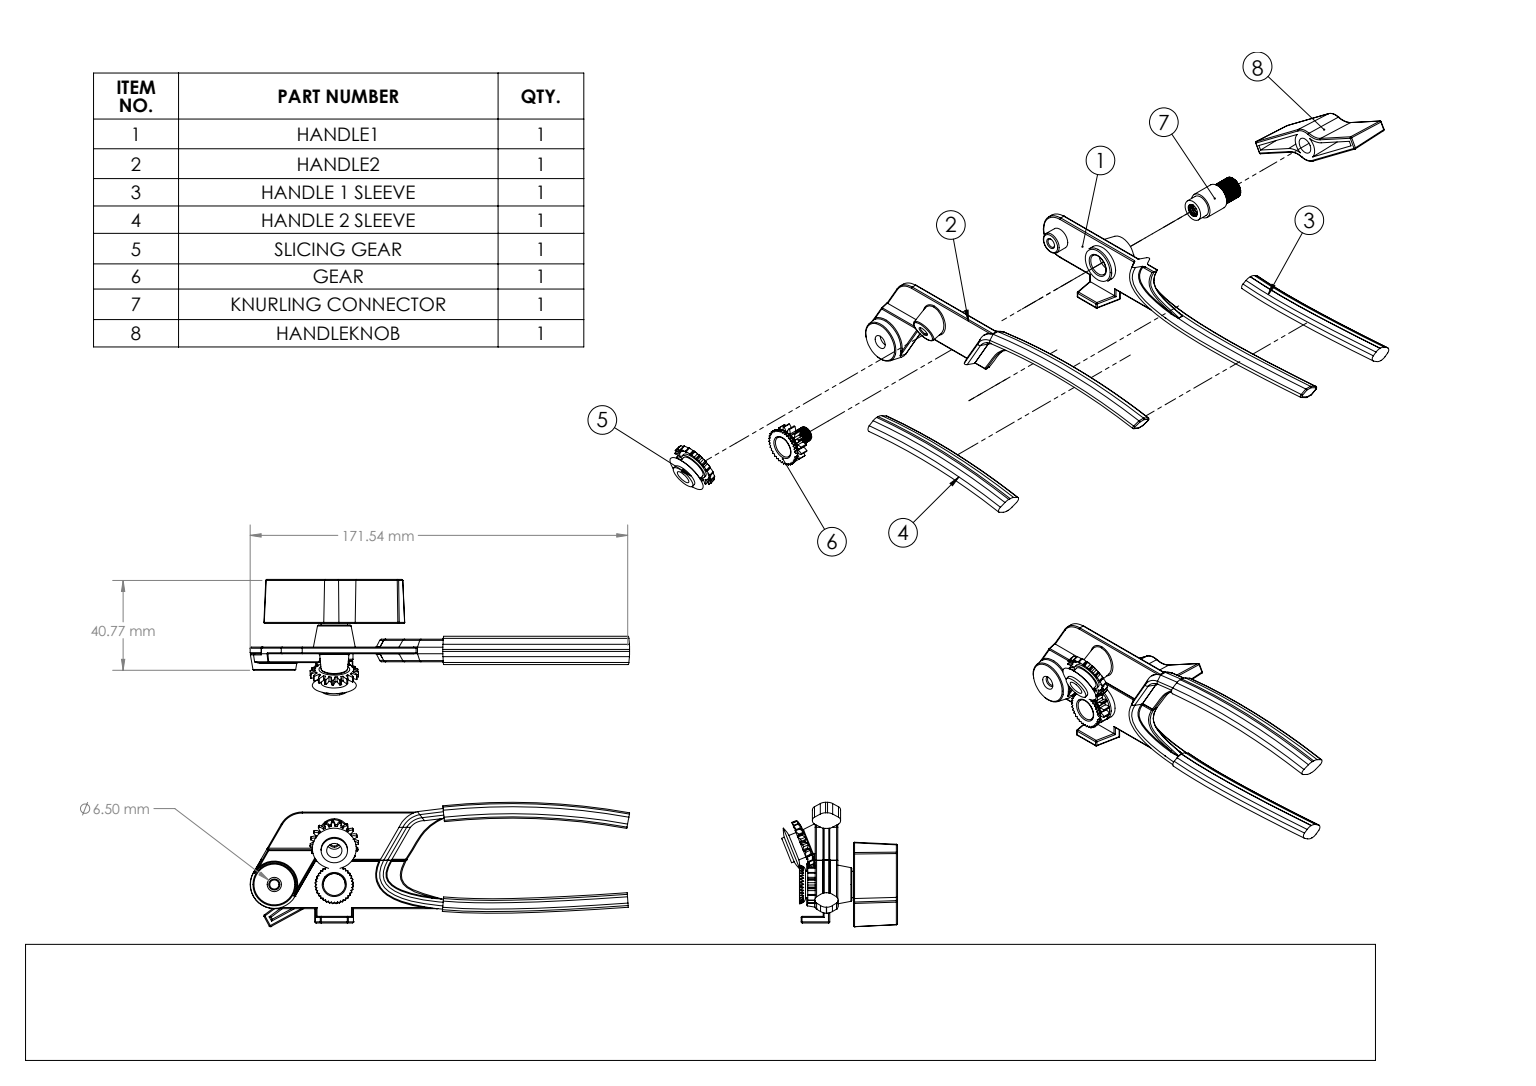
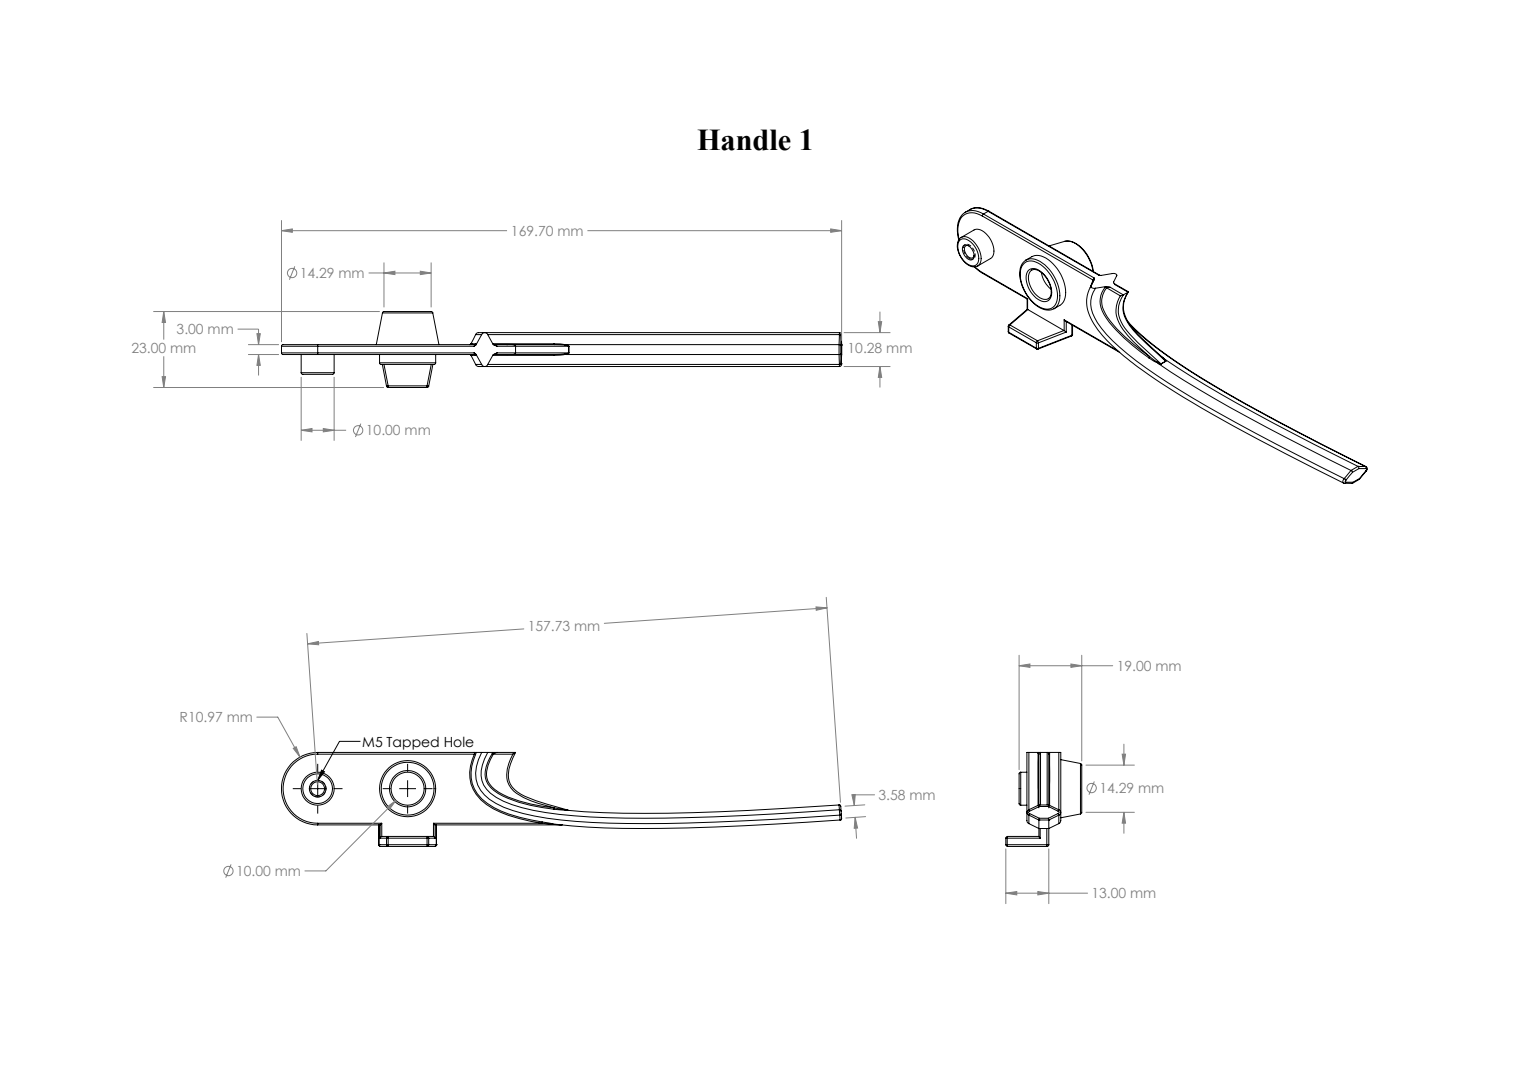
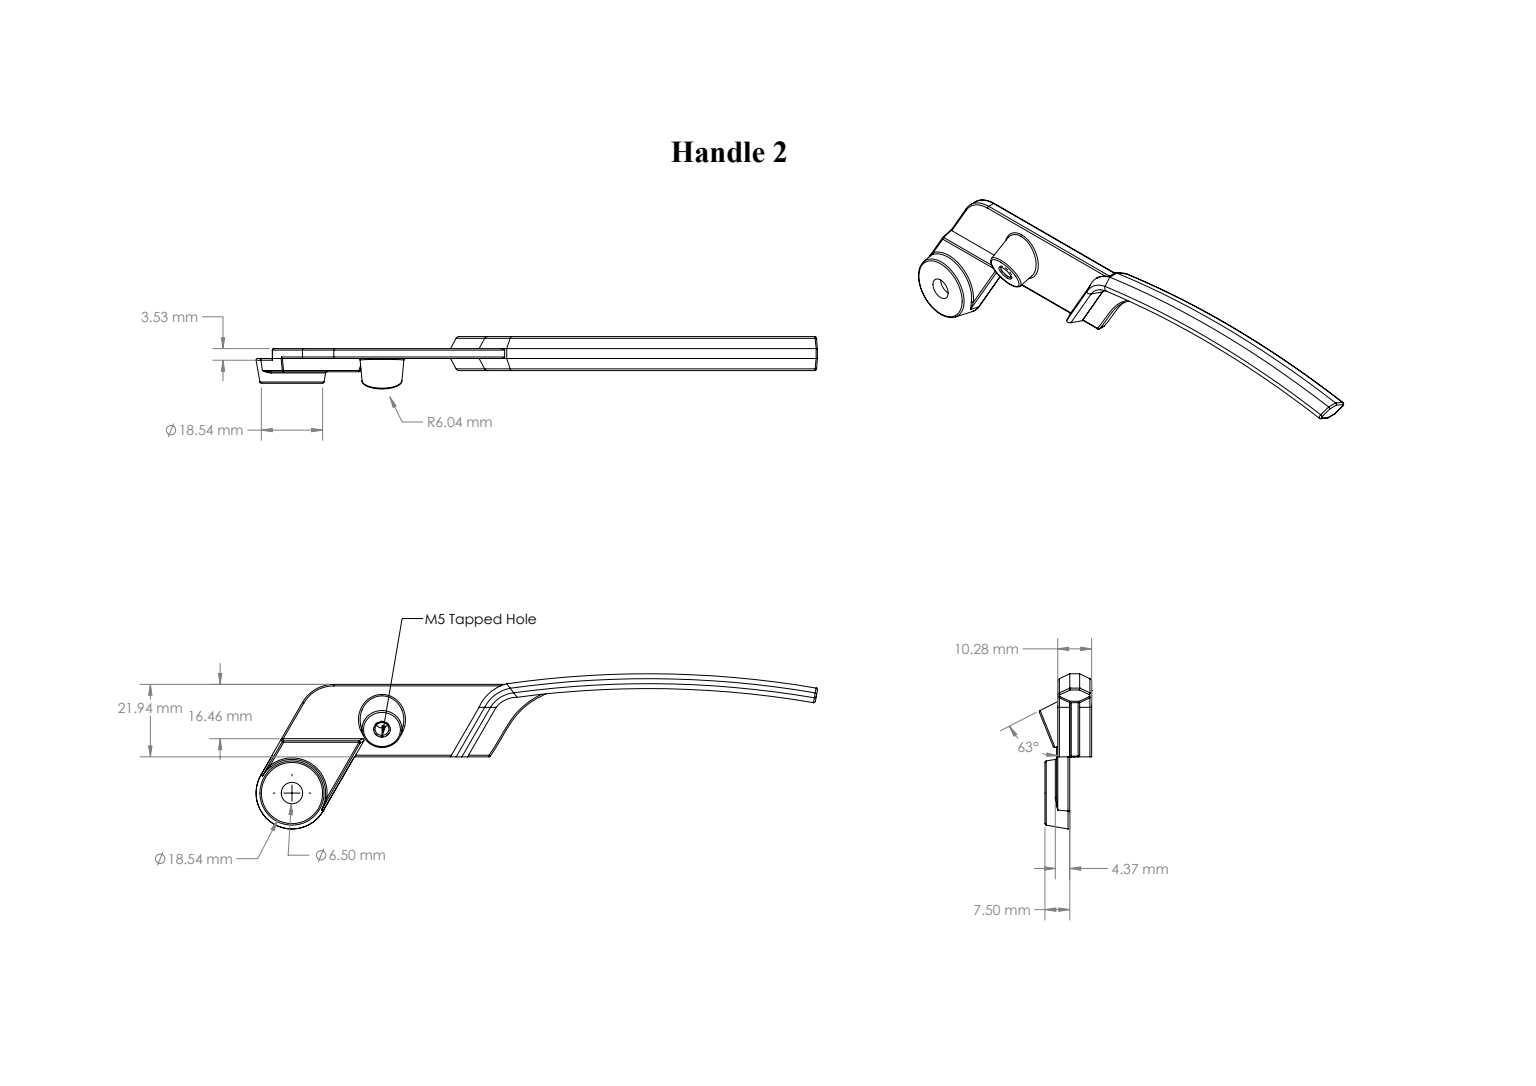
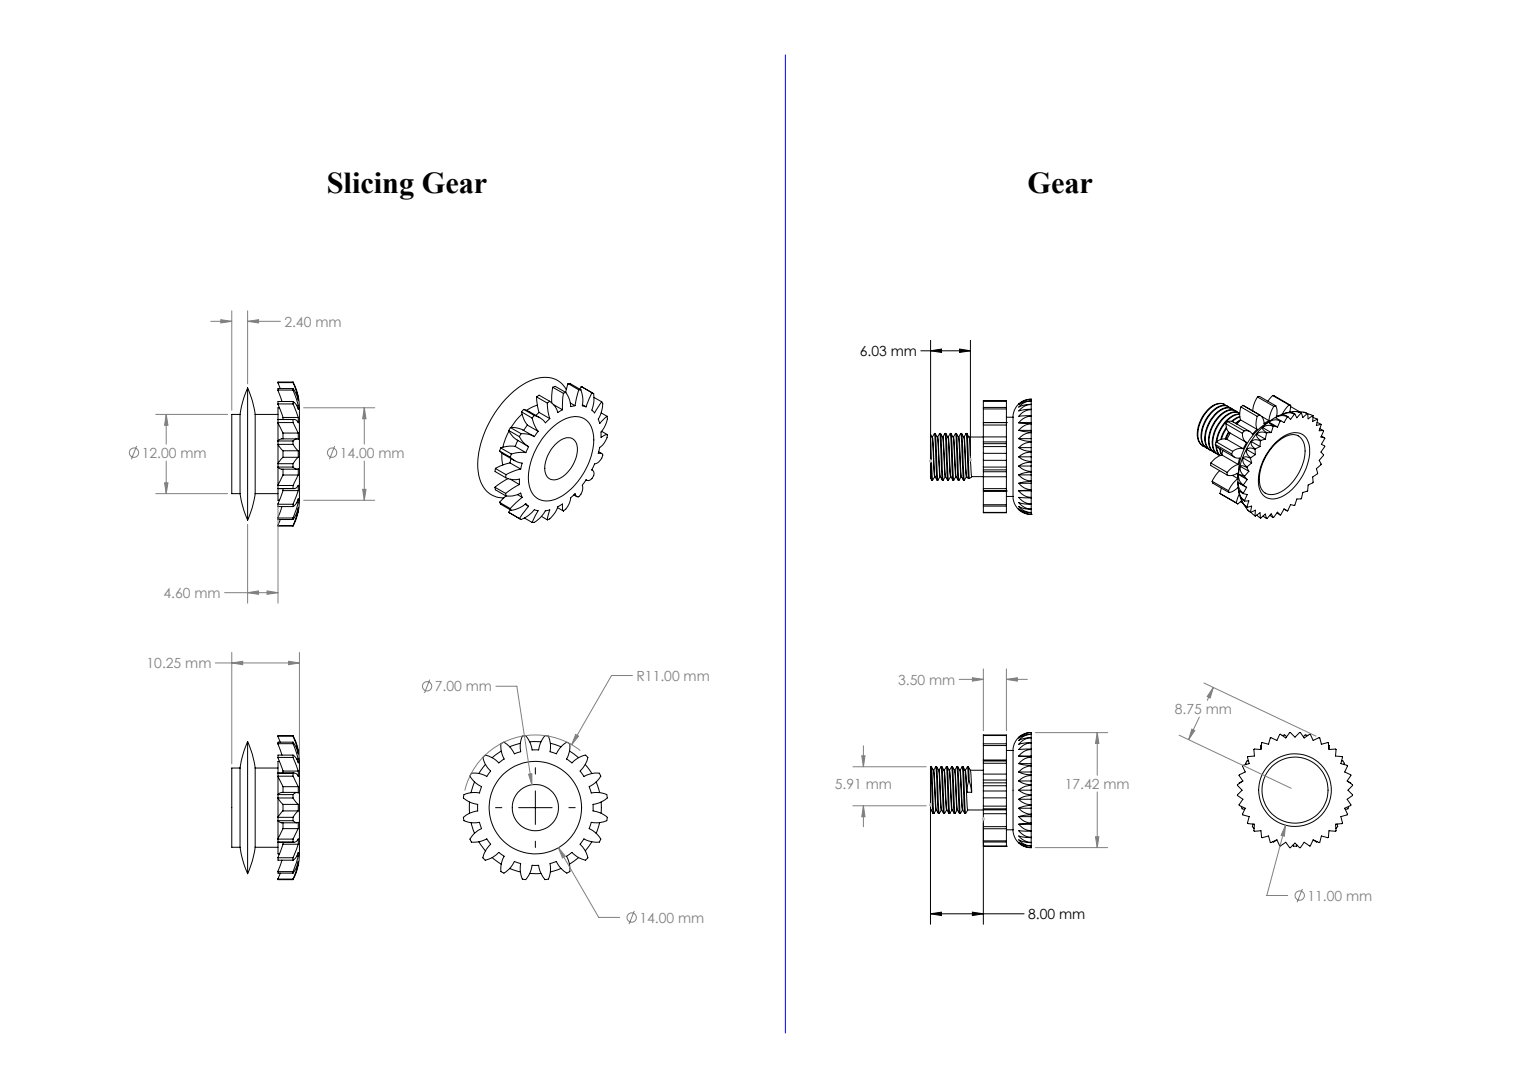
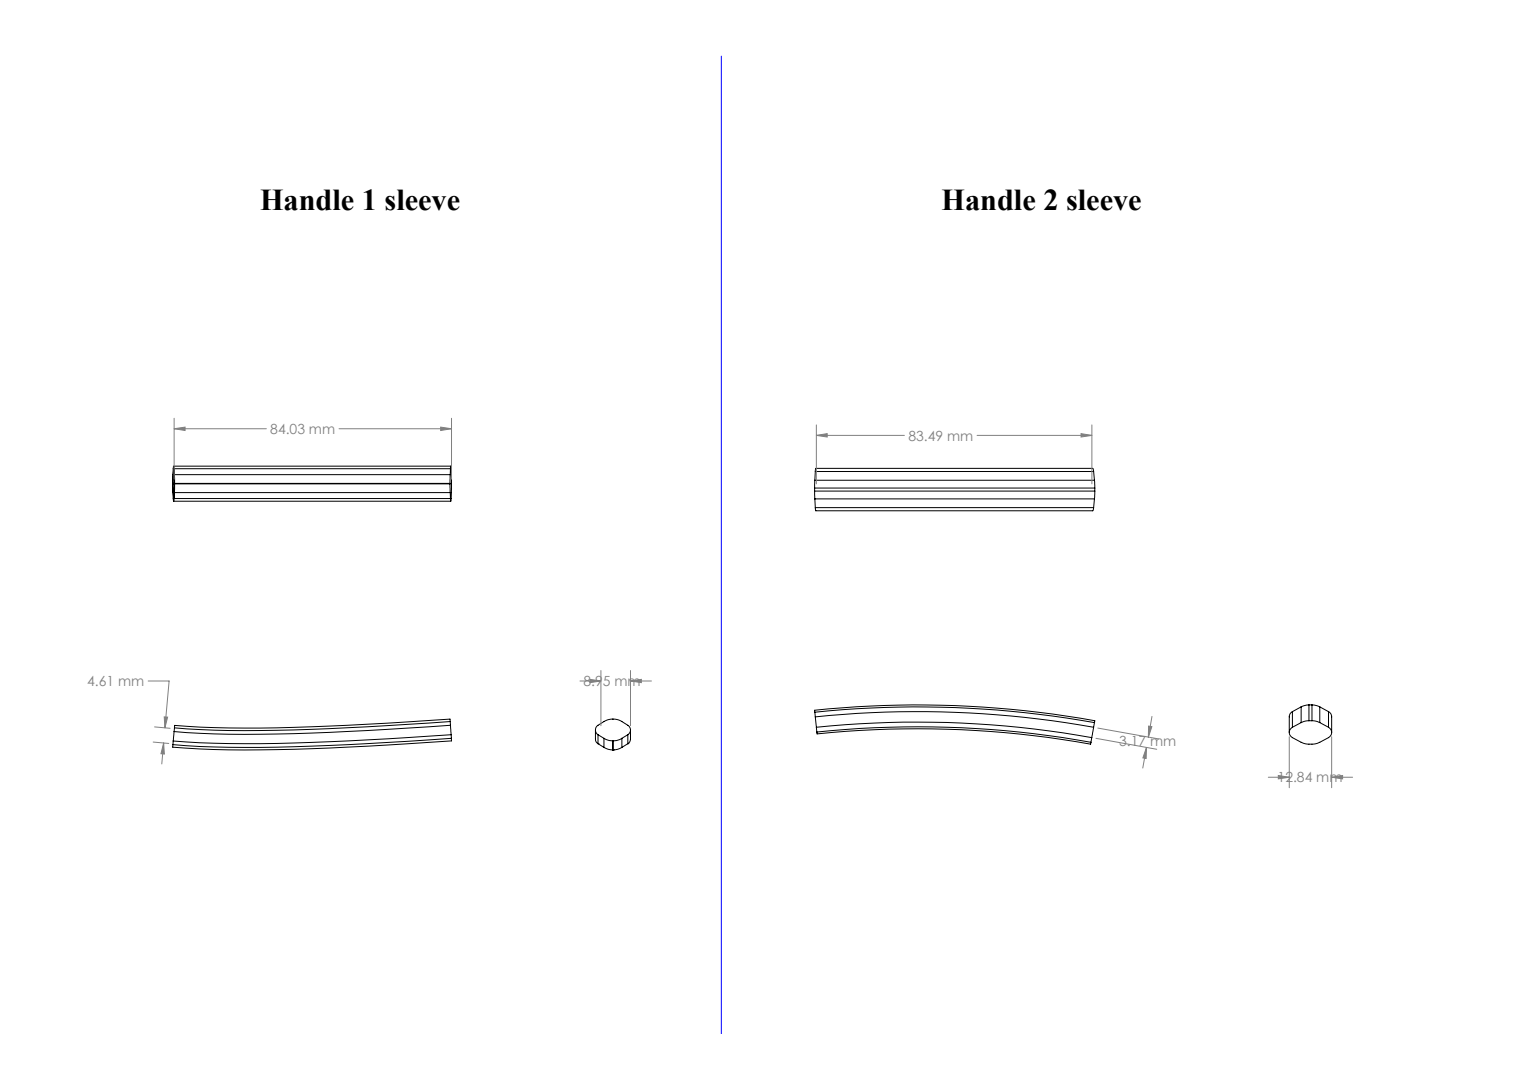
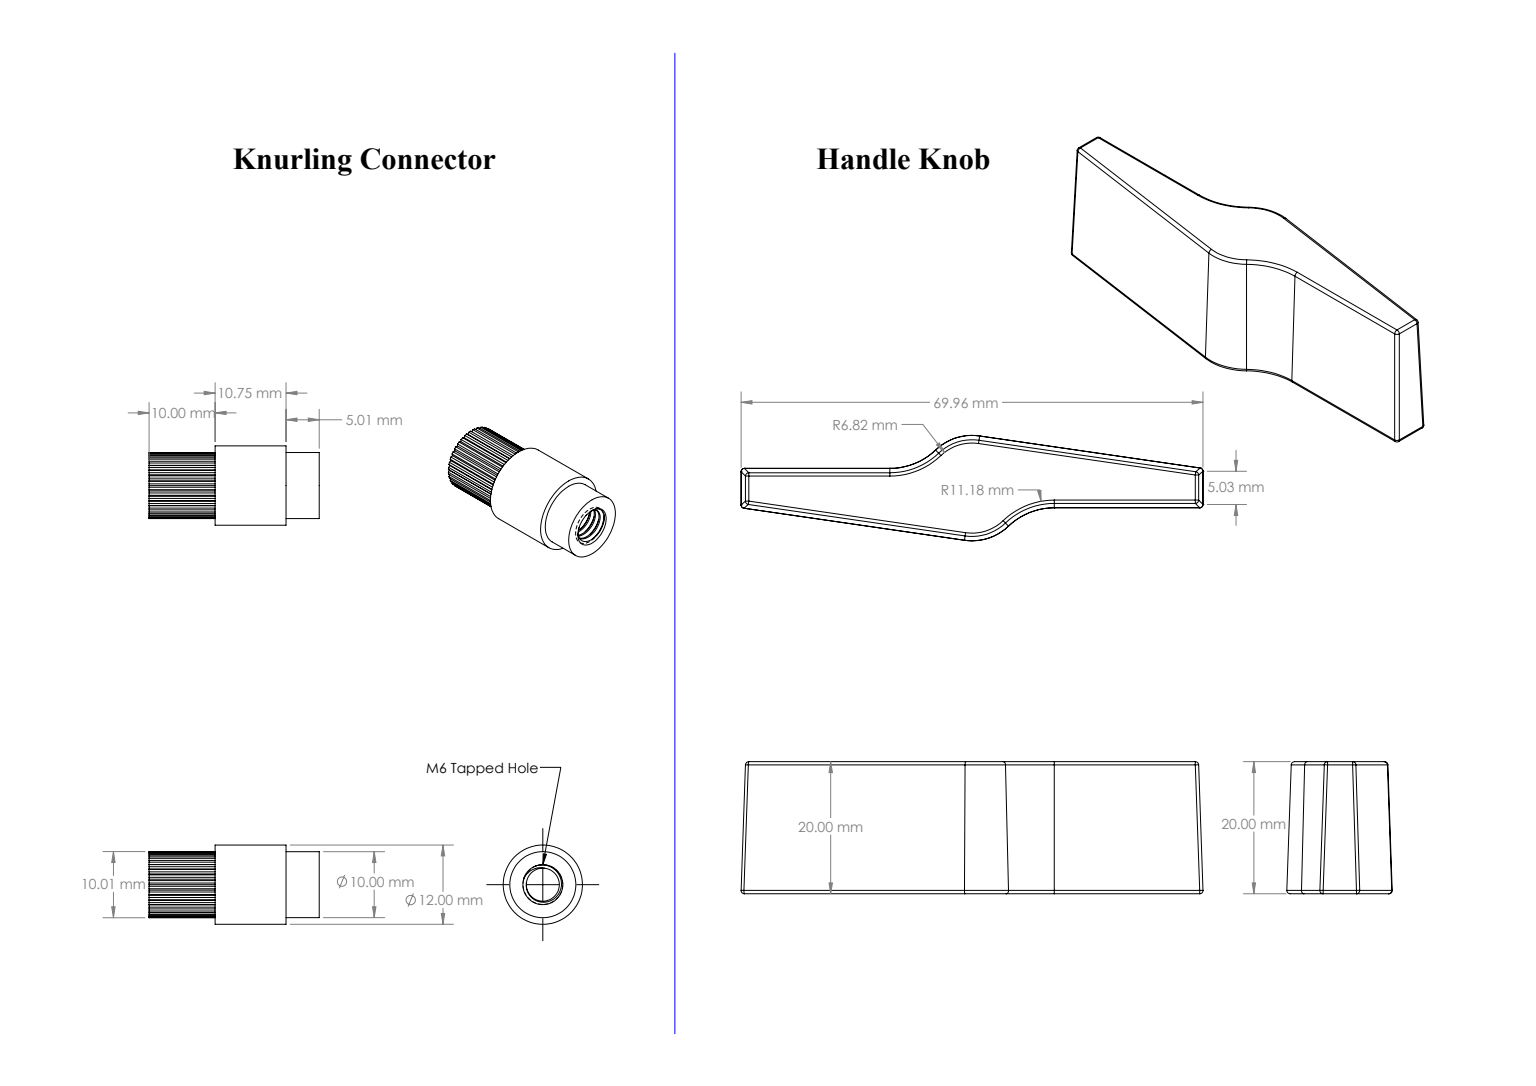
ISO-10303-21;
HEADER;
FILE_DESCRIPTION (('STEP AP203'),
    '1' );
FILE_NAME ('MAS-163',
    '2026-10-06T15:07:10',
    ( '' ),
    ( '' ),
    'SwSTEP 2.0',
    'SolidWorks 2024',
    '' );
FILE_SCHEMA (( 'AUTOMOTIVE_DESIGN' ));
ENDSEC;

DATA;
#1 = ADVANCED_FACE ( 'NONE', ( #10434 ), #18456, .F. ) ;
#2 = CARTESIAN_POINT ( 'NONE',  ( 54.89716490668163118, -3.628845007888942931, 0.07017451552782483226 ) ) ;
#3 = CARTESIAN_POINT ( 'NONE',  ( -8.000050800000000351, 3.673940397442060361E-16, 3.000000000000000444 ) ) ;
#4 = ORIENTED_EDGE ( 'NONE', *, *, #27611, .T. ) ;
#5 = DIRECTION ( 'NONE',  ( 1.000000000000000000, -0.000000000000000000, 0.000000000000000000 ) ) ;
#6 = EDGE_CURVE ( 'NONE', #31023, #30399, #20030, .T. ) ;
#7 = AXIS2_PLACEMENT_3D ( 'NONE', #248, #30174, #22638 ) ;
#8 = AXIS2_PLACEMENT_3D ( 'NONE', #3231, #13394, #23612 ) ;
#9 = APPLICATION_PROTOCOL_DEFINITION ( 'international standard', 'config_control_design', 1994, #20608 ) ;
#10 = CARTESIAN_POINT ( 'NONE',  ( 18.75828436641558028, -5.879118399717574661, -3.993434336035625254 ) ) ;
#11 = VERTEX_POINT ( 'NONE', #9811 ) ;
#12 = AXIS2_PLACEMENT_3D ( 'NONE', #13774, #23975, #1092 ) ;
#13 = SHAPE_REPRESENTATION ( 'Part5_knurlingConnector', ( #2865 ), #13509 ) ;
#14 = DIRECTION ( 'NONE',  ( 0.000000000000000000, 1.000000000000000000, 0.000000000000000000 ) ) ;
#15 = ORIENTED_EDGE ( 'NONE', *, *, #21559, .T. ) ;
#16 = CARTESIAN_POINT ( 'NONE',  ( -21.76338877130672245, 18.20021209127403239, 1.779283699008895159 ) ) ;
#18 = ORIENTED_EDGE ( 'NONE', *, *, #3562, .F. ) ;
#17 = CARTESIAN_POINT ( 'NONE',  ( 69.01456695820279208, -4.997110861600952525, -4.033870539711066350 ) ) ;
#19 = ORIENTED_EDGE ( 'NONE', *, *, #12026, .T. ) ;
#20 = CARTESIAN_POINT ( 'NONE',  ( -2.511343449419941365, -0.3178988483021044087, 3.024605502323848949 ) ) ;
#21 = CARTESIAN_POINT ( 'NONE',  ( 10.57125986779756843, 4.681538312723516171, 0.8254815157535410064 ) ) ;
#22 = DIRECTION ( 'NONE',  ( 0.000000000000000000, 1.000000000000000000, 0.000000000000000000 ) ) ;
#23 = EDGE_CURVE ( 'NONE', #10880, #2577, #7296, .T. ) ;
#24 = FACE_OUTER_BOUND ( 'NONE', #30613, .T. ) ;
#25 = CC_DESIGN_DATE_AND_TIME_ASSIGNMENT ( #14013, #6672, ( #1036 ) ) ;
#27 = ORIENTED_EDGE ( 'NONE', *, *, #10830, .T. ) ;
#26 = FACE_OUTER_BOUND ( 'NONE', #27997, .T. ) ;
#28 = DIRECTION ( 'NONE',  ( -1.000000000000000000, -0.000000000000000000, 0.000000000000000000 ) ) ;
#29 = CARTESIAN_POINT ( 'NONE',  ( 26.04699060503310193, 19.53185396608588320, 1.500000000000000000 ) ) ;
#30 = CARTESIAN_POINT ( 'NONE',  ( -3.423602242323041001, -10.69107769603132674, 1.500000000000237144 ) ) ;
#31 = CARTESIAN_POINT ( 'NONE',  ( 2.717504505341735932, -0.4236608596156870021, 1.500000000000000000 ) ) ;
#33 = ORIENTED_EDGE ( 'NONE', *, *, #17651, .T. ) ;
#32 = CARTESIAN_POINT ( 'NONE',  ( 107.5624060836778426, -18.99272400518356463, -4.497198431447757550 ) ) ;
#34 = DIRECTION ( 'NONE',  ( -0.000000000000000000, -0.000000000000000000, 1.000000000000000000 ) ) ;
#35 = AXIS2_PLACEMENT_3D ( 'NONE', #30229, #18289, #20649 ) ;
#36 = AXIS2_PLACEMENT_3D ( 'NONE', #29138, #6225, #23788 ) ;
#37 = B_SPLINE_CURVE_WITH_KNOTS ( 'NONE', 3,
 ( #24439, #32167, #19463, #16927, #1731, #20453, #20272, #30474 ),
 .UNSPECIFIED., .F., .F.,
 ( 4, 2, 2, 4 ),
 ( 2.304311362529957687E-07, 0.001227991214883143506, 0.001841871606756588465, 0.002455751998630033642 ),
 .UNSPECIFIED. ) ;
#38 = DIRECTION ( 'NONE',  ( 1.000000000000000000, -8.574039729943018344E-17, -0.000000000000000000 ) ) ;
#39 = CARTESIAN_POINT ( 'NONE',  ( 23.86000000273118715, -1.942864903642428587, -1.573300977624592756 ) ) ;
#40 = AXIS2_PLACEMENT_3D ( 'NONE', #21836, #32050, #26400 ) ;
#41 = EDGE_CURVE ( 'NONE', #3413, #15831, #25636, .T. ) ;
#42 = DIRECTION ( 'NONE',  ( 0.000000000000000000, 1.000000000000000000, 0.000000000000000000 ) ) ;
#43 = CARTESIAN_POINT ( 'NONE',  ( -8.000050800000000351, 0.000000000000000000, 0.000000000000000000 ) ) ;
#44 = CARTESIAN_POINT ( 'NONE',  ( -2.880987360464337677, -0.6119841066606566127, -1.499999999999999334 ) ) ;
#45 = VECTOR ( 'NONE', #11499, 1000.000000000000000 ) ;
#46 = EDGE_LOOP ( 'NONE', ( #17358, #23961, #2698, #31842 ) ) ;
#47 = DIRECTION ( 'NONE',  ( 0.000000000000000000, -0.4226182617406998299, -0.9063077870366498257 ) ) ;
#48 = LINE ( 'NONE', #23124, #20445 ) ;
#49 = CARTESIAN_POINT ( 'NONE',  ( -6.387550801365593500, 3.521866450007987037, 0.3701630799359328372 ) ) ;
#50 = ORIENTED_EDGE ( 'NONE', *, *, #20292, .T. ) ;
#51 = DIRECTION ( 'NONE',  ( 6.062761635205658338E-17, 0.7071067811865558994, -0.7071067811865391350 ) ) ;
#52 = AXIS2_PLACEMENT_3D ( 'NONE', #22887, #28230, #10168 ) ;
#53 = DIRECTION ( 'NONE',  ( 0.000000000000000000, -0.7071067811865380248, -0.7071067811865570096 ) ) ;
#54 = VECTOR ( 'NONE', #11765, 999.9999999999998863 ) ;
#55 = CARTESIAN_POINT ( 'NONE',  ( 2.117172266158220406, -1.242920418748501676, -0.9788672205888330202 ) ) ;
#56 = CARTESIAN_POINT ( 'NONE',  ( 19.46884934643044929, -15.80146560116522991, 1.000000000000000000 ) ) ;
#57 = EDGE_LOOP ( 'NONE', ( #2228, #29495, #10201, #20358 ) ) ;
#58 = CIRCLE ( 'NONE', #27352, 8.500000000000000000 ) ;
#59 = CIRCLE ( 'NONE', #14435, 12.62979293944910353 ) ;
#60 = CARTESIAN_POINT ( 'NONE',  ( -40.65244704454411107, -12.44919619934167088, 5.499999999999999112 ) ) ;
#61 = VERTEX_POINT ( 'NONE', #14078 ) ;
#62 = CARTESIAN_POINT ( 'NONE',  ( -2.655659815844460869, 0.1700350810717016214, 1.254089647469669000 ) ) ;
#64 = ORIENTED_EDGE ( 'NONE', *, *, #2032, .F. ) ;
#63 = DIRECTION ( 'NONE',  ( 0.000000000000000000, -0.000000000000000000, -1.000000000000000000 ) ) ;
#65 = ORIENTED_EDGE ( 'NONE', *, *, #16539, .T. ) ;
#66 = DIRECTION ( 'NONE',  ( 0.000000000000000000, -0.7071067811865455743, -0.7071067811865495711 ) ) ;
#67 = ADVANCED_FACE ( 'NONE', ( #1394 ), #31658, .F. ) ;
#68 = EDGE_LOOP ( 'NONE', ( #22629, #18065, #11744, #10106 ) ) ;
#70 = VECTOR ( 'NONE', #32626, 1000.000000000000000 ) ;
#69 = CARTESIAN_POINT ( 'NONE',  ( 5.612718761614564400, -7.013540705848206436, 4.279483796479000013 ) ) ;
#72 = VERTEX_POINT ( 'NONE', #1047 ) ;
#71 = DIRECTION ( 'NONE',  ( 0.000000000000000000, 0.9961946980917452121, 0.08715574274766296758 ) ) ;
#73 = CARTESIAN_POINT ( 'NONE',  ( 0.8174907777731121872, -3.242754804592638429, -1.762319835267122992 ) ) ;
#74 = CARTESIAN_POINT ( 'NONE',  ( 0.9232102171129921153, 0.000000000000000000, 4.522129901861157819 ) ) ;
#75 = CARTESIAN_POINT ( 'NONE',  ( 10.57125986779756843, -1.115095498423343878, 4.884328206559833241 ) ) ;
#76 = DIRECTION ( 'NONE',  ( -1.000000000000000000, -0.000000000000000000, -0.000000000000000000 ) ) ;
#77 = AXIS2_PLACEMENT_3D ( 'NONE', #24647, #7270, #1946 ) ;
#78 = DIRECTION ( 'NONE',  ( -0.000000000000000000, -0.000000000000000000, -1.000000000000000000 ) ) ;
#79 = CARTESIAN_POINT ( 'NONE',  ( 0.6738579927983930906, -5.220872085256825557, 1.499999999999999556 ) ) ;
#80 = FACE_OUTER_BOUND ( 'NONE', #3087, .T. ) ;
#81 = ADVANCED_FACE ( 'NONE', ( #26310 ), #21929, .F. ) ;
#82 = EDGE_CURVE ( 'NONE', #20879, #12815, #17217, .T. ) ;
#83 = AXIS2_PLACEMENT_3D ( 'NONE', #30124, #5184, #17706 ) ;
#84 = VECTOR ( 'NONE', #19365, 1000.000000000000227 ) ;
#85 = PLANE ( 'NONE',  #10726 ) ;
#86 = CARTESIAN_POINT ( 'NONE',  ( 101.9216173105994159, -5.769792427975438898, -0.07017451552783579571 ) ) ;
#87 = DIRECTION ( 'NONE',  ( 4.458171167563049465E-29, -1.000000000000000000, -5.782411586589359611E-15 ) ) ;
#88 = CARTESIAN_POINT ( 'NONE',  ( 54.64624227588102201, -3.635739347938791610, 0.02339150516273077324 ) ) ;
#89 = CIRCLE ( 'NONE', #23575, 2.099999999999997868 ) ;
#90 = EDGE_CURVE ( 'NONE', #31165, #31196, #18949, .T. ) ;
#91 = CIRCLE ( 'NONE', #29457, 2.999999999999999112 ) ;
#92 = CARTESIAN_POINT ( 'NONE',  ( 7.249760686538667009, -2.789499415801756586E-14, 8.014274990069656823 ) ) ;
#93 = CARTESIAN_POINT ( 'NONE',  ( 9.999999999999998224, -4.753758587302148619, -3.462581523170091167E-33 ) ) ;
#94 = ORIENTED_EDGE ( 'NONE', *, *, #25211, .F. ) ;
#95 = CARTESIAN_POINT ( 'NONE',  ( -5.787550801365593856, 0.3701630799359330593, -3.521866450007987037 ) ) ;
#96 = AXIS2_PLACEMENT_3D ( 'NONE', #16937, #1925, #32505 ) ;
#97 = VECTOR ( 'NONE', #5631, 999.9999999999998863 ) ;
#98 = FACE_OUTER_BOUND ( 'NONE', #358, .T. ) ;
#99 = CARTESIAN_POINT ( 'NONE',  ( 2.274274201627632941, 1.975651141464536797, -10.82112760146234720 ) ) ;
#100 = ORIENTED_EDGE ( 'NONE', *, *, #5872, .F. ) ;
#101 = CARTESIAN_POINT ( 'NONE',  ( 18.76371685221734964, -5.818394111045739336, -4.091315477141358237 ) ) ;
#102 = CARTESIAN_POINT ( 'NONE',  ( 5.377543748152548986, -5.151476664237435443, -6.139290821770307716 ) ) ;
#103 = ORIENTED_EDGE ( 'NONE', *, *, #2188, .F. ) ;
#104 = DIRECTION ( 'NONE',  ( 0.000000000000000000, 0.000000000000000000, 1.000000000000000000 ) ) ;
#105 = APPROVAL_ROLE ( '' ) ;
#106 = AXIS2_PLACEMENT_3D ( 'NONE', #14206, #26936, #32117 ) ;
#108 = ORIENTED_EDGE ( 'NONE', *, *, #26018, .T. ) ;
#107 = CARTESIAN_POINT ( 'NONE',  ( 13.65718777918027271, -19.09288791508984318, -4.522129901861166701 ) ) ;
#109 = ORIENTED_EDGE ( 'NONE', *, *, #15136, .T. ) ;
#110 = DIRECTION ( 'NONE',  ( -0.000000000000000000, -1.000000000000000000, -0.000000000000000000 ) ) ;
#111 = AXIS2_PLACEMENT_3D ( 'NONE', #29332, #11295, #4258 ) ;
#112 = VERTEX_POINT ( 'NONE', #19260 ) ;
#113 = CARTESIAN_POINT ( 'NONE',  ( 107.9870634758426746, -17.88307938695580646, -4.509668461024523012 ) ) ;
#115 = VERTEX_POINT ( 'NONE', #32150 ) ;
#114 = LINE ( 'NONE', #298, #18162 ) ;
#116 = CIRCLE ( 'NONE', #24119, 8.500000000000000000 ) ;
#117 = LINE ( 'NONE', #10625, #6451 ) ;
#118 = CARTESIAN_POINT ( 'NONE',  ( 0.000000000000000000, 0.000000000000000000, 0.000000000000000000 ) ) ;
#119 = VECTOR ( 'NONE', #15199, 1000.000000000000114 ) ;
#120 = CARTESIAN_POINT ( 'NONE',  ( 21.54063306425963020, -21.75686058823632862, -1.475739251284730269 ) ) ;
#121 = CARTESIAN_POINT ( 'NONE',  ( 108.6457025336241031, 16.11621187055573046, -2.334455007174250696 ) ) ;
#122 = VECTOR ( 'NONE', #10002, 1000.000000000000000 ) ;
#123 = ADVANCED_FACE ( 'NONE', ( #13736 ), #14864, .T. ) ;
#124 = ORIENTED_EDGE ( 'NONE', *, *, #31376, .T. ) ;
#125 = CARTESIAN_POINT ( 'NONE',  ( -4.599999999999996980, 0.000000000000000000, -10.00000000000000178 ) ) ;
#126 = CARTESIAN_POINT ( 'NONE',  ( 107.7308922075239082, 16.67966155151041363, -1.408250966677084381 ) ) ;
#127 = CARTESIAN_POINT ( 'NONE',  ( -7.000050800000000351, 7.347880794884120722E-16, 6.000000000000000888 ) ) ;
#128 = DIRECTION ( 'NONE',  ( 0.000000000000000000, 0.000000000000000000, 1.000000000000000000 ) ) ;
#129 = EDGE_CURVE ( 'NONE', #32786, #20668, #15618, .T. ) ;
#130 = EDGE_CURVE ( 'NONE', #2062, #25766, #16915, .T. ) ;
#131 = CARTESIAN_POINT ( 'NONE',  ( -35.00045521830035966, -0.01303574654798572707, 2.568038078148746184 ) ) ;
#132 = CIRCLE ( 'NONE', #12926, 5.009999999999999787 ) ;
#133 = CARTESIAN_POINT ( 'NONE',  ( -6.962942409646511344, 7.727249047114547632E-16, -2.999999999999999556 ) ) ;
#134 = CARTESIAN_POINT ( 'NONE',  ( 3.063284526839887167, 0.000000000000000000, 0.000000000000000000 ) ) ;
#135 = PLANE ( 'NONE',  #7597 ) ;
#136 = VERTEX_POINT ( 'NONE', #4209 ) ;
#137 = VECTOR ( 'NONE', #28016, 1000.000000000000000 ) ;
#138 = VECTOR ( 'NONE', #31382, 1000.000000000000114 ) ;
#139 = CARTESIAN_POINT ( 'NONE',  ( -5.712550801365594566, -1.088641768524163389, -3.675193018007246071 ) ) ;
#140 = VERTEX_POINT ( 'NONE', #15060 ) ;
#141 = VECTOR ( 'NONE', #13151, 1000.000000000000000 ) ;
#142 = CARTESIAN_POINT ( 'NONE',  ( -4.654531657079157725, -2.846291840500172921, -1.545410377633947618 ) ) ;
#143 = AXIS2_PLACEMENT_3D ( 'NONE', #19996, #12938, #271 ) ;
#144 = AXIS2_PLACEMENT_3D ( 'NONE', #9896, #22118, #20259 ) ;
#145 = CARTESIAN_POINT ( 'NONE',  ( 108.0191169540316167, 18.28461066811921754, 4.532506712702909724 ) ) ;
#146 = CARTESIAN_POINT ( 'NONE',  ( 0.4088345642745362385, -8.504920321588055998, 1.772058741665319292 ) ) ;
#147 = CARTESIAN_POINT ( 'NONE',  ( 13.44509804309065615, -13.81913516398266495, 1.499999999999168887 ) ) ;
#148 = AXIS2_PLACEMENT_3D ( 'NONE', #28905, #8200, #6010 ) ;
#149 = ORIENTED_EDGE ( 'NONE', *, *, #3090, .F. ) ;
#150 = CARTESIAN_POINT ( 'NONE',  ( -4.187842409712542721E-16, -4.884328206559843011, 1.115095498423292142 ) ) ;
#151 = AXIS2_PLACEMENT_3D ( 'NONE', #26577, #18412, #21086 ) ;
#152 = ORIENTED_EDGE ( 'NONE', *, *, #16988, .F. ) ;
#153 = CARTESIAN_POINT ( 'NONE',  ( 2.592584512317751333, -0.9926283730658966853, -10.27797909967270584 ) ) ;
#154 = PERSON_AND_ORGANIZATION ( #6766, #25292 ) ;
#155 = CARTESIAN_POINT ( 'NONE',  ( 85.03119751210560651, -5.129410398413424055, 4.093303008813728994 ) ) ;
#156 = AXIS2_PLACEMENT_3D ( 'NONE', #22378, #9498, #26916 ) ;
#157 = CARTESIAN_POINT ( 'NONE',  ( 3.499999999999999556, 0.000000000000000000, 0.000000000000000000 ) ) ;
#158 = AXIS2_PLACEMENT_3D ( 'NONE', #14423, #2390, #20600 ) ;
#160 = CARTESIAN_POINT ( 'NONE',  ( 56.97280603064898941, -277.2763395528616002, 4.999054092451761022 ) ) ;
#159 = CARTESIAN_POINT ( 'NONE',  ( 10.00000000000000000, 2.718385644597173023, 4.208382051008202396 ) ) ;
#161 = EDGE_CURVE ( 'NONE', #26388, #31289, #10295, .T. ) ;
#162 = AXIS2_PLACEMENT_3D ( 'NONE', #23286, #22786, #32990 ) ;
#163 = ORIENTED_EDGE ( 'NONE', *, *, #25130, .F. ) ;
#164 = VECTOR ( 'NONE', #17000, 1000.000000000000114 ) ;
#165 = CARTESIAN_POINT ( 'NONE',  ( 0.7632845268449858223, 8.461683424485162419, -2.223716399040675196 ) ) ;
#166 = CARTESIAN_POINT ( 'NONE',  ( 2.857987933988741958, 0.6743480930095439030, 9.536462466408304195 ) ) ;
#167 = VECTOR ( 'NONE', #10719, 1000.000000000000114 ) ;
#168 = CARTESIAN_POINT ( 'NONE',  ( 24.73500000136559507, 3.156283516753366047, 0.9349337715887203748 ) ) ;
#169 = CIRCLE ( 'NONE', #6539, 2.099999999999997868 ) ;
#170 = CARTESIAN_POINT ( 'NONE',  ( 10.98818895950636509, -14.84697401622043600, -1.499999999999999556 ) ) ;
#171 = EDGE_CURVE ( 'NONE', #23760, #9712, #9390, .T. ) ;
#173 = ORIENTED_EDGE ( 'NONE', *, *, #21181, .F. ) ;
#172 = CARTESIAN_POINT ( 'NONE',  ( 0.8174570305809125692, -9.170357625429589987, 1.500000000000000444 ) ) ;
#174 = CARTESIAN_POINT ( 'NONE',  ( -5.212550801365593678, -1.828967928396026510, 3.368539882008728004 ) ) ;
#175 = LINE ( 'NONE', #20570, #28869 ) ;
#176 = B_SPLINE_CURVE_WITH_KNOTS ( 'NONE', 3,
 ( #7908, #5090, #2742, #23440, #17780, #10075, #13097, #30687, #7762, #30496, #23136, #15414 ),
 .UNSPECIFIED., .F., .F.,
 ( 4, 2, 2, 2, 2, 4 ),
 ( -5.999999993276212224E-08, 0.0005421711927698825593, 0.0008132867891547902132, 0.001084402385539697759, 0.001626633578309510247, 0.002168864771079322736 ),
 .UNSPECIFIED. ) ;
#177 = CARTESIAN_POINT ( 'NONE',  ( 5.377543748152548986, -6.139290821770289064, 5.151476664237455871 ) ) ;
#178 = EDGE_CURVE ( 'NONE', #11731, #23666, #11346, .T. ) ;
#179 =( GEOMETRIC_REPRESENTATION_CONTEXT ( 3 ) GLOBAL_UNCERTAINTY_ASSIGNED_CONTEXT ( ( #3915 ) ) GLOBAL_UNIT_ASSIGNED_CONTEXT ( ( #27348, #27672, #7131 ) ) REPRESENTATION_CONTEXT ( 'NONE', 'WORKASPACE' ) );
#180 = ORIENTED_EDGE ( 'NONE', *, *, #13228, .F. ) ;
#182 = EDGE_LOOP ( 'NONE', ( #4676, #19441, #6640, #3021 ) ) ;
#181 = CARTESIAN_POINT ( 'NONE',  ( -2.598264985223428969, 0.000000000000000000, 5.684322216989629695 ) ) ;
#183 = EDGE_CURVE ( 'NONE', #26433, #28176, #18018, .T. ) ;
#184 = AXIS2_PLACEMENT_3D ( 'NONE', #31855, #21799, #29506 ) ;
#185 = LINE ( 'NONE', #10366, #12356 ) ;
#186 = CARTESIAN_POINT ( 'NONE',  ( 107.7222261516258612, 19.48138685844068974, -4.344084370466780420 ) ) ;
#187 = EDGE_CURVE ( 'NONE', #21614, #30476, #10440, .T. ) ;
#188 = CARTESIAN_POINT ( 'NONE',  ( 23.67250000136559507, 3.024605502323846729, -0.3178988483021056854 ) ) ;
#189 = CARTESIAN_POINT ( 'NONE',  ( 102.9885081044300534, -6.698322160490901567, -0.07017451552781736601 ) ) ;
#190 = LINE ( 'NONE', #18394, #23629 ) ;
#191 = VECTOR ( 'NONE', #32403, 1000.000000000000000 ) ;
#192 = CARTESIAN_POINT ( 'NONE',  ( 2.326025872504024150, -9.559203939530167560, 5.234065033669340394 ) ) ;
#193 = PRODUCT_DEFINITION_SHAPE ( 'NONE', 'NONE',  #33098 ) ;
#194 = CIRCLE ( 'NONE', #7673, 0.5000000000000004441 ) ;
#195 = CARTESIAN_POINT ( 'NONE',  ( 3.499999999999999556, 0.000000000000000000, 0.000000000000000000 ) ) ;
#196 = DIRECTION ( 'NONE',  ( -0.000000000000000000, -0.000000000000000000, 1.000000000000000000 ) ) ;
#197 = ORIENTED_EDGE ( 'NONE', *, *, #20307, .T. ) ;
#198 = CARTESIAN_POINT ( 'NONE',  ( 28.66386174151161370, -4.482150724175043344, 2.184956778824117762 ) ) ;
#199 = AXIS2_PLACEMENT_3D ( 'NONE', #1341, #6668, #6487 ) ;
#201 = EDGE_CURVE ( 'NONE', #32996, #24872, #8151, .T. ) ;
#200 = AXIS2_PLACEMENT_3D ( 'NONE', #7022, #17038, #24913 ) ;
#202 = B_SPLINE_CURVE_WITH_KNOTS ( 'NONE', 3,
 ( #27500, #19992, #25480, #30192, #2590, #12755, #27322, #4443 ),
 .UNSPECIFIED., .F., .F.,
 ( 4, 2, 2, 4 ),
 ( 0.000000000000000000, 0.5000000000000000000, 0.7500000000000000000, 1.000000000000000000 ),
 .UNSPECIFIED. ) ;
#203 = CIRCLE ( 'NONE', #12966, 11.00000000000000000 ) ;
#204 = COORDINATED_UNIVERSAL_TIME_OFFSET ( 0, 0, .AHEAD. ) ;
#205 = CARTESIAN_POINT ( 'NONE',  ( 101.9216173105994443, -5.769792427975428240, -0.07017451552783622593 ) ) ;
#206 = EDGE_LOOP ( 'NONE', ( #7867, #23805, #1516, #15326 ) ) ;
#207 = DIRECTION ( 'NONE',  ( -1.000000000000000000, 8.574039729943018344E-17, -0.000000000000000000 ) ) ;
#208 = ORIENTED_EDGE ( 'NONE', *, *, #25908, .T. ) ;
#209 = DIRECTION ( 'NONE',  ( -0.9975973382524639943, -0.06927878976713693071, 0.000000000000000000 ) ) ;
#211 = ORIENTED_EDGE ( 'NONE', *, *, #28572, .F. ) ;
#210 = CARTESIAN_POINT ( 'NONE',  ( 40.87780399789884456, -5.761808403395388467, -4.013697493846343889 ) ) ;
#212 = ORIENTED_EDGE ( 'NONE', *, *, #20307, .F. ) ;
#213 = CARTESIAN_POINT ( 'NONE',  ( 0.000000000000000000, 9.620177616658057929, -5.227991826303984624 ) ) ;
#214 = CARTESIAN_POINT ( 'NONE',  ( 0.7212198416586443894, 5.676697589981204217, -6.922088825865619022 ) ) ;
#215 = DIRECTION ( 'NONE',  ( 7.023442172597920956E-17, 0.8191520442889983489, -0.5735764363510366115 ) ) ;
#216 = CYLINDRICAL_SURFACE ( 'NONE', #29485, 8.749000000000002331 ) ;
#218 = ORIENTED_EDGE ( 'NONE', *, *, #6090, .F. ) ;
#217 = CARTESIAN_POINT ( 'NONE',  ( 22.29750000273118715, 2.594547506269380133, 0.7685399846772031918 ) ) ;
#219 = VECTOR ( 'NONE', #6570, 1000.000000000000000 ) ;
#220 = CARTESIAN_POINT ( 'NONE',  ( 107.5617944031221640, -18.98359742639815551, 4.522129901861158707 ) ) ;
#221 = DIRECTION ( 'NONE',  ( 3.623545766764223251E-17, 0.4226182617407006070, -0.9063077870366493816 ) ) ;
#222 = CARTESIAN_POINT ( 'NONE',  ( 3.557967483062660641, -17.13335440830369194, 1.747754005074379169 ) ) ;
#224 = ADVANCED_FACE ( 'NONE', ( #25945 ), #18072, .T. ) ;
#223 = CARTESIAN_POINT ( 'NONE',  ( 24.11000000136559862, -3.156283516753370044, -0.9349337715887220401 ) ) ;
#225 = AXIS2_PLACEMENT_3D ( 'NONE', #7662, #15180, #20362 ) ;
#226 = CARTESIAN_POINT ( 'NONE',  ( 9.101556641444268791, 0.000000000000000000, 0.000000000000000000 ) ) ;
#228 = VERTEX_POINT ( 'NONE', #15742 ) ;
#227 = FACE_OUTER_BOUND ( 'NONE', #31998, .T. ) ;
#229 = EDGE_CURVE ( 'NONE', #7402, #25225, #10396, .T. ) ;
#230 = LINE ( 'NONE', #2912, #2926 ) ;
#231 = AXIS2_PLACEMENT_3D ( 'NONE', #18970, #26981, #26340 ) ;
#232 = CARTESIAN_POINT ( 'NONE',  ( 2.274274201627632053, 10.82112760146237029, 1.975651141464422000 ) ) ;
#233 = CARTESIAN_POINT ( 'NONE',  ( 22.67250000136559507, 2.363507492473148286, 1.913930629741525058 ) ) ;
#234 = LOCAL_TIME ( 16, 7, 10.00000000000000000, #9845 ) ;
#235 = EDGE_CURVE ( 'NONE', #10254, #1604, #2904, .T. ) ;
#236 = DIRECTION ( 'NONE',  ( -1.000000000000000000, 0.000000000000000000, 0.000000000000000000 ) ) ;
#237 = CARTESIAN_POINT ( 'NONE',  ( 6.356381451270080696, 8.587653982362812854, -0.5733789922931548100 ) ) ;
#238 = CARTESIAN_POINT ( 'NONE',  ( 18.75828436641558028, -5.879118399717575549, 3.993434336035622589 ) ) ;
#239 = ORIENTED_EDGE ( 'NONE', *, *, #30794, .T. ) ;
#240 = PLANE ( 'NONE',  #32748 ) ;
#241 = DIRECTION ( 'NONE',  ( 0.4999999999999970579, -0.09052430460833674197, 0.8612812260087757688 ) ) ;
#242 = CARTESIAN_POINT ( 'NONE',  ( -2.537550801365593411, 1.828967928396027398, -3.368539882008727115 ) ) ;
#243 = ORIENTED_EDGE ( 'NONE', *, *, #2990, .F. ) ;
#244 = EDGE_CURVE ( 'NONE', #31304, #5929, #3201, .T. ) ;
#245 =( BOUNDED_CURVE ( )  B_SPLINE_CURVE ( 3, ( #13031, #23237, #341, #27192 ),
 .UNSPECIFIED., .F., .F. ) 
 B_SPLINE_CURVE_WITH_KNOTS ( ( 4, 4 ),
 ( 0.000000000000000000, 1.570796326794914100 ),
 .UNSPECIFIED. ) 
 CURVE ( )  GEOMETRIC_REPRESENTATION_ITEM ( )  RATIONAL_B_SPLINE_CURVE ( ( 1.000000000000000000, 0.8047378541243608296, 0.8047378541243608296, 1.000000000000000000 ) ) 
 REPRESENTATION_ITEM ( '' )  );
#246 = AXIS2_PLACEMENT_3D ( 'NONE', #21103, #12004, #13369 ) ;
#247 = CARTESIAN_POINT ( 'NONE',  ( 10.57125986779756843, 0.8254815157535864145, -4.681538312723508177 ) ) ;
#248 = CARTESIAN_POINT ( 'NONE',  ( 3.249999999999999556, 9.241976615262160522, -1.699438267350404930 ) ) ;
#249 = CARTESIAN_POINT ( 'NONE',  ( 72.52374898135332160, -19.78015497550546442, -4.522129901861164925 ) ) ;
#250 = DIRECTION ( 'NONE',  ( 0.000000000000000000, 0.000000000000000000, 1.000000000000000000 ) ) ;
#251 = ORIENTED_EDGE ( 'NONE', *, *, #16628, .F. ) ;
#252 = LINE ( 'NONE', #7401, #30475 ) ;
#253 = ORIENTED_EDGE ( 'NONE', *, *, #2293, .F. ) ;
#254 = CARTESIAN_POINT ( 'NONE',  ( -2.745055912661534592, -0.1926413909284909742, 1.404235515125175970 ) ) ;
#256 = VERTEX_POINT ( 'NONE', #8036 ) ;
#255 = DIRECTION ( 'NONE',  ( 0.000000000000000000, -1.000000000000000000, 0.000000000000000000 ) ) ;
#257 = EDGE_LOOP ( 'NONE', ( #26300, #26585, #23410, #1568 ) ) ;
#258 = DIRECTION ( 'NONE',  ( 0.000000000000000000, 0.000000000000000000, -1.000000000000000000 ) ) ;
#259 = CC_DESIGN_APPROVAL ( #32320, ( #27464 ) ) ;
#260 = ORIENTED_EDGE ( 'NONE', *, *, #26605, .T. ) ;
#261 = CARTESIAN_POINT ( 'NONE',  ( -8.000050800000000351, 3.673940397442060361E-16, 3.000000000000000444 ) ) ;
#263 = ORIENTED_EDGE ( 'NONE', *, *, #4868, .T. ) ;
#262 = CARTESIAN_POINT ( 'NONE',  ( 102.9885081044300534, -6.698322160490901567, 0.07017451552781736601 ) ) ;
#264 = VERTEX_POINT ( 'NONE', #28449 ) ;
#265 = CARTESIAN_POINT ( 'NONE',  ( -5.500050800000000351, -2.983565686104819648, -0.3135853898029605791 ) ) ;
#266 = DIRECTION ( 'NONE',  ( 0.000000000000000000, 0.000000000000000000, -1.000000000000000000 ) ) ;
#267 = EDGE_CURVE ( 'NONE', #17721, #28345, #13209, .T. ) ;
#268 = CARTESIAN_POINT ( 'NONE',  ( 7.249760686538667009, 8.385837730238846314E-14, -8.014274990069656823 ) ) ;
#269 = FACE_OUTER_BOUND ( 'NONE', #21675, .T. ) ;
#270 = VECTOR ( 'NONE', #15790, 999.9999999999998863 ) ;
#271 = DIRECTION ( 'NONE',  ( 1.000000000000000000, 0.000000000000000000, 0.000000000000000000 ) ) ;
#272 = PLANE ( 'NONE',  #12904 ) ;
#273 = LINE ( 'NONE', #20493, #10381 ) ;
#274 = CARTESIAN_POINT ( 'NONE',  ( 3.566513200368869096, -17.47573827932033197, 1.500000000000000000 ) ) ;
#275 = CARTESIAN_POINT ( 'NONE',  ( 18.80941384712784981, -5.307593421039076276, 3.636029349014984202 ) ) ;
#276 = DIRECTION ( 'NONE',  ( 0.000000000000000000, -1.000000000000000000, 0.000000000000000000 ) ) ;
#277 = CARTESIAN_POINT ( 'NONE',  ( 5.885541736258995904, -3.216848386728015097, -7.752826540560539215 ) ) ;
#278 = CARTESIAN_POINT ( 'NONE',  ( 69.22368686548678340, -4.843077221807417843, 5.695980980372492120 ) ) ;
#279 = FACE_OUTER_BOUND ( 'NONE', #24858, .T. ) ;
#280 = VERTEX_POINT ( 'NONE', #698 ) ;
#281 = CARTESIAN_POINT ( 'NONE',  ( -7.237550801365592257, 3.675193018007247403, -1.088641768524161391 ) ) ;
#282 = ADVANCED_FACE ( 'NONE', ( #5372, #20917 ), #12718, .T. ) ;
#283 = CARTESIAN_POINT ( 'NONE',  ( 0.3045634402742546376, 4.096074720329792918, 9.425384029459841884 ) ) ;
#284 = CARTESIAN_POINT ( 'NONE',  ( 108.7297614063222113, 16.58428484178596207, 3.222654696952877096 ) ) ;
#285 = VERTEX_POINT ( 'NONE', #15558 ) ;
#286 = CARTESIAN_POINT ( 'NONE',  ( -5.750050799999999462, 7.347880794884122694E-16, 6.000000000000002665 ) ) ;
#287 = AXIS2_PLACEMENT_3D ( 'NONE', #26971, #13593, #8899 ) ;
#288 = ORIENTED_EDGE ( 'NONE', *, *, #372, .T. ) ;
#289 = CARTESIAN_POINT ( 'NONE',  ( 19.10390797508229710, -2.015740111943975066, -0.07017451552781585333 ) ) ;
#290 = DATE_AND_TIME ( #23181, #10926 ) ;
#292 = VERTEX_POINT ( 'NONE', #23411 ) ;
#291 = CARTESIAN_POINT ( 'NONE',  ( 0.3285611067768016147, -13.34342412963018276, -4.522129901861166701 ) ) ;
#293 = VERTEX_POINT ( 'NONE', #28613 ) ;
#294 = CARTESIAN_POINT ( 'NONE',  ( -3.765880891406458986, -9.390842214537469701, 1.743616753168593769 ) ) ;
#295 = ADVANCED_FACE ( 'NONE', ( #25777 ), #18309, .T. ) ;
#296 = ORIENTED_EDGE ( 'NONE', *, *, #10528, .F. ) ;
#297 = CARTESIAN_POINT ( 'NONE',  ( 7.249760686538667009, 0.000000000000000000, 0.000000000000000000 ) ) ;
#299 = VERTEX_POINT ( 'NONE', #30459 ) ;
#298 = CARTESIAN_POINT ( 'NONE',  ( 1.394036994807660394E-16, 1.625881193364758337, -4.467071865485455540 ) ) ;
#300 = CARTESIAN_POINT ( 'NONE',  ( 48.09670199522224721, -9.430894477034977186, 0.07017451552781803215 ) ) ;
#301 = DIRECTION ( 'NONE',  ( 0.4999999999999981681, 0.8660254037844397068, 0.000000000000000000 ) ) ;
#302 = EDGE_CURVE ( 'NONE', #6546, #31289, #13105, .T. ) ;
#303 = DIRECTION ( 'NONE',  ( -0.000000000000000000, -0.000000000000000000, -1.000000000000000000 ) ) ;
#304 = DIRECTION ( 'NONE',  ( 0.000000000000000000, 0.4226182617407134856, -0.9063077870366433864 ) ) ;
#305 = ORIENTED_EDGE ( 'NONE', *, *, #17119, .F. ) ;
#306 = CARTESIAN_POINT ( 'NONE',  ( 5.377543748152548986, -6.139290821770289064, 5.151476664237455871 ) ) ;
#307 = CARTESIAN_POINT ( 'NONE',  ( 25.86240141410256044, 23.76612641949138549, -0.4463807625373443777 ) ) ;
#308 = CARTESIAN_POINT ( 'NONE',  ( 7.249760686538667009, -8.466096581343467875, -2.210816291636301223 ) ) ;
#309 = DIRECTION ( 'NONE',  ( -1.000000000000000000, -0.000000000000000000, -0.000000000000000000 ) ) ;
#310 = CARTESIAN_POINT ( 'NONE',  ( 23.22564588060107482, -21.93932300456764040, 1.000000000000000000 ) ) ;
#311 = CARTESIAN_POINT ( 'NONE',  ( 2.330754651808292648E-16, 2.718385644597173467, 4.208382051008202396 ) ) ;
#312 = CARTESIAN_POINT ( 'NONE',  ( 2.376564509656898139, 9.436969261173645762, 5.239665997526921082 ) ) ;
#313 = CARTESIAN_POINT ( 'NONE',  ( 6.037141879243260512, -6.770886333893388453, -5.096219216992919243 ) ) ;
#314 = ORIENTED_EDGE ( 'NONE', *, *, #986, .T. ) ;
#315 = CARTESIAN_POINT ( 'NONE',  ( -6.812550801365595099, -1.828967928396026510, 3.368539882008728004 ) ) ;
#316 = EDGE_LOOP ( 'NONE', ( #2684, #263, #10060, #23233 ) ) ;
#317 = CARTESIAN_POINT ( 'NONE',  ( -3.504531657079157370, 2.975847129947406522, 0.3127741368606808403 ) ) ;
#318 = CARTESIAN_POINT ( 'NONE',  ( 108.0671932761865861, 18.55231859988835552, 4.648224005204301790 ) ) ;
#319 = CARTESIAN_POINT ( 'NONE',  ( 0.1303119166710321464, -6.187468044926815125, 1.772538222416039089 ) ) ;
#320 = CARTESIAN_POINT ( 'NONE',  ( 8.690654616498143525, -10.89241706857682956, 1.499999999999998668 ) ) ;
#321 = ORIENTED_EDGE ( 'NONE', *, *, #29783, .T. ) ;
#322 = CARTESIAN_POINT ( 'NONE',  ( 102.2656009641821271, -1.731193774301692523, -2.184956770134436344 ) ) ;
#323 = ORIENTED_EDGE ( 'NONE', *, *, #3103, .F. ) ;
#324 = FACE_OUTER_BOUND ( 'NONE', #26610, .T. ) ;
#325 = CALENDAR_DATE ( 2026, 6, 10 ) ;
#326 = CARTESIAN_POINT ( 'NONE',  ( 28.66745692012980840, -6.633544308268587208, 4.150065909475219250 ) ) ;
#327 = EDGE_CURVE ( 'NONE', #7729, #6546, #8223, .T. ) ;
#328 = EDGE_CURVE ( 'NONE', #24580, #21614, #8416, .T. ) ;
#329 = CARTESIAN_POINT ( 'NONE',  ( 2.619932554246601438E-16, 3.055657119358849982, -3.641590349731898879 ) ) ;
#331 = SPHERICAL_SURFACE ( 'NONE', #5973, 0.5000000000000000000 ) ;
#330 = CARTESIAN_POINT ( 'NONE',  ( 7.249760686538667009, 0.000000000000000000, 0.000000000000000000 ) ) ;
#332 = ORIENTED_EDGE ( 'NONE', *, *, #10400, .T. ) ;
#333 = CARTESIAN_POINT ( 'NONE',  ( -8.000050800000002127, -3.003076289684047495, 0.02717128497728628356 ) ) ;
#334 = CARTESIAN_POINT ( 'NONE',  ( 7.249760686538667009, 8.721381771256204729, -0.7071067811865423547 ) ) ;
#335 = DIRECTION ( 'NONE',  ( -0.000000000000000000, -0.000000000000000000, -1.000000000000000000 ) ) ;
#336 = DIRECTION ( 'NONE',  ( 8.574039729943018344E-17, 1.000000000000000000, 0.000000000000000000 ) ) ;
#338 = ORIENTED_EDGE ( 'NONE', *, *, #20871, .F. ) ;
#337 = CARTESIAN_POINT ( 'NONE',  ( 108.3527736681033531, 20.14254290672267800, -1.579327705512915569 ) ) ;
#339 = CARTESIAN_POINT ( 'NONE',  ( -7.712550801365593678, 1.088641768524161613, 3.675193018007247403 ) ) ;
#340 = CARTESIAN_POINT ( 'NONE',  ( 0.000000000000000000, 0.000000000000000000, 0.000000000000000000 ) ) ;
#341 = CARTESIAN_POINT ( 'NONE',  ( -31.68982948510041808, 0.2071067811865522357, 1.500000000000005329 ) ) ;
#342 = ORIENTED_EDGE ( 'NONE', *, *, #15050, .F. ) ;
#343 = ORIENTED_EDGE ( 'NONE', *, *, #19267, .T. ) ;
#344 = CARTESIAN_POINT ( 'NONE',  ( 25.75999999999999801, 2.805042440084548172, 1.132414195126726364 ) ) ;
#345 = CARTESIAN_POINT ( 'NONE',  ( 4.749760686538667009, -7.530955069117533540, 2.741043480754901118 ) ) ;
#346 = EDGE_CURVE ( 'NONE', #14768, #27103, #14556, .T. ) ;
#347 = CARTESIAN_POINT ( 'NONE',  ( 22.48500000136559507, 0.9349337715887185984, -3.156283516753368268 ) ) ;
#348 = CARTESIAN_POINT ( 'NONE',  ( 0.000000000000000000, 1.999317321091499400, 10.76487093102065451 ) ) ;
#349 = CARTESIAN_POINT ( 'NONE',  ( 29.27523314209411609, -3.695744416148339706, -0.07017451552781629742 ) ) ;
#350 = CARTESIAN_POINT ( 'NONE',  ( 3.122314033877900197E-16, 3.641590349731971710, -3.055657119358763829 ) ) ;
#351 = ORIENTED_EDGE ( 'NONE', *, *, #13040, .F. ) ;
#352 = CARTESIAN_POINT ( 'NONE',  ( 2.795120667414443094, 7.433119754671809964, -6.320583870825271511 ) ) ;
#353 = EDGE_CURVE ( 'NONE', #9758, #29455, #29513, .T. ) ;
#354 = PERSON_AND_ORGANIZATION ( #6766, #25292 ) ;
#355 = CARTESIAN_POINT ( 'NONE',  ( 0.000000000000000000, 0.000000000000000000, 0.000000000000000000 ) ) ;
#356 = ORIENTED_EDGE ( 'NONE', *, *, #4582, .F. ) ;
#357 = DIRECTION ( 'NONE',  ( 0.000000000000000000, 0.000000000000000000, 1.000000000000000000 ) ) ;
#358 = EDGE_LOOP ( 'NONE', ( #22416, #3974, #15722, #2891 ) ) ;
#359 = CARTESIAN_POINT ( 'NONE',  ( -18.90990005423338971, 16.40670164838886791, 1.822708526801201767 ) ) ;
#361 = ORIENTED_EDGE ( 'NONE', *, *, #14296, .F. ) ;
#360 = CARTESIAN_POINT ( 'NONE',  ( 28.68200330690814681, -6.065191176915236682, -4.312042181581901445 ) ) ;
#362 = ADVANCED_FACE ( 'NONE', ( #28114 ), #31976, .F. ) ;
#363 = ORIENTED_EDGE ( 'NONE', *, *, #25190, .F. ) ;
#364 = CYLINDRICAL_SURFACE ( 'NONE', #25143, 3.000000000000000444 ) ;
#365 = CARTESIAN_POINT ( 'NONE',  ( -6.512550801365594388, -1.088641768524163611, -3.675193018007245627 ) ) ;
#366 = CARTESIAN_POINT ( 'NONE',  ( 26.11000000000000298, 1.942864903642424146, 1.573300977624592534 ) ) ;
#367 = CARTESIAN_POINT ( 'NONE',  ( 1.624999999999999778, 1.464956435139542767, 10.90201369670499254 ) ) ;
#369 = ORIENTED_EDGE ( 'NONE', *, *, #18274, .T. ) ;
#368 = DIRECTION ( 'NONE',  ( -0.9816271834476639757, 0.000000000000000000, -0.1908089953765449709 ) ) ;
#370 = DIRECTION ( 'NONE',  ( 1.000000000000000000, -2.473959037481237219E-13, 0.000000000000000000 ) ) ;
#371 = CARTESIAN_POINT ( 'NONE',  ( 23.81497248397844402, 17.93793532042042571, 1.500000000000414557 ) ) ;
#372 = EDGE_CURVE ( 'NONE', #17843, #32661, #6158, .T. ) ;
#373 = CARTESIAN_POINT ( 'NONE',  ( -4.433196769082780264, -8.338993190668213984, 1.500000000000000000 ) ) ;
#374 = CARTESIAN_POINT ( 'NONE',  ( 25.67250000136559507, 2.363507492473148286, 1.913930629741525058 ) ) ;
#375 = CARTESIAN_POINT ( 'NONE',  ( 72.90878003214187686, -18.24052684336794883, 1.499999999999999556 ) ) ;
#377 = ORIENTED_EDGE ( 'NONE', *, *, #23581, .T. ) ;
#376 = CARTESIAN_POINT ( 'NONE',  ( 18.60402535541760827, -7.603424548860325594, -0.4426577273443823568 ) ) ;
#378 = CARTESIAN_POINT ( 'NONE',  ( 107.6235316907398811, 18.91057310341854603, 4.414476567109417715 ) ) ;
#379 = CARTESIAN_POINT ( 'NONE',  ( 3.499999999999999556, 5.471841788314750765, -3.018103451449674068 ) ) ;
#380 = CARTESIAN_POINT ( 'NONE',  ( 22.04750000136559507, -3.024605502323851169, 0.3178988483021052969 ) ) ;
#381 = EDGE_CURVE ( 'NONE', #25477, #26129, #24703, .T. ) ;
#382 = CARTESIAN_POINT ( 'NONE',  ( -8.000050800000000351, 0.2618957199879418662, -2.989246278116708400 ) ) ;
#383 = DIRECTION ( 'NONE',  ( -0.000000000000000000, -0.000000000000000000, -1.000000000000000000 ) ) ;
#384 = DIRECTION ( 'NONE',  ( -1.000000000000000000, -0.000000000000000000, -0.000000000000000000 ) ) ;
#385 = EDGE_LOOP ( 'NONE', ( #24811, #18638, #9529, #556 ) ) ;
#386 = CARTESIAN_POINT ( 'NONE',  ( 1.624999999999999778, 4.762163868918273479, 9.915734732513236338 ) ) ;
#387 = EDGE_CURVE ( 'NONE', #22172, #21390, #18321, .T. ) ;
#388 = DIRECTION ( 'NONE',  ( 0.000000000000000000, -1.000000000000000000, 0.000000000000000000 ) ) ;
#389 = VERTEX_POINT ( 'NONE', #29371 ) ;
#390 = DIRECTION ( 'NONE',  ( 0.5000000000000002220, 0.09052430460833657544, 0.8612812260087741034 ) ) ;
#391 = CARTESIAN_POINT ( 'NONE',  ( 0.7632845268398871230, 0.000000000000000000, 0.000000000000000000 ) ) ;
#392 = EDGE_CURVE ( 'NONE', #27444, #8159, #6302, .T. ) ;
#393 = CARTESIAN_POINT ( 'NONE',  ( -1.047937531484008478, -4.989690239015235562, -4.522129901861164925 ) ) ;
#395 = CARTESIAN_POINT ( 'NONE',  ( 107.5537258199849617, -18.86684600943444678, 4.756303069492835434 ) ) ;
#394 = CARTESIAN_POINT ( 'NONE',  ( 18.65837979360809840, -6.995851018290569989, 0.07017451552783667001 ) ) ;
#396 = ADVANCED_FACE ( 'NONE', ( #26695 ), #12150, .T. ) ;
#397 = ORIENTED_EDGE ( 'NONE', *, *, #19596, .F. ) ;
#398 = CARTESIAN_POINT ( 'NONE',  ( -40.27879340802675756, -12.50360960397076582, 5.500000000000000000 ) ) ;
#399 = EDGE_LOOP ( 'NONE', ( #18098, #32679, #22647, #21722 ) ) ;
#400 = CARTESIAN_POINT ( 'NONE',  ( 2.437082316315989150, 1.217322776604855550, -10.59788678609682755 ) ) ;
#402 = ORIENTED_EDGE ( 'NONE', *, *, #26636, .T. ) ;
#401 = CARTESIAN_POINT ( 'NONE',  ( 109.3993806922052840, 20.31298924473512457, -2.334455007174283558 ) ) ;
#403 = ORIENTED_EDGE ( 'NONE', *, *, #25920, .T. ) ;
#404 = CARTESIAN_POINT ( 'NONE',  ( 110.6444052656891301, 21.58830278953161752, -0.4463807625373402699 ) ) ;
#405 = DIRECTION ( 'NONE',  ( -1.000000000000000000, 0.000000000000000000, -0.000000000000000000 ) ) ;
#407 = ORIENTED_EDGE ( 'NONE', *, *, #15411, .F. ) ;
#406 = CARTESIAN_POINT ( 'NONE',  ( 108.6155529559672885, -15.79924867777639186, -1.500000000000000000 ) ) ;
#408 = ORIENTED_EDGE ( 'NONE', *, *, #11645, .F. ) ;
#409 = CARTESIAN_POINT ( 'NONE',  ( 7.249760686538667009, -6.940565734314570356, -4.007137495034885255 ) ) ;
#410 = CARTESIAN_POINT ( 'NONE',  ( -23.54713438637982748, 14.02568012664692532, 10.48023388603047579 ) ) ;
#411 = CARTESIAN_POINT ( 'NONE',  ( 107.6641948605228123, -20.45809826282219746, -1.499999999999999556 ) ) ;
#412 = CARTESIAN_POINT ( 'NONE',  ( 34.48223484310469189, 0.5174497483512505713, 2.981930256614498287 ) ) ;
#413 = CARTESIAN_POINT ( 'NONE',  ( 101.6441386174529953, -1.774168274679931212, 2.184956718805492581 ) ) ;
#414 = ADVANCED_FACE ( 'NONE', ( #24506 ), #19854, .T. ) ;
#415 = CARTESIAN_POINT ( 'NONE',  ( 3.249999999999999556, -4.472189673936727949, -8.264486777890155622 ) ) ;
#416 = CARTESIAN_POINT ( 'NONE',  ( 19.80237848050798988, -16.61788897934828668, 1.500000000000000666 ) ) ;
#417 = DIRECTION ( 'NONE',  ( -1.000000000000000000, 8.574039729943018344E-17, -0.000000000000000000 ) ) ;
#418 = LINE ( 'NONE', #30860, #2758 ) ;
#419 = CARTESIAN_POINT ( 'NONE',  ( 6.037141879243264064, 5.096219216992939671, -6.770886333893373354 ) ) ;
#420 =( BOUNDED_CURVE ( )  B_SPLINE_CURVE ( 3, ( #13886, #28791, #15780, #3092 ),
 .UNSPECIFIED., .F., .F. ) 
 B_SPLINE_CURVE_WITH_KNOTS ( ( 4, 4 ),
 ( 4.530379766455337354, 4.712388980384688786 ),
 .UNSPECIFIED. ) 
 CURVE ( )  GEOMETRIC_REPRESENTATION_ITEM ( )  RATIONAL_B_SPLINE_CURVE ( ( 1.000000000000000000, 0.9972412918903135193, 0.9972412918903135193, 1.000000000000000000 ) ) 
 REPRESENTATION_ITEM ( '' )  );
#421 = CARTESIAN_POINT ( 'NONE',  ( 5.377543748152549874, -5.151476664237518044, 6.139290821770238438 ) ) ;
#422 = CARTESIAN_POINT ( 'NONE',  ( 7.249760686538667009, -8.711672189281420842, -0.8180878109962766986 ) ) ;
#423 = EDGE_CURVE ( 'NONE', #9882, #10953, #9131, .T. ) ;
#424 = LINE ( 'NONE', #31348, #31150 ) ;
#425 = VERTEX_POINT ( 'NONE', #11999 ) ;
#426 = CARTESIAN_POINT ( 'NONE',  ( 25.36241694306878358, -2.409633728563083999, 1.062054624121506530 ) ) ;
#427 = EDGE_CURVE ( 'NONE', #20419, #3413, #32361, .T. ) ;
#428 = DIRECTION ( 'NONE',  ( 0.000000000000000000, 1.000000000000000000, 0.000000000000000000 ) ) ;
#429 = VERTEX_POINT ( 'NONE', #6803 ) ;
#430 = DIRECTION ( 'NONE',  ( -1.000000000000000000, 0.000000000000000000, 0.000000000000000000 ) ) ;
#431 = EDGE_CURVE ( 'NONE', #18549, #32842, #2321, .T. ) ;
#432 = ORIENTED_EDGE ( 'NONE', *, *, #6249, .F. ) ;
#433 = CARTESIAN_POINT ( 'NONE',  ( 47.98568197278773795, -2.821418575600917578, -1.010822989962086416 ) ) ;
#434 = ITEM_DEFINED_TRANSFORMATION ( 'NONE', 'NONE', #5522,  #2865 ) ;
#436 = VERTEX_POINT ( 'NONE', #29725 ) ;
#435 = CARTESIAN_POINT ( 'NONE',  ( -0.9232102171129831225, 0.000000000000000000, -4.522129901861166701 ) ) ;
#437 = ORIENTED_EDGE ( 'NONE', *, *, #9373, .F. ) ;
#438 = CARTESIAN_POINT ( 'NONE',  ( 16.00007615138554584, -20.81650653636907222, 1.751028325053374912 ) ) ;
#439 = ORIENTED_EDGE ( 'NONE', *, *, #22087, .T. ) ;
#440 = CARTESIAN_POINT ( 'NONE',  ( 5.612973690782940395, 0.1996300861632082368, -8.213905076232775215 ) ) ;
#442 = VERTEX_POINT ( 'NONE', #22198 ) ;
#441 = CARTESIAN_POINT ( 'NONE',  ( -2.410187303267195436, 0.5774022981078724692, 3.166406138753334876 ) ) ;
#443 = CARTESIAN_POINT ( 'NONE',  ( 85.48138648428258080, -7.654866896025229295, 1.915219082070893863 ) ) ;
#444 = CARTESIAN_POINT ( 'NONE',  ( 10.52034268205830259, 3.641590349731929077, 3.055657119358814011 ) ) ;
#445 = CARTESIAN_POINT ( 'NONE',  ( 34.48223484310472031, 0.5000000000000000000, -2.552009564962230304 ) ) ;
#446 = DIRECTION ( 'NONE',  ( 0.000000000000000000, -1.000000000000000000, 0.000000000000000000 ) ) ;
#447 = EDGE_CURVE ( 'NONE', #26968, #22574, #32221, .T. ) ;
#448 = VERTEX_POINT ( 'NONE', #22027 ) ;
#449 = CC_DESIGN_PERSON_AND_ORGANIZATION_ASSIGNMENT ( #5660, #26050, ( #25774 ) ) ;
#450 = DIRECTION ( 'NONE',  ( 0.000000000000000000, -0.000000000000000000, 1.000000000000000000 ) ) ;
#451 = CARTESIAN_POINT ( 'NONE',  ( -1.170068671574863162, -6.059534462705075342, -4.522129901861164925 ) ) ;
#452 = CARTESIAN_POINT ( 'NONE',  ( 41.35542541871918587, -7.892720653449311285, -2.184957211333078408 ) ) ;
#453 = CARTESIAN_POINT ( 'NONE',  ( 3.499999999999999556, 0.000000000000000000, 0.000000000000000000 ) ) ;
#454 = CARTESIAN_POINT ( 'NONE',  ( -8.000050800000003903, -2.272722698207227054, 1.977113453969371992 ) ) ;
#455 = CARTESIAN_POINT ( 'NONE',  ( -7.100050802731186828, -2.853674364686378695, -1.549418761218566809 ) ) ;
#456 = LINE ( 'NONE', #31055, #2820 ) ;
#458 = CARTESIAN_POINT ( 'NONE',  ( -31.18783180709124636, -25.44850941282521006, 1.500000000000000000 ) ) ;
#457 = DESIGN_CONTEXT ( 'detailed design', #29768, 'design' ) ;
#459 = CARTESIAN_POINT ( 'NONE',  ( -4.612550801365593145, 3.368539882008727115, 1.828967928396026954 ) ) ;
#460 = ORIENTED_EDGE ( 'NONE', *, *, #1746, .F. ) ;
#461 = EDGE_CURVE ( 'NONE', #19227, #4581, #203, .T. ) ;
#462 = CARTESIAN_POINT ( 'NONE',  ( -4.254531657079158258, 2.846291840500173365, 1.545410377633946952 ) ) ;
#463 = CIRCLE ( 'NONE', #26112, 2.524999999999999467 ) ;
#464 = CARTESIAN_POINT ( 'NONE',  ( 107.9275968081481238, 17.77499038371485440, 4.627610784060872895 ) ) ;
#465 = DIRECTION ( 'NONE',  ( 1.000000000000000000, 0.000000000000000000, 0.000000000000000000 ) ) ;
#466 = CARTESIAN_POINT ( 'NONE',  ( 10.37705096095590385, -12.86926679082321989, 1.500000000000000000 ) ) ;
#467 = ORIENTED_EDGE ( 'NONE', *, *, #26078, .F. ) ;
#468 = CARTESIAN_POINT ( 'NONE',  ( 54.93487251133846883, -4.984033517864898677, -3.390608480941980307 ) ) ;
#469 = VERTEX_POINT ( 'NONE', #6960 ) ;
#470 = CARTESIAN_POINT ( 'NONE',  ( 8.911384905465473238, 0.4717275430040298034, -1.041239158277187160 ) ) ;
#471 = CALENDAR_DATE ( 2026, 6, 10 ) ;
#472 = CARTESIAN_POINT ( 'NONE',  ( 18.77392604112944596, -5.704275868917796366, 4.185347664740951323 ) ) ;
#473 = CARTESIAN_POINT ( 'NONE',  ( -56.32770133515839461, 0.5000000000000000000, -1.500000000000000000 ) ) ;
#475 = CARTESIAN_POINT ( 'NONE',  ( 3.249999999999999556, -9.314797388894881180, -1.239665997526989027 ) ) ;
#474 = CARTESIAN_POINT ( 'NONE',  ( -31.57659242536668032, -27.93932300454937590, -1.500000000000000000 ) ) ;
#476 = ORIENTED_EDGE ( 'NONE', *, *, #29164, .F. ) ;
#477 = CARTESIAN_POINT ( 'NONE',  ( -16.20597128428593336, -10.96966150227469328, -11.00000000000000000 ) ) ;
#478 = DIRECTION ( 'NONE',  ( -0.9916316928897271898, 0.1290991311227692728, 0.000000000000000000 ) ) ;
#479 = FACE_OUTER_BOUND ( 'NONE', #18450, .T. ) ;
#481 = VERTEX_POINT ( 'NONE', #4141 ) ;
#480 = CARTESIAN_POINT ( 'NONE',  ( 3.249999999999999556, -4.472189673936843413, 8.264486777890091673 ) ) ;
#482 = CARTESIAN_POINT ( 'NONE',  ( -5.662550801365592967, 0.3701630799359330593, -3.521866450007987037 ) ) ;
#483 = FACE_OUTER_BOUND ( 'NONE', #1513, .T. ) ;
#484 = CARTESIAN_POINT ( 'NONE',  ( 18.72482702355275919, -6.253104344970715545, -3.390608483633605896 ) ) ;
#485 = ORIENTED_EDGE ( 'NONE', *, *, #21661, .T. ) ;
#486 = EDGE_LOOP ( 'NONE', ( #3638, #26614, #7912, #9286 ) ) ;
#487 = DIRECTION ( 'NONE',  ( 0.000000000000000000, 0.000000000000000000, 1.000000000000000000 ) ) ;
#488 = CARTESIAN_POINT ( 'NONE',  ( 10.00000000000000178, -8.574039729943018837E-16, 0.000000000000000000 ) ) ;
#489 = EDGE_CURVE ( 'NONE', #14880, #20515, #18846, .T. ) ;
#490 = DIRECTION ( 'NONE',  ( 0.000000000000000000, 0.000000000000000000, -1.000000000000000000 ) ) ;
#491 = EDGE_CURVE ( 'NONE', #21250, #937, #1474, .T. ) ;
#492 = CARTESIAN_POINT ( 'NONE',  ( 2.437082469501525850, 2.117184480729110252, 10.45536235038312789 ) ) ;
#493 = CARTESIAN_POINT ( 'NONE',  ( 2.693711038332267105, -9.791507810136474532, 2.271851790478933264 ) ) ;
#494 = ADVANCED_FACE ( 'NONE', ( #32059 ), #21714, .T. ) ;
#495 = DIRECTION ( 'NONE',  ( -1.000000000000000000, -0.000000000000000000, 0.000000000000000000 ) ) ;
#496 = CARTESIAN_POINT ( 'NONE',  ( 35.27105150273526135, -8.350847396885011875, 0.8105616794655192692 ) ) ;
#497 = ORIENTED_EDGE ( 'NONE', *, *, #9027, .F. ) ;
#498 = DIRECTION ( 'NONE',  ( -1.000000000000000000, -0.000000000000000000, 3.469446951953613794E-15 ) ) ;
#499 = ORIENTED_EDGE ( 'NONE', *, *, #31059, .T. ) ;
#500 = PERSON_AND_ORGANIZATION ( #6766, #25292 ) ;
#501 = DIRECTION ( 'NONE',  ( 0.000000000000000000, 0.9659258262890683122, -0.2588190451025207950 ) ) ;
#502 = VERTEX_POINT ( 'NONE', #30290 ) ;
#503 = CARTESIAN_POINT ( 'NONE',  ( 12.58808848377064749, -13.45617626434417424, -1.000000000000000000 ) ) ;
#504 = AXIS2_PLACEMENT_3D ( 'NONE', #2462, #12630, #10109 ) ;
#505 = ORIENTED_EDGE ( 'NONE', *, *, #30275, .T. ) ;
#506 = CARTESIAN_POINT ( 'NONE',  ( -5.050050802731187005, 1.887961173149511618, 2.331437884370912705 ) ) ;
#508 = VERTEX_POINT ( 'NONE', #20245 ) ;
#507 = CARTESIAN_POINT ( 'NONE',  ( 69.02940965804741325, -5.294544073343872448, -4.275175994953113623 ) ) ;
#509 = EDGE_LOOP ( 'NONE', ( #5695, #23872, #18382, #2587 ) ) ;
#510 = DIRECTION ( 'NONE',  ( -7.023442172597817418E-17, -0.8191520442889873577, -0.5735764363510524877 ) ) ;
#511 = CARTESIAN_POINT ( 'NONE',  ( -7.462550801365593678, -3.521866450007987037, -0.3701630799359323931 ) ) ;
#512 = CARTESIAN_POINT ( 'NONE',  ( 25.60999999999999943, -1.942864903642428587, -1.573300977624592756 ) ) ;
#513 = CARTESIAN_POINT ( 'NONE',  ( 48.09670199522225431, -9.430894477034977186, -1.010822989962099960 ) ) ;
#514 = AXIS2_PLACEMENT_3D ( 'NONE', #118, #18332, #28539 ) ;
#516 = VERTEX_POINT ( 'NONE', #28101 ) ;
#515 = DIRECTION ( 'NONE',  ( 0.000000000000000000, 1.000000000000000000, -3.469446951953611033E-15 ) ) ;
#517 = DIRECTION ( 'NONE',  ( 0.000000000000000000, 0.000000000000000000, 1.000000000000000000 ) ) ;
#518 = CARTESIAN_POINT ( 'NONE',  ( 28.57616583553759426, -7.888378049842258655, 2.184956778784801212 ) ) ;
#519 = CARTESIAN_POINT ( 'NONE',  ( -4.280319716189089796, -6.512003988132526899, 1.499999999999839906 ) ) ;
#521 = CARTESIAN_POINT ( 'NONE',  ( 0.3749740905865333596, -7.612528756000540575, 6.632019415960392905 ) ) ;
#520 = APPLICATION_CONTEXT ( 'configuration controlled 3d designs of mechanical parts and assemblies' ) ;
#522 = CARTESIAN_POINT ( 'NONE',  ( 9.282537329959881234, 0.2172754300398732352, 1.050000000000000044 ) ) ;
#524 = ORIENTED_EDGE ( 'NONE', *, *, #21647, .T. ) ;
#523 = CARTESIAN_POINT ( 'NONE',  ( 12.40148790557316794, 21.49000000000003041, 1.500000000000000000 ) ) ;
#525 = PLANE ( 'NONE',  #17308 ) ;
#526 = EDGE_CURVE ( 'NONE', #4621, #9325, #17910, .T. ) ;
#527 = CARTESIAN_POINT ( 'NONE',  ( -30.13173294563779692, 12.12011656760094347, 1.929752697766440095 ) ) ;
#528 = CARTESIAN_POINT ( 'NONE',  ( 25.23500000273118715, 2.486304738420679783, -0.2613211581691337604 ) ) ;
#529 = CARTESIAN_POINT ( 'NONE',  ( 3.249999999999999556, 5.538577986808997267, -6.772677083992326708 ) ) ;
#530 = CIRCLE ( 'NONE', #8506, 10.46966150227469150 ) ;
#531 = PLANE ( 'NONE',  #9140 ) ;
#532 = CARTESIAN_POINT ( 'NONE',  ( -2.800010172794354268, -0.4410551771863219783, -1.509141217649267563 ) ) ;
#533 = VERTEX_POINT ( 'NONE', #7525 ) ;
#534 = LINE ( 'NONE', #15760, #25821 ) ;
#535 = AXIS2_PLACEMENT_3D ( 'NONE', #29828, #6903, #19297 ) ;
#536 = VERTEX_POINT ( 'NONE', #30638 ) ;
#537 = AXIS2_PLACEMENT_3D ( 'NONE', #26514, #11961, #29839 ) ;
#538 = LINE ( 'NONE', #32993, #30655 ) ;
#539 = CARTESIAN_POINT ( 'NONE',  ( 8.883366670699761071E-16, -1.425064293572414265, 10.85582367538893855 ) ) ;
#540 = CARTESIAN_POINT ( 'NONE',  ( 0.5859972064454607166, -5.135271408404159743, -0.9788672205888330202 ) ) ;
#542 = CARTESIAN_POINT ( 'NONE',  ( 107.9485675974711825, -17.32874831497913704, 4.529272001225892907 ) ) ;
#541 = CARTESIAN_POINT ( 'NONE',  ( 9.225170531479669478, -11.43511417576379152, 1.000000000000000222 ) ) ;
#543 = ORIENTED_EDGE ( 'NONE', *, *, #5001, .T. ) ;
#544 = FACE_OUTER_BOUND ( 'NONE', #17814, .T. ) ;
#545 = VERTEX_POINT ( 'NONE', #10382 ) ;
#546 = LINE ( 'NONE', #10576, #3351 ) ;
#548 = ORIENTED_EDGE ( 'NONE', *, *, #612, .F. ) ;
#547 = CARTESIAN_POINT ( 'NONE',  ( 0.000000000000000000, 0.5000000000000000000, 1.500000000000000000 ) ) ;
#549 = ORIENTED_EDGE ( 'NONE', *, *, #24860, .T. ) ;
#550 = CYLINDRICAL_SURFACE ( 'NONE', #17716, 5.010000000000000675 ) ;
#551 = EDGE_CURVE ( 'NONE', #8703, #19157, #23122, .T. ) ;
#552 = AXIS2_PLACEMENT_3D ( 'NONE', #1507, #1358, #29414 ) ;
#553 = DIRECTION ( 'NONE',  ( -0.1908089953765452762, 2.336736254364082527E-17, 0.9816271834476639757 ) ) ;
#555 = ORIENTED_EDGE ( 'NONE', *, *, #27981, .T. ) ;
#554 = CARTESIAN_POINT ( 'NONE',  ( 18.90256931246762662, -4.266302279389236674, 3.236220886658451867 ) ) ;
#556 = ORIENTED_EDGE ( 'NONE', *, *, #21436, .T. ) ;
#557 = CARTESIAN_POINT ( 'NONE',  ( -17.45597128428593692, -25.43932300454937945, 11.00000000000000000 ) ) ;
#558 = ADVANCED_FACE ( 'NONE', ( #15374 ), #27940, .T. ) ;
#559 = DIRECTION ( 'NONE',  ( 0.000000000000000000, 0.000000000000000000, 1.000000000000000000 ) ) ;
#560 = CARTESIAN_POINT ( 'NONE',  ( 25.61042644976673444, -17.59778802277001475, -1.000000000000000000 ) ) ;
#561 = DIRECTION ( 'NONE',  ( -2.219124775574906615E-17, -0.2588190451025184080, -0.9659258262890689783 ) ) ;
#562 = CARTESIAN_POINT ( 'NONE',  ( 0.5664946525141408840, -9.241976615262153416, 2.300561732649529567 ) ) ;
#563 = VECTOR ( 'NONE', #4638, 1000.000000000000000 ) ;
#564 = CARTESIAN_POINT ( 'NONE',  ( -6.512942406915326110, 3.284080845023683730E-15, 3.000000000000000000 ) ) ;
#565 = DIRECTION ( 'NONE',  ( -1.000000000000000000, -0.000000000000000000, 0.000000000000000000 ) ) ;
#566 = CARTESIAN_POINT ( 'NONE',  ( 102.4497391607695107, -4.374320780259970398, 3.390608474976775533 ) ) ;
#567 = ADVANCED_FACE ( 'NONE', ( #23085 ), #2862, .T. ) ;
#568 = EDGE_CURVE ( 'NONE', #31503, #15557, #22908, .T. ) ;
#569 = B_SPLINE_CURVE_WITH_KNOTS ( 'NONE', 3,
 ( #22916, #20430, #30648, #17918, #6761, #28109, #15384, #16952, #27148, #25941 ),
 .UNSPECIFIED., .F., .F.,
 ( 4, 2, 2, 2, 4 ),
 ( 1.968338519001761812E-07, 0.0005467927057105467954, 0.001093388577569193469, 0.001639984449427840142, 0.002186580321286488333 ),
 .UNSPECIFIED. ) ;
#570 = CARTESIAN_POINT ( 'NONE',  ( 74.44693909926891706, -23.04272217940160417, 0.9788672205877712029 ) ) ;
#571 = CARTESIAN_POINT ( 'NONE',  ( 6.880159329304571081, 5.066480354149027754, -7.110803091624010364 ) ) ;
#572 = VERTEX_POINT ( 'NONE', #7365 ) ;
#573 = CARTESIAN_POINT ( 'NONE',  ( 109.4759884372992076, 20.73957139739071209, 1.099690583642431996 ) ) ;
#574 = CIRCLE ( 'NONE', #2174, 11.00000000000000000 ) ;
#575 = AXIS2_PLACEMENT_3D ( 'NONE', #12635, #6949, #22840 ) ;
#576 = CARTESIAN_POINT ( 'NONE',  ( 85.13613392229180477, -2.069934983084472879, 2.713652344655542503 ) ) ;
#577 = ADVANCED_FACE ( 'NONE', ( #20591 ), #17409, .T. ) ;
#578 = CARTESIAN_POINT ( 'NONE',  ( 13.28835132608794467, 21.83091171094871541, -1.350227401154549201 ) ) ;
#579 = ORIENTED_EDGE ( 'NONE', *, *, #5693, .F. ) ;
#580 = CARTESIAN_POINT ( 'NONE',  ( 22.54750000136559507, 1.913930629741522838, -2.363507492473150062 ) ) ;
#581 = AXIS2_PLACEMENT_3D ( 'NONE', #10709, #10896, #26590 ) ;
#582 = CIRCLE ( 'NONE', #14406, 8.025310301077755781 ) ;
#583 = CARTESIAN_POINT ( 'NONE',  ( -2.300050802731187449, -2.853674364686378695, -1.549418761218566809 ) ) ;
#584 = CYLINDRICAL_SURFACE ( 'NONE', #24225, 0.5000000000000000000 ) ;
#585 = ORIENTED_EDGE ( 'NONE', *, *, #31853, .T. ) ;
#586 = CARTESIAN_POINT ( 'NONE',  ( 29.41391112839825794, -2.700987858898180161, -0.07017451552781628354 ) ) ;
#587 = EDGE_CURVE ( 'NONE', #19482, #31424, #9790, .T. ) ;
#588 = AXIS2_PLACEMENT_3D ( 'NONE', #14724, #17049, #17552 ) ;
#589 = ORIENTED_EDGE ( 'NONE', *, *, #4285, .T. ) ;
#590 = CARTESIAN_POINT ( 'NONE',  ( -2.476225935960405966, -0.3178988483021057410, 3.024605502323848949 ) ) ;
#591 = COORDINATED_UNIVERSAL_TIME_OFFSET ( 0, 0, .AHEAD. ) ;
#593 = VERTEX_POINT ( 'NONE', #13532 ) ;
#592 = CARTESIAN_POINT ( 'NONE',  ( 22.80656763371926843, 0.8852964313267434049, -2.499999999999998224 ) ) ;
#594 = ORIENTED_EDGE ( 'NONE', *, *, #1096, .T. ) ;
#595 = CARTESIAN_POINT ( 'NONE',  ( 24.98500000136559507, -2.892927487894331406, 1.570731468192932523 ) ) ;
#596 = VERTEX_POINT ( 'NONE', #15873 ) ;
#597 = CARTESIAN_POINT ( 'NONE',  ( -7.712942406915323623, 7.727249047114547632E-16, -2.999999999999999556 ) ) ;
#599 = ORIENTED_EDGE ( 'NONE', *, *, #16813, .F. ) ;
#598 = CARTESIAN_POINT ( 'NONE',  ( 34.48223484310472031, 0.000000000000000000, -2.552009564962230304 ) ) ;
#600 = CARTESIAN_POINT ( 'NONE',  ( 0.1606233661178082250, 7.161985370896794656, -7.854816391752104998 ) ) ;
#601 = DIRECTION ( 'NONE',  ( -0.000000000000000000, -0.3746065934159164001, 0.9271838545667856479 ) ) ;
#602 = CIRCLE ( 'NONE', #15549, 6.000000000000000888 ) ;
#603 = VECTOR ( 'NONE', #13281, 999.9999999999998863 ) ;
#604 = LINE ( 'NONE', #23341, #24218 ) ;
#605 = CARTESIAN_POINT ( 'NONE',  ( 7.249760686538667009, 5.064320921489914973, -7.135485519861949122 ) ) ;
#606 = CIRCLE ( 'NONE', #12872, 7.981930256614262476 ) ;
#607 = ORIENTED_EDGE ( 'NONE', *, *, #23916, .F. ) ;
#608 = VECTOR ( 'NONE', #21725, 1000.000000000000000 ) ;
#609 = DIRECTION ( 'NONE',  ( -0.000000000000000000, -0.000000000000000000, -1.000000000000000000 ) ) ;
#610 = CARTESIAN_POINT ( 'NONE',  ( 85.12704628545870378, -6.675959057340966396, -1.529339193924102558 ) ) ;
#611 = CARTESIAN_POINT ( 'NONE',  ( -6.607304909706597229, 1.062355717592093463, 3.000000000000000000 ) ) ;
#612 = EDGE_CURVE ( 'NONE', #16944, #1202, #29094, .T. ) ;
#613 = EDGE_CURVE ( 'NONE', #28731, #7095, #18897, .T. ) ;
#614 = AXIS2_PLACEMENT_3D ( 'NONE', #4782, #32547, #27177 ) ;
#615 = CARTESIAN_POINT ( 'NONE',  ( -8.000050799999998574, 0.5580980903926698877, 3.189890360694769278 ) ) ;
#616 = CARTESIAN_POINT ( 'NONE',  ( 0.7632845268398871230, 0.000000000000000000, 0.000000000000000000 ) ) ;
#617 = DIRECTION ( 'NONE',  ( 1.000000000000000000, 5.361488761196503499E-16, 0.000000000000000000 ) ) ;
#618 = EDGE_CURVE ( 'NONE', #28100, #32600, #18353, .T. ) ;
#619 = CARTESIAN_POINT ( 'NONE',  ( -4.762550801365593500, 2.752080473201636845, -2.228590825266444142 ) ) ;
#620 = ORIENTED_EDGE ( 'NONE', *, *, #22042, .F. ) ;
#621 = CARTESIAN_POINT ( 'NONE',  ( -3.554531657079157192, 3.105402419394639235, -0.9198621039125850496 ) ) ;
#622 = CIRCLE ( 'NONE', #17698, 5.010000000000000675 ) ;
#623 = CYLINDRICAL_SURFACE ( 'NONE', #32243, 6.000000000000000888 ) ;
#624 = AXIS2_PLACEMENT_3D ( 'NONE', #18416, #31291, #8364 ) ;
#625 = LINE ( 'NONE', #28375, #22614 ) ;
#626 = CARTESIAN_POINT ( 'NONE',  ( 10.65647057407925935, -13.03481288881981470, 1.500000000000000000 ) ) ;
#627 = ORIENTED_EDGE ( 'NONE', *, *, #2224, .F. ) ;
#628 = LINE ( 'NONE', #13792, #10850 ) ;
#629 = AXIS2_PLACEMENT_3D ( 'NONE', #5301, #20695, #17660 ) ;
#631 = ADVANCED_FACE ( 'NONE', ( #20899 ), #8359, .T. ) ;
#630 = AXIS2_PLACEMENT_3D ( 'NONE', #19998, #29844, #32868 ) ;
#632 = CC_DESIGN_PERSON_AND_ORGANIZATION_ASSIGNMENT ( #14954, #2785, ( #16786 ) ) ;
#633 = AXIS2_PLACEMENT_3D ( 'NONE', #749, #3096, #10588 ) ;
#634 =( BOUNDED_CURVE ( )  B_SPLINE_CURVE ( 2, ( #16762, #19452, #22119, #14577, #26963, #32332, #9391, #29801, #17064, #15388, #15560 ),
 .UNSPECIFIED., .F., .F. ) 
 B_SPLINE_CURVE_WITH_KNOTS ( ( 3, 2, 2, 2, 2, 3 ),
 ( 0.6966116191895003196, 0.6999999999999999556, 0.7249999999999999778, 0.7500000000000000000, 0.7750000000000000222, 0.7966116191895004084 ),
 .UNSPECIFIED. ) 
 CURVE ( )  GEOMETRIC_REPRESENTATION_ITEM ( )  RATIONAL_B_SPLINE_CURVE ( ( 0.9821626249036858880, 0.9896829947469992783, 1.000000000000000000, 0.9238795325112867385, 1.000000000000000000, 0.9238795325112867385, 1.000000000000000000, 0.9238795325112867385, 1.000000000000000000, 0.9341965377642874602, 0.9821626249036858880 ) ) 
 REPRESENTATION_ITEM ( '' )  );
#635 = VERTEX_POINT ( 'NONE', #15729 ) ;
#636 = CARTESIAN_POINT ( 'NONE',  ( 1.073911348006138189, -2.620901292623725176, 1.760914277779327852 ) ) ;
#637 = PERSON_AND_ORGANIZATION ( #6766, #25292 ) ;
#638 = CARTESIAN_POINT ( 'NONE',  ( 85.03224897449447894, -5.146568951867915409, 4.073740955748646364 ) ) ;
#639 = AXIS2_PLACEMENT_3D ( 'NONE', #9264, #19485, #29678 ) ;
#640 = CIRCLE ( 'NONE', #21982, 8.749000000000002331 ) ;
#641 = AXIS2_PLACEMENT_3D ( 'NONE', #19095, #4668, #2156 ) ;
#642 = CARTESIAN_POINT ( 'NONE',  ( 5.887529755120531227, -8.194579018285280014, -1.823049025159271030 ) ) ;
#643 = DIRECTION ( 'NONE',  ( -1.000000000000000000, -0.000000000000000000, 0.000000000000000000 ) ) ;
#644 = ORIENTED_EDGE ( 'NONE', *, *, #3720, .T. ) ;
#645 = CARTESIAN_POINT ( 'NONE',  ( 107.6936962044510437, -18.97455700431297743, -4.522180800239018694 ) ) ;
#646 = CARTESIAN_POINT ( 'NONE',  ( 26.08945412691625165, 19.05746434167071612, -1.104107218669578838 ) ) ;
#647 = EDGE_CURVE ( 'NONE', #29104, #11269, #16022, .T. ) ;
#648 = CARTESIAN_POINT ( 'NONE',  ( 2.589202944057205968, -7.715757980413516570, -6.846250362091614861 ) ) ;
#650 = ORIENTED_EDGE ( 'NONE', *, *, #29595, .F. ) ;
#649 = CARTESIAN_POINT ( 'NONE',  ( 22.50111451137534502, -3.256483526998273983E-15, 2.499999999999998668 ) ) ;
#651 = VECTOR ( 'NONE', #390, 1000.000000000000000 ) ;
#652 = CARTESIAN_POINT ( 'NONE',  ( -3.312550801365593767, -1.088641768524163389, -3.675193018007246071 ) ) ;
#653 = B_SPLINE_SURFACE_WITH_KNOTS ( 'NONE', 3, 3, ( 
 ( #5901, #17970, #28158, #18296, #756, #15621, #31007, #8088, #16091, #15434 ),
 ( #25834, #26324, #2957, #28315, #10939, #23314, #28505, #26145, #3102, #23459 ),
 ( #566, #10757, #21141, #31191, #8273, #19272, #9234, #8753, #18779, #9052 ),
 ( #6575, #23945, #11248, #16772, #29297, #26626, #28989, #23798, #911, #19109 ) ),
 .UNSPECIFIED., .F., .F., .F.,
 ( 4, 4 ),
 ( 4, 3, 3, 4 ),
 ( -1.565413741823433983E-11, 1.000000000000000444 ),
 ( 0.003584360682152736184, 0.5017921803410764214, 0.7508960901705381552, 1.000000000000000000 ),
 .UNSPECIFIED. ) ;
#654 = VECTOR ( 'NONE', #21945, 1000.000000000000000 ) ;
#655 = DIRECTION ( 'NONE',  ( 1.000000000000000000, 0.000000000000000000, 0.000000000000000000 ) ) ;
#656 = CARTESIAN_POINT ( 'NONE',  ( 29.21679767122667570, -7.327048195454283430, -2.787782193710479195 ) ) ;
#657 = EDGE_CURVE ( 'NONE', #8978, #937, #27438, .T. ) ;
#658 = CIRCLE ( 'NONE', #13443, 0.8000000000000182521 ) ;
#659 = ORIENTED_EDGE ( 'NONE', *, *, #8107, .T. ) ;
#660 = VERTEX_POINT ( 'NONE', #18554 ) ;
#661 = VECTOR ( 'NONE', #32653, 1000.000000000000000 ) ;
#662 = VECTOR ( 'NONE', #6430, 999.9999999999998863 ) ;
#664 = CIRCLE ( 'NONE', #2262, 8.750000000000000000 ) ;
#663 = CARTESIAN_POINT ( 'NONE',  ( 0.3076689118644541643, -4.089891983583716417, 9.439351442249007462 ) ) ;
#665 = CARTESIAN_POINT ( 'NONE',  ( 108.1329823800173102, -19.98427530701518506, -1.262026545339949957 ) ) ;
#666 = CIRCLE ( 'NONE', #7043, 6.248999999999999666 ) ;
#667 = DIRECTION ( 'NONE',  ( -1.000000000000000000, 0.000000000000000000, 0.000000000000000000 ) ) ;
#668 = CIRCLE ( 'NONE', #25743, 5.009999999999999787 ) ;
#669 = CARTESIAN_POINT ( 'NONE',  ( 1.265925305626725584E-16, 1.476463073999702669, -4.787500056513350977 ) ) ;
#670 = CARTESIAN_POINT ( 'NONE',  ( 19.01480233880980819, -3.011762293215293429, -0.07017451552781921176 ) ) ;
#671 = DIRECTION ( 'NONE',  ( 0.4999999999999981126, 0.8660254037844395958, -0.000000000000000000 ) ) ;
#672 = CARTESIAN_POINT ( 'NONE',  ( 23.62103335626344958, -7.897478826046258504, 1.169950778987780771 ) ) ;
#673 = ORIENTED_EDGE ( 'NONE', *, *, #10837, .T. ) ;
#674 = CARTESIAN_POINT ( 'NONE',  ( 5.612718622971679672, -2.621884781721320223, 7.786491723834104484 ) ) ;
#675 = AXIS2_PLACEMENT_3D ( 'NONE', #17353, #9979, #19861 ) ;
#676 = ORIENTED_EDGE ( 'NONE', *, *, #29431, .T. ) ;
#678 = CIRCLE ( 'NONE', #32185, 8.500000000000000000 ) ;
#677 = APPROVAL_STATUS ( 'not_yet_approved' ) ;
#679 = CARTESIAN_POINT ( 'NONE',  ( 41.43709133142961321, -4.769546740945156849, 4.522129901861162260 ) ) ;
#680 = AXIS2_PLACEMENT_3D ( 'NONE', #6810, #29224, #6310 ) ;
#681 = VERTEX_POINT ( 'NONE', #28912 ) ;
#682 = AXIS2_PLACEMENT_3D ( 'NONE', #9016, #19424, #19236 ) ;
#683 = AXIS2_PLACEMENT_3D ( 'NONE', #25151, #12274, #10094 ) ;
#684 = DIRECTION ( 'NONE',  ( 1.000000000000000000, 0.000000000000000000, 0.000000000000000000 ) ) ;
#685 = VERTEX_POINT ( 'NONE', #6019 ) ;
#686 = CARTESIAN_POINT ( 'NONE',  ( 5.240875073191910261, 0.000000000000000000, 3.405250132838362642 ) ) ;
#688 = ORIENTED_EDGE ( 'NONE', *, *, #22874, .T. ) ;
#687 = CARTESIAN_POINT ( 'NONE',  ( 54.94807382917689154, -5.453310457255624577, -4.112224493141035886 ) ) ;
#689 = VERTEX_POINT ( 'NONE', #26432 ) ;
#690 = CARTESIAN_POINT ( 'NONE',  ( 0.000000000000000000, -0.5000000000000000000, -1.000000000000000000 ) ) ;
#691 = CARTESIAN_POINT ( 'NONE',  ( -3.262550801365593056, 0.3701630799359330593, -3.521866450007987037 ) ) ;
#692 = EDGE_CURVE ( 'NONE', #389, #11133, #17844, .T. ) ;
#693 = CARTESIAN_POINT ( 'NONE',  ( 25.85999999999999943, 1.573300977624590313, -1.942864903642426144 ) ) ;
#694 = AXIS2_PLACEMENT_3D ( 'NONE', #1892, #22262, #9533 ) ;
#695 = CARTESIAN_POINT ( 'NONE',  ( 0.4213074008609886123, -4.489821273616160902, -1.766536014443793157 ) ) ;
#697 = VERTEX_POINT ( 'NONE', #21084 ) ;
#696 = DIRECTION ( 'NONE',  ( 0.000000000000000000, -0.9271838545667856479, -0.3746065934159165667 ) ) ;
#698 = CARTESIAN_POINT ( 'NONE',  ( 0.000000000000000000, 0.6700234925293840904, -8.473551116235670477 ) ) ;
#699 = CARTESIAN_POINT ( 'NONE',  ( 10.13822877939487199, 2.318259723584965570, 1.500000000000000000 ) ) ;
#700 = ADVANCED_FACE ( 'NONE', ( #21232 ), #3532, .T. ) ;
#701 = CARTESIAN_POINT ( 'NONE',  ( 17.33093461831356663, -21.43932300456619799, 1.499999999999999112 ) ) ;
#702 = CARTESIAN_POINT ( 'NONE',  ( 0.000000000000000000, 0.000000000000000000, 0.000000000000000000 ) ) ;
#703 = DIRECTION ( 'NONE',  ( 1.000000000000000000, -8.574039729943018344E-17, -0.000000000000000000 ) ) ;
#705 = ORIENTED_EDGE ( 'NONE', *, *, #743, .T. ) ;
#704 = FACE_OUTER_BOUND ( 'NONE', #14822, .T. ) ;
#706 = CARTESIAN_POINT ( 'NONE',  ( 3.020080181664714924, -8.342499971020062688, 3.262125172866680245 ) ) ;
#707 = CIRCLE ( 'NONE', #23645, 12.49867430706168570 ) ;
#708 = CIRCLE ( 'NONE', #24193, 10.97000000000000064 ) ;
#709 = FACE_OUTER_BOUND ( 'NONE', #8742, .T. ) ;
#710 = CARTESIAN_POINT ( 'NONE',  ( 24.79750000273118715, -2.594547506269383685, -0.7685399846772043020 ) ) ;
#711 = AXIS2_PLACEMENT_3D ( 'NONE', #8425, #28665, #3261 ) ;
#712 = AXIS2_PLACEMENT_3D ( 'NONE', #24711, #32423, #22364 ) ;
#713 = CARTESIAN_POINT ( 'NONE',  ( -22.68133094298037378, 3.998227953278250535, 2.146185852361514268 ) ) ;
#714 = AXIS2_PLACEMENT_3D ( 'NONE', #13186, #23388, #20888 ) ;
#715 = DIRECTION ( 'NONE',  ( 0.000000000000000000, 0.000000000000000000, 1.000000000000000000 ) ) ;
#716 = CARTESIAN_POINT ( 'NONE',  ( -2.910169157840587939, 0.01692106640608362356, -0.9265120394754853272 ) ) ;
#717 = DIRECTION ( 'NONE',  ( 0.09975574163943258521, -0.1727820128662111709, 0.9798954883250903247 ) ) ;
#718 = VECTOR ( 'NONE', #3334, 1000.000000000000000 ) ;
#719 = VECTOR ( 'NONE', #6939, 1000.000000000000000 ) ;
#720 = DIRECTION ( 'NONE',  ( -1.000000000000000000, 8.574039729943018344E-17, -3.081487911019577365E-33 ) ) ;
#721 = ORIENTED_EDGE ( 'NONE', *, *, #28942, .F. ) ;
#722 = DIRECTION ( 'NONE',  ( -1.000000000000000000, 0.000000000000000000, 0.000000000000000000 ) ) ;
#723 = CARTESIAN_POINT ( 'NONE',  ( 40.74410603220335503, -8.021703207526138968, -2.184955501622229068 ) ) ;
#724 = CARTESIAN_POINT ( 'NONE',  ( 101.9216173105994443, -5.769792427975428240, -0.07017451552783622593 ) ) ;
#726 = CARTESIAN_POINT ( 'NONE',  ( 107.4617763835125430, -17.53021834753707964, 4.828547747425045777 ) ) ;
#725 = CARTESIAN_POINT ( 'NONE',  ( 0.7632845268398871230, -3.174628368996133876, 8.152713396088751452 ) ) ;
#727 = ORIENTED_EDGE ( 'NONE', *, *, #28371, .F. ) ;
#728 = B_SPLINE_CURVE_WITH_KNOTS ( 'NONE', 3,
 ( #7940, #18129, #5442, #15635, #1066, #29001, #26493, #6100, #31020, #18311, #23647, #8763, #426, #5914, #13122, #18477, #21469, #8428, #31499, #29155, #16280, #8584, #10951, #10606, #23808, #28668, #21153, #6243, #3592, #13602, #31351, #18623 ),
 .UNSPECIFIED., .F., .F.,
 ( 4, 2, 2, 2, 2, 2, 2, 2, 2, 2, 2, 2, 2, 2, 2, 4 ),
 ( 0.0002608162019139872436, 0.0007834053667116245385, 0.001305994531509261942, 0.001828583696306898803, 0.002351172861104536532, 0.002873762025902174260, 0.003396351190699811555, 0.003918940355497449284, 0.004441529520295087012, 0.004964118685092724741, 0.005486707849890363337, 0.006009297014688001065, 0.006531886179485638794, 0.007577064509080915986, 0.008099653673878555449, 0.008622242838676193177 ),
 .UNSPECIFIED. ) ;
#729 = AXIS2_PLACEMENT_3D ( 'NONE', #23943, #14238, #31981 ) ;
#730 = CARTESIAN_POINT ( 'NONE',  ( -3.122314033877847442E-16, -3.641590349731908649, -3.055657119358837992 ) ) ;
#731 = VECTOR ( 'NONE', #17523, 1000.000000000000000 ) ;
#732 = ORIENTED_EDGE ( 'NONE', *, *, #5555, .F. ) ;
#733 = CARTESIAN_POINT ( 'NONE',  ( 3.249999999999999556, -9.314797388894900720, 5.239665997526856245 ) ) ;
#734 = AXIS2_PLACEMENT_3D ( 'NONE', #26761, #722, #9023 ) ;
#736 = ORIENTED_EDGE ( 'NONE', *, *, #30321, .F. ) ;
#735 = FACE_OUTER_BOUND ( 'NONE', #6838, .T. ) ;
#737 = ORIENTED_EDGE ( 'NONE', *, *, #21414, .T. ) ;
#738 = CARTESIAN_POINT ( 'NONE',  ( 0.000000000000000000, 0.000000000000000000, 0.000000000000000000 ) ) ;
#739 = AXIS2_PLACEMENT_3D ( 'NONE', #29345, #19505, #16967 ) ;
#740 = EDGE_CURVE ( 'NONE', #28886, #23895, #13196, .T. ) ;
#741 = VECTOR ( 'NONE', #14947, 1000.000000000000000 ) ;
#743 = EDGE_CURVE ( 'NONE', #9413, #2672, #27116, .T. ) ;
#742 = VECTOR ( 'NONE', #14344, 1000.000000000000114 ) ;
#744 = DIRECTION ( 'NONE',  ( 0.7222222222222246524, 0.000000000000000000, -0.6916610887771492688 ) ) ;
#746 = ORIENTED_EDGE ( 'NONE', *, *, #27778, .F. ) ;
#745 = CARTESIAN_POINT ( 'NONE',  ( 107.7872093323711340, 16.99325752433615122, 1.795912459692029950 ) ) ;
#747 = ORIENTED_EDGE ( 'NONE', *, *, #22464, .F. ) ;
#748 = CARTESIAN_POINT ( 'NONE',  ( -0.9904391912309036261, -13.96299501477513694, -1.744689047112403024 ) ) ;
#749 = CARTESIAN_POINT ( 'NONE',  ( 3.499999999999999556, 0.000000000000000000, 0.000000000000000000 ) ) ;
#750 = APPROVAL_PERSON_ORGANIZATION ( #21716, #28044, #12024 ) ;
#751 = CARTESIAN_POINT ( 'NONE',  ( 23.15368348410971677, -16.86203458189143944, -1.500000000001110223 ) ) ;
#752 = CARTESIAN_POINT ( 'NONE',  ( 107.8942783567389796, -16.54699675389560909, -1.787313614190034539 ) ) ;
#753 = DIRECTION ( 'NONE',  ( 8.541412920197221047E-17, 0.9961946980917459893, -0.08715574274765196250 ) ) ;
#754 = CARTESIAN_POINT ( 'NONE',  ( 3.499999999999999556, 0.000000000000000000, 0.000000000000000000 ) ) ;
#755 = CARTESIAN_POINT ( 'NONE',  ( 0.7529060732733400263, -8.134409449814636872, 1.500000000000000222 ) ) ;
#756 = CARTESIAN_POINT ( 'NONE',  ( 47.94941403272063951, -7.827919050483855834, 2.184956529741820752 ) ) ;
#757 = CARTESIAN_POINT ( 'NONE',  ( 5.612718622971678784, 7.786491723834110701, 2.621884781721292246 ) ) ;
#758 = CARTESIAN_POINT ( 'NONE',  ( 3.295700863922491841, -0.1006852655820335979, 1.307585114970543527 ) ) ;
#759 = VECTOR ( 'NONE', #9903, 1000.000000000000000 ) ;
#760 = ORIENTED_EDGE ( 'NONE', *, *, #21404, .F. ) ;
#761 = AXIS2_PLACEMENT_3D ( 'NONE', #16484, #14658, #22192 ) ;
#762 = CARTESIAN_POINT ( 'NONE',  ( 2.274274201625309910, -10.90201369670500853, -1.464956435139685098 ) ) ;
#763 = CIRCLE ( 'NONE', #8227, 2.999999999999999556 ) ;
#764 = CARTESIAN_POINT ( 'NONE',  ( 107.8403069886983161, 17.28892622638833032, 3.587457385742634841 ) ) ;
#765 = CARTESIAN_POINT ( 'NONE',  ( 13.62547635268498780, 21.94000000000002970, -1.050000000000000044 ) ) ;
#766 = ORIENTED_EDGE ( 'NONE', *, *, #18502, .F. ) ;
#767 = CARTESIAN_POINT ( 'NONE',  ( 21.73500000136559507, 3.156283516753366047, 0.9349337715887203748 ) ) ;
#768 = FACE_OUTER_BOUND ( 'NONE', #20677, .T. ) ;
#769 = CARTESIAN_POINT ( 'NONE',  ( 15.28872660057386845, 20.76088595412476678, -4.612695725900422872 ) ) ;
#770 = CC_DESIGN_SECURITY_CLASSIFICATION ( #27439, ( #2373 ) ) ;
#771 = ORIENTED_EDGE ( 'NONE', *, *, #7007, .F. ) ;
#772 = CARTESIAN_POINT ( 'NONE',  ( 21.08401840680096129, -16.78474387324269657, -1.500000000000000000 ) ) ;
#773 = VERTEX_POINT ( 'NONE', #29749 ) ;
#774 = EDGE_CURVE ( 'NONE', #4552, #3662, #6328, .T. ) ;
#775 = EDGE_LOOP ( 'NONE', ( #2601, #31681, #22240, #22954, #30437 ) ) ;
#776 = DIRECTION ( 'NONE',  ( -0.1908089953765452762, 4.720536385445197917E-14, 0.9816271834476639757 ) ) ;
#777 = APPROVAL_STATUS ( 'not_yet_approved' ) ;
#779 = ORIENTED_EDGE ( 'NONE', *, *, #24719, .T. ) ;
#778 = CARTESIAN_POINT ( 'NONE',  ( 23.25111450864416085, -3.256483526998273983E-15, 2.499999999999998668 ) ) ;
#780 = VERTEX_POINT ( 'NONE', #19708 ) ;
#781 = DIRECTION ( 'NONE',  ( -1.000000000000000000, 0.000000000000000000, 0.000000000000000000 ) ) ;
#782 = EDGE_CURVE ( 'NONE', #21865, #32461, #19232, .T. ) ;
#783 = ORIENTED_EDGE ( 'NONE', *, *, #1125, .F. ) ;
#784 = CARTESIAN_POINT ( 'NONE',  ( -7.706376978575948833, 0.1572233378491243172, -2.999999999999999556 ) ) ;
#785 = AXIS2_PLACEMENT_3D ( 'NONE', #10480, #20693, #30894 ) ;
#787 = ORIENTED_EDGE ( 'NONE', *, *, #30846, .T. ) ;
#786 = CARTESIAN_POINT ( 'NONE',  ( 102.2339617642410872, -1.281710854344942918, -1.169950773171123615 ) ) ;
#788 = DIRECTION ( 'NONE',  ( 0.4999999999999978906, 0.8660254037844398178, 0.000000000000000000 ) ) ;
#789 = CARTESIAN_POINT ( 'NONE',  ( 6.524595126109736576, 0.8869162863045649825, -8.613374939462815405 ) ) ;
#790 = ADVANCED_FACE ( 'NONE', ( #27408, #9160 ), #14183, .F. ) ;
#791 = DIRECTION ( 'NONE',  ( 1.000000000000000000, -8.574039729943018344E-17, -0.000000000000000000 ) ) ;
#792 = LINE ( 'NONE', #25869, #9780 ) ;
#793 = CARTESIAN_POINT ( 'NONE',  ( -10.00000000000000000, 0.000000000000000000, 0.000000000000000000 ) ) ;
#794 = B_SPLINE_CURVE_WITH_KNOTS ( 'NONE', 3,
 ( #24093, #31175, #8737, #21611, #11413, #29134 ),
 .UNSPECIFIED., .F., .F.,
 ( 4, 2, 4 ),
 ( 2.337797342572514391E-16, 0.001737887880030562987, 0.003475775760060892221 ),
 .UNSPECIFIED. ) ;
#795 = ORIENTED_EDGE ( 'NONE', *, *, #32126, .F. ) ;
#796 = LINE ( 'NONE', #23831, #12832 ) ;
#797 = DIRECTION ( 'NONE',  ( -8.326672684688674053E-17, -0.3746065934159164001, 0.9271838545667857590 ) ) ;
#798 = ADVANCED_FACE ( 'NONE', ( #16866 ), #27219, .F. ) ;
#799 = CARTESIAN_POINT ( 'NONE',  ( -34.62197427260419857, 18.00000000000000355, 0.3975189810868542395 ) ) ;
#800 = CARTESIAN_POINT ( 'NONE',  ( 3.499999999999999556, 6.226349476952025341, 0.5315761383463585288 ) ) ;
#801 = LOCAL_TIME ( 16, 7, 10.00000000000000000, #2461 ) ;
#802 = DIRECTION ( 'NONE',  ( 0.9842544651762055175, -0.1767573132311700268, 0.000000000000000000 ) ) ;
#803 = CARTESIAN_POINT ( 'NONE',  ( 0.000000000000000000, -25.93932300454937945, 11.50000000000000000 ) ) ;
#804 = DIRECTION ( 'NONE',  ( -1.000000000000000000, -0.000000000000000000, -0.000000000000000000 ) ) ;
#805 = DIRECTION ( 'NONE',  ( 0.000000000000000000, -1.000000000000000000, 0.000000000000000000 ) ) ;
#806 = CARTESIAN_POINT ( 'NONE',  ( 40.87351160865108568, -4.997573076398440506, 2.787782134468652639 ) ) ;
#807 = CARTESIAN_POINT ( 'NONE',  ( -2.312550801365593767, 3.675193018007247403, -1.088641768524161391 ) ) ;
#808 = ORIENTED_EDGE ( 'NONE', *, *, #4569, .T. ) ;
#809 = CARTESIAN_POINT ( 'NONE',  ( -6.300050800000000173, -2.983565686104819648, -0.3135853898029605791 ) ) ;
#810 = VECTOR ( 'NONE', #16884, 1000.000000000000000 ) ;
#811 = EDGE_CURVE ( 'NONE', #9973, #29226, #28846, .T. ) ;
#812 = CARTESIAN_POINT ( 'NONE',  ( 107.6454270328456602, 19.04591414929136306, 5.010299225411025681 ) ) ;
#813 = FACE_OUTER_BOUND ( 'NONE', #16299, .T. ) ;
#814 = CARTESIAN_POINT ( 'NONE',  ( 8.323087564152990225, -11.23204384871645445, 1.500000000000000000 ) ) ;
#815 = ORIENTED_EDGE ( 'NONE', *, *, #4615, .T. ) ;
#816 = CARTESIAN_POINT ( 'NONE',  ( 18.96091535642496240, -3.614110606601104614, -2.184956778830005053 ) ) ;
#817 = ORIENTED_EDGE ( 'NONE', *, *, #14859, .T. ) ;
#818 = DIRECTION ( 'NONE',  ( 1.000000000000000000, 1.369475477426763776E-16, -4.370874484540404848E-33 ) ) ;
#819 = APPROVAL_STATUS ( 'not_yet_approved' ) ;
#820 = ADVANCED_FACE ( 'NONE', ( #14690 ), #3843, .T. ) ;
#821 = CARTESIAN_POINT ( 'NONE',  ( 69.03558484035113452, -5.418257723523708158, 4.312042181588143563 ) ) ;
#822 = EDGE_CURVE ( 'NONE', #24398, #8881, #4333, .T. ) ;
#823 = CARTESIAN_POINT ( 'NONE',  ( 5.377543748152551650, -7.892520144992426268, -1.391664247347309535 ) ) ;
#824 = DIRECTION ( 'NONE',  ( -1.000000000000000000, 0.000000000000000000, -0.000000000000000000 ) ) ;
#825 = EDGE_LOOP ( 'NONE', ( #8438, #11419, #17829, #28728, #15049 ) ) ;
#826 = EDGE_CURVE ( 'NONE', #25076, #23417, #2306, .T. ) ;
#827 = DIRECTION ( 'NONE',  ( -1.000000000000000000, 0.000000000000000000, 0.000000000000000000 ) ) ;
#828 = CARTESIAN_POINT ( 'NONE',  ( -3.830085165118321606E-16, -4.467071865485483961, 1.625881193364682620 ) ) ;
#829 = CARTESIAN_POINT ( 'NONE',  ( 9.172108879787138846, -0.1070445578126106578, 1.318121098349317233 ) ) ;
#831 = ORIENTED_EDGE ( 'NONE', *, *, #14747, .T. ) ;
#830 = CARTESIAN_POINT ( 'NONE',  ( 3.499999999999999556, -7.009698679648281860, -0.7308381473897611613 ) ) ;
#832 = CARTESIAN_POINT ( 'NONE',  ( -2.162550801365593856, 2.228590825266444142, 2.752080473201636845 ) ) ;
#833 = CARTESIAN_POINT ( 'NONE',  ( 0.000000000000000000, 9.680994141368845618, -5.222868219166749704 ) ) ;
#834 = CARTESIAN_POINT ( 'NONE',  ( 1.624999999999999778, -1.975651141462163807, -10.82112760146738495 ) ) ;
#835 = ORIENTED_EDGE ( 'NONE', *, *, #5183, .F. ) ;
#836 = ORIENTED_EDGE ( 'NONE', *, *, #20671, .T. ) ;
#837 = EDGE_CURVE ( 'NONE', #5413, #9418, #4165, .T. ) ;
#838 = DIRECTION ( 'NONE',  ( -0.000000000000000000, -0.08715574274766219043, 0.9961946980917452121 ) ) ;
#839 = CARTESIAN_POINT ( 'NONE',  ( -31.57659242536668032, -21.43932300455408679, -1.500000000000000000 ) ) ;
#840 = CARTESIAN_POINT ( 'NONE',  ( 0.7294883270165408717, -11.94795532514693548, 5.485967528433933538 ) ) ;
#841 = ORIENTED_EDGE ( 'NONE', *, *, #657, .F. ) ;
#842 = DIRECTION ( 'NONE',  ( 0.000000000000000000, 0.000000000000000000, 1.000000000000000000 ) ) ;
#843 = CARTESIAN_POINT ( 'NONE',  ( 0.6791198108364924213, -8.522429291907473115, 3.345077512921551754 ) ) ;
#844 = CARTESIAN_POINT ( 'NONE',  ( -58.24607230066835228, -3.627201876406635606, 5.444121653535032301 ) ) ;
#845 =( BOUNDED_CURVE ( )  B_SPLINE_CURVE ( 3, ( #15367, #15720, #25573, #27743 ),
 .UNSPECIFIED., .F., .T. ) 
 B_SPLINE_CURVE_WITH_KNOTS ( ( 4, 4 ),
 ( 0.6009777071441372298, 1.570796326794896558 ),
 .UNSPECIFIED. ) 
 CURVE ( )  GEOMETRIC_REPRESENTATION_ITEM ( )  RATIONAL_B_SPLINE_CURVE ( ( 1.000000000000000000, 0.9231448173252677636, 0.9231448173252677636, 1.000000000000000000 ) ) 
 REPRESENTATION_ITEM ( '' )  );
#846 = CARTESIAN_POINT ( 'NONE',  ( -3.287550801365593856, 2.752080473201636845, -2.228590825266444142 ) ) ;
#847 = CARTESIAN_POINT ( 'NONE',  ( -61.24371088333262492, -10.96999999999998643, 1.500000000000000000 ) ) ;
#848 = FACE_OUTER_BOUND ( 'NONE', #25602, .T. ) ;
#849 = ORIENTED_EDGE ( 'NONE', *, *, #26141, .F. ) ;
#850 = CARTESIAN_POINT ( 'NONE',  ( 5.489343958331428297, -2.678936089601496207, 7.664144799260943053 ) ) ;
#851 = EDGE_CURVE ( 'NONE', #23090, #29352, #14400, .T. ) ;
#852 = ORIENTED_EDGE ( 'NONE', *, *, #8382, .T. ) ;
#853 = COORDINATED_UNIVERSAL_TIME_OFFSET ( 0, 0, .AHEAD. ) ;
#854 = EDGE_CURVE ( 'NONE', #11874, #1933, #8468, .T. ) ;
#855 = CARTESIAN_POINT ( 'NONE',  ( 40.88398074938778137, -6.894607256478876955, 3.996604168373521837 ) ) ;
#856 = CARTESIAN_POINT ( 'NONE',  ( 8.285115449721931924, -10.40907249743529661, -1.000000000000000000 ) ) ;
#857 = ORIENTED_EDGE ( 'NONE', *, *, #25958, .F. ) ;
#858 = CARTESIAN_POINT ( 'NONE',  ( 0.3749743548326627818, -10.05686762493553488, 0.8908839545094129342 ) ) ;
#859 = ORIENTED_EDGE ( 'NONE', *, *, #4261, .T. ) ;
#860 = ORIENTED_EDGE ( 'NONE', *, *, #3468, .F. ) ;
#861 = FACE_OUTER_BOUND ( 'NONE', #4593, .T. ) ;
#862 = CARTESIAN_POINT ( 'NONE',  ( -4.362550801365593145, -2.752080473201636845, 2.228590825266444586 ) ) ;
#863 = CARTESIAN_POINT ( 'NONE',  ( 7.249760686538667009, -7.953573330858190182, -3.647351267791651974 ) ) ;
#864 = CARTESIAN_POINT ( 'NONE',  ( 0.000000000000000000, -6.478011392632841314, -6.807171995660652009 ) ) ;
#866 = VERTEX_POINT ( 'NONE', #1849 ) ;
#865 = CARTESIAN_POINT ( 'NONE',  ( 24.72695737054825926, 18.91229966141139229, -1.500000000000000000 ) ) ;
#867 = CARTESIAN_POINT ( 'NONE',  ( -5.137550801365594388, -3.368539882008727115, -1.828967928396028064 ) ) ;
#868 = CARTESIAN_POINT ( 'NONE',  ( 13.86820176991295739, 7.731990000458505818, 1.500000000000000000 ) ) ;
#869 = CARTESIAN_POINT ( 'NONE',  ( 15.95505479268522642, -20.93460661231094733, 1.499999999995777378 ) ) ;
#870 = DIRECTION ( 'NONE',  ( -1.000000000000000000, 8.574039729943018344E-17, 0.000000000000000000 ) ) ;
#872 = EDGE_LOOP ( 'NONE', ( #15387, #30686 ) ) ;
#871 = CARTESIAN_POINT ( 'NONE',  ( 21.59559372541029276, -17.25941758357585698, 1.753144073645959145 ) ) ;
#873 = EDGE_CURVE ( 'NONE', #7332, #32468, #32589, .T. ) ;
#874 = CC_DESIGN_PERSON_AND_ORGANIZATION_ASSIGNMENT ( #25929, #25425, ( #17492 ) ) ;
#875 = DIRECTION ( 'NONE',  ( 0.000000000000000000, 0.000000000000000000, -1.000000000000000000 ) ) ;
#876 = CARTESIAN_POINT ( 'NONE',  ( 22.86000000273118715, -1.942864903642428587, -1.573300977624592756 ) ) ;
#877 = CARTESIAN_POINT ( 'NONE',  ( -17.10362080823519904, 9.298459344128380266, 1.499999999999894529 ) ) ;
#878 = CARTESIAN_POINT ( 'NONE',  ( 16.36487458112949511, 19.37645981759117575, 4.629213727441584325 ) ) ;
#879 = CARTESIAN_POINT ( 'NONE',  ( 0.9499999999999995115, 0.000000000000000000, -6.999999999999998224 ) ) ;
#880 = CARTESIAN_POINT ( 'NONE',  ( 10.00000000000000000, 3.055657119358849094, -3.641590349731898879 ) ) ;
#881 = LINE ( 'NONE', #23597, #20986 ) ;
#882 = CARTESIAN_POINT ( 'NONE',  ( -5.887550801365593500, -2.228590825266444586, -2.752080473201636401 ) ) ;
#883 = EDGE_LOOP ( 'NONE', ( #21962, #13403, #22343, #14448, #9426 ) ) ;
#884 = ADVANCED_FACE ( 'NONE', ( #20061 ), #30103, .T. ) ;
#885 = CARTESIAN_POINT ( 'NONE',  ( 19.69555400981542803, -21.64588847999043253, 1.456500879219768452 ) ) ;
#886 = EDGE_CURVE ( 'NONE', #10135, #4581, #22553, .T. ) ;
#887 = CARTESIAN_POINT ( 'NONE',  ( 101.8797206818349821, -5.166491396337139719, -2.184956718990371805 ) ) ;
#888 = DIRECTION ( 'NONE',  ( 6.062761635205596708E-17, 0.7071067811865490160, -0.7071067811865460184 ) ) ;
#890 = CARTESIAN_POINT ( 'NONE',  ( 107.4977942790300460, -18.05374091625411026, 5.138025335311863451 ) ) ;
#889 = CARTESIAN_POINT ( 'NONE',  ( 1.624999999999999778, 1.975651141462238414, 10.82112760146736896 ) ) ;
#891 = ORIENTED_EDGE ( 'NONE', *, *, #15986, .F. ) ;
#892 = CARTESIAN_POINT ( 'NONE',  ( -15.51216819290874227, 0.000000000000000000, 1.500000000000000000 ) ) ;
#893 = ORIENTED_EDGE ( 'NONE', *, *, #25791, .T. ) ;
#894 = CARTESIAN_POINT ( 'NONE',  ( 0.000000000000000000, -6.807171995660538322, -6.478011392632959442 ) ) ;
#896 = EDGE_LOOP ( 'NONE', ( #4625, #17001, #16391, #439, #13609, #23483, #12341 ) ) ;
#895 = CYLINDRICAL_SURFACE ( 'NONE', #10132, 297.4345239564032681 ) ;
#897 = ORIENTED_EDGE ( 'NONE', *, *, #16464, .F. ) ;
#898 = CARTESIAN_POINT ( 'NONE',  ( 69.38611993481310947, -8.080330187063884395, -2.713652344655543391 ) ) ;
#899 = LINE ( 'NONE', #26780, #12884 ) ;
#901 = VERTEX_POINT ( 'NONE', #15003 ) ;
#900 = CARTESIAN_POINT ( 'NONE',  ( -34.99740252253902639, 0.5174497483512505713, 2.982117921349408007 ) ) ;
#902 = CARTESIAN_POINT ( 'NONE',  ( 14.62799800222094326, 9.826424398192026288, -1.500000000000000000 ) ) ;
#903 = CARTESIAN_POINT ( 'NONE',  ( -2.926117933286927375, 0.000000000000000000, -1.252246291852652682 ) ) ;
#904 = CARTESIAN_POINT ( 'NONE',  ( 0.000000000000000000, 6.226349476952025341, 0.5315761383463585288 ) ) ;
#905 = DIRECTION ( 'NONE',  ( 0.000000000000000000, 0.000000000000000000, 1.000000000000000000 ) ) ;
#906 = CARTESIAN_POINT ( 'NONE',  ( 107.9484595593237231, -17.32719259252710842, -4.525028783333800320 ) ) ;
#907 = CARTESIAN_POINT ( 'NONE',  ( 24.80306213860341558, -17.49230408913766865, 1.499999999999999778 ) ) ;
#908 =( BOUNDED_CURVE ( )  B_SPLINE_CURVE ( 2, ( #3312, #2835, #5963 ),
 .UNSPECIFIED., .F., .F. ) 
 B_SPLINE_CURVE_WITH_KNOTS ( ( 3, 3 ),
 ( 0.9966116191895003640, 1.000000000000000000 ),
 .UNSPECIFIED. ) 
 CURVE ( )  GEOMETRIC_REPRESENTATION_ITEM ( )  RATIONAL_B_SPLINE_CURVE ( ( 0.9821626249036858880, 0.9896829947469992783, 1.000000000000000000 ) ) 
 REPRESENTATION_ITEM ( '' )  );
#909 = LINE ( 'NONE', #32114, #29425 ) ;
#910 = CARTESIAN_POINT ( 'NONE',  ( 9.101556641444268791, 0.000000000000000000, 0.000000000000000000 ) ) ;
#911 = CARTESIAN_POINT ( 'NONE',  ( 23.71121667297767388, -6.322215142808032873, 3.993434336039484833 ) ) ;
#912 = CARTESIAN_POINT ( 'NONE',  ( -3.000050799999999906, -1.887961173149512062, -2.331437884370912261 ) ) ;
#913 = CARTESIAN_POINT ( 'NONE',  ( 2.712282326253089959, -0.4283266402567246223, 1.500000000000000444 ) ) ;
#914 = ORIENTED_EDGE ( 'NONE', *, *, #129, .T. ) ;
#915 = CARTESIAN_POINT ( 'NONE',  ( 6.524595395369781059, -3.538595500939536009, -7.902859683906648058 ) ) ;
#916 = DIRECTION ( 'NONE',  ( 0.000000000000000000, -1.224646799147352961E-16, 1.000000000000000000 ) ) ;
#917 = EDGE_CURVE ( 'NONE', #21913, #11133, #25114, .T. ) ;
#918 = FACE_OUTER_BOUND ( 'NONE', #5499, .T. ) ;
#919 = ORIENTED_EDGE ( 'NONE', *, *, #1785, .T. ) ;
#920 = CARTESIAN_POINT ( 'NONE',  ( 24.36000000136559507, -1.570731468192933633, -2.892927487894330074 ) ) ;
#921 = EDGE_CURVE ( 'NONE', #22025, #24661, #7837, .T. ) ;
#922 = EDGE_CURVE ( 'NONE', #4124, #22902, #28033, .T. ) ;
#923 = CARTESIAN_POINT ( 'NONE',  ( -15.51216819290874227, -25.44850941282521006, 1.500000000000000000 ) ) ;
#924 = ORIENTED_EDGE ( 'NONE', *, *, #10559, .F. ) ;
#925 = CARTESIAN_POINT ( 'NONE',  ( 5.489321708267614675, 6.285661071314543769, -5.138670926724834942 ) ) ;
#926 = VERTEX_POINT ( 'NONE', #32930 ) ;
#927 = ORIENTED_EDGE ( 'NONE', *, *, #23648, .F. ) ;
#928 = CARTESIAN_POINT ( 'NONE',  ( 5.887530024394195038, 3.218326717262362191, -7.753515897409855029 ) ) ;
#929 = B_SPLINE_SURFACE_WITH_KNOTS ( 'NONE', 1, 3, ( 
 ( #24414, #9994, #24573, #16743, #11708, #9375, #1887, #1698 ),
 ( #20370, #7474, #25388, #21910, #20206, #4373, #33072, #9205 ) ),
 .UNSPECIFIED., .F., .F., .F.,
 ( 2, 2 ),
 ( 4, 2, 2, 4 ),
 ( 0.000000000000000000, 1.000000000000000000 ),
 ( 0.000000000000000000, 0.5000000000000000000, 0.7500000000000000000, 1.000000000000000000 ),
 .UNSPECIFIED. ) ;
#931 = ORIENTED_EDGE ( 'NONE', *, *, #18046, .F. ) ;
#930 = CARTESIAN_POINT ( 'NONE',  ( -2.889143798725324785, 0.000000000000000000, -0.9788672205760856615 ) ) ;
#932 = ORIENTED_EDGE ( 'NONE', *, *, #14409, .T. ) ;
#933 = LINE ( 'NONE', #11451, #32119 ) ;
#934 = ORIENTED_EDGE ( 'NONE', *, *, #229, .F. ) ;
#935 = LINE ( 'NONE', #25672, #31041 ) ;
#937 = VERTEX_POINT ( 'NONE', #28069 ) ;
#936 = CARTESIAN_POINT ( 'NONE',  ( 102.2410647596622937, -1.384237843926474643, -1.529339869963366683 ) ) ;
#938 = CARTESIAN_POINT ( 'NONE',  ( 21.97280264420809814, -21.86582870483968577, 1.264433483335436481 ) ) ;
#939 = CARTESIAN_POINT ( 'NONE',  ( 12.44989959798868817, -0.06979899340500209104, 13.00000000000004441 ) ) ;
#940 = DIRECTION ( 'NONE',  ( -0.000000000000000000, -0.000000000000000000, 1.000000000000000000 ) ) ;
#941 = DIRECTION ( 'NONE',  ( -1.000000000000000000, -0.000000000000000000, 0.000000000000000000 ) ) ;
#942 = CARTESIAN_POINT ( 'NONE',  ( 107.5608083496522767, -18.96961453642471795, 4.558424976626936242 ) ) ;
#943 = PLANE ( 'NONE',  #31003 ) ;
#944 = CARTESIAN_POINT ( 'NONE',  ( -2.633834500755857455, -0.2542144740826015603, -1.655286495009812064 ) ) ;
#945 = CARTESIAN_POINT ( 'NONE',  ( 102.5401559989745266, -5.675509796544895735, -0.8105616764226521997 ) ) ;
#946 = DIRECTION ( 'NONE',  ( -1.000000000000000000, -0.000000000000000000, 0.000000000000000000 ) ) ;
#947 = EDGE_CURVE ( 'NONE', #7301, #24368, #1667, .T. ) ;
#948 = FACE_OUTER_BOUND ( 'NONE', #24455, .T. ) ;
#949 = FACE_OUTER_BOUND ( 'NONE', #14062, .T. ) ;
#950 = CARTESIAN_POINT ( 'NONE',  ( 0.5640493910588674220, -7.306425354229854285, -6.134141009809413347 ) ) ;
#951 = DIRECTION ( 'NONE',  ( 0.000000000000000000, 0.000000000000000000, 1.000000000000000000 ) ) ;
#952 = CARTESIAN_POINT ( 'NONE',  ( 108.0191169609971524, 18.28461070690599399, 4.532506661183012042 ) ) ;
#953 = CARTESIAN_POINT ( 'NONE',  ( -2.612550801365594477, -3.368539882008727115, -1.828967928396028064 ) ) ;
#954 = EDGE_LOOP ( 'NONE', ( #32362, #14583, #4659, #24433 ) ) ;
#955 = CARTESIAN_POINT ( 'NONE',  ( -6.550050800000000173, 0.9222479816126443186, 3.113457007523260156 ) ) ;
#956 = DIRECTION ( 'NONE',  ( 1.000000000000000000, -2.473959037481237219E-13, 0.000000000000000000 ) ) ;
#957 = FACE_OUTER_BOUND ( 'NONE', #10051, .T. ) ;
#958 = CARTESIAN_POINT ( 'NONE',  ( 8.996310305901880966, 0.3994363609773792789, 1.500000000000000000 ) ) ;
#959 = ORIENTED_EDGE ( 'NONE', *, *, #29979, .F. ) ;
#960 = CARTESIAN_POINT ( 'NONE',  ( 3.499999999999999556, 6.745408891279611296, -5.171987904998036178 ) ) ;
#961 = EDGE_LOOP ( 'NONE', ( #15262, #23988, #4017, #14320 ) ) ;
#962 = CARTESIAN_POINT ( 'NONE',  ( 3.920534810732780873, -12.31833506282117519, 1.757815050190617567 ) ) ;
#963 = COORDINATED_UNIVERSAL_TIME_OFFSET ( 0, 0, .AHEAD. ) ;
#964 = CARTESIAN_POINT ( 'NONE',  ( 18.79826502154066148, -5.432214915678442502, 4.312042181580753031 ) ) ;
#965 = CARTESIAN_POINT ( 'NONE',  ( 6.038144853276844692, -8.256557579931650181, -1.911563584435280072 ) ) ;
#966 = CARTESIAN_POINT ( 'NONE',  ( 24.12394826718414365, -17.31889127434044440, -1.369171926258704541 ) ) ;
#967 = CARTESIAN_POINT ( 'NONE',  ( 20.74999999999999645, 5.000000000000001776, 0.000000000000000000 ) ) ;
#968 = ORIENTED_EDGE ( 'NONE', *, *, #8596, .F. ) ;
#969 = EDGE_CURVE ( 'NONE', #6731, #481, #20377, .T. ) ;
#970 = CARTESIAN_POINT ( 'NONE',  ( 18.84751267742354841, -4.881724961800174789, 4.171847256157207084 ) ) ;
#971 = CARTESIAN_POINT ( 'NONE',  ( 0.08034252266819512378, 10.71005054582426830, -1.301095883299802525 ) ) ;
#972 = CARTESIAN_POINT ( 'NONE',  ( 21.04750000136559507, -1.913930629741527500, 2.363507492473149618 ) ) ;
#974 = VERTEX_POINT ( 'NONE', #18030 ) ;
#973 = CARTESIAN_POINT ( 'NONE',  ( 24.37017644007658390, -17.36705458136659175, -1.347230727354008728 ) ) ;
#975 = DIRECTION ( 'NONE',  ( 1.000000000000000000, -8.574039729943018344E-17, -0.000000000000000000 ) ) ;
#976 = ADVANCED_FACE ( 'NONE', ( #2153 ), #5166, .T. ) ;
#977 = CARTESIAN_POINT ( 'NONE',  ( 0.000000000000000000, 0.000000000000000000, 0.000000000000000000 ) ) ;
#978 = CARTESIAN_POINT ( 'NONE',  ( 69.10820754288535284, -6.866680491174807166, -2.787783121313799128 ) ) ;
#979 = VERTEX_POINT ( 'NONE', #25394 ) ;
#980 = ORIENTED_EDGE ( 'NONE', *, *, #20628, .T. ) ;
#981 = CARTESIAN_POINT ( 'NONE',  ( 3.063284526843251587, -3.174628368989204308, -8.152713396074016572 ) ) ;
#982 = CARTESIAN_POINT ( 'NONE',  ( 3.830085165118329002E-16, 4.467071865485494619, -1.625881193364653088 ) ) ;
#983 = LINE ( 'NONE', #25918, #18347 ) ;
#984 = CARTESIAN_POINT ( 'NONE',  ( -2.819379691724118508, -6.927609664242505794, 4.522129901861159595 ) ) ;
#985 = ADVANCED_FACE ( 'NONE', ( #2503, #22875 ), #33078, .T. ) ;
#986 = EDGE_CURVE ( 'NONE', #29104, #19214, #32052, .T. ) ;
#987 = DIRECTION ( 'NONE',  ( 1.000000000000000000, 0.000000000000000000, -0.000000000000000000 ) ) ;
#988 = CARTESIAN_POINT ( 'NONE',  ( -8.504531657079157370, 0.3127741368606810068, -2.975847129947406522 ) ) ;
#989 = CARTESIAN_POINT ( 'NONE',  ( -57.64511383230080810, -3.319689624912403048, 5.564001359196002916 ) ) ;
#990 = CARTESIAN_POINT ( 'NONE',  ( -4.687550801365594211, 2.228590825266444142, 2.752080473201636845 ) ) ;
#991 = DIRECTION ( 'NONE',  ( 8.541412920197217349E-17, 0.9961946980917454342, 0.08715574274765866547 ) ) ;
#992 = CARTESIAN_POINT ( 'NONE',  ( 47.94950013216585916, -7.827917879355857700, 2.184956529945685233 ) ) ;
#993 = VERTEX_POINT ( 'NONE', #30766 ) ;
#994 = CARTESIAN_POINT ( 'NONE',  ( 2.857987972556676137, -8.111531947321635627, -5.059832898186699346 ) ) ;
#995 = EDGE_CURVE ( 'NONE', #6245, #17057, #9237, .T. ) ;
#996 = ORIENTED_EDGE ( 'NONE', *, *, #11125, .F. ) ;
#997 = DATE_TIME_ROLE ( 'creation_date' ) ;
#998 = CARTESIAN_POINT ( 'NONE',  ( 102.4231258375787661, -3.997392187481084047, 3.997238528708670913 ) ) ;
#999 = ADVANCED_FACE ( 'NONE', ( #13492 ), #31556, .F. ) ;
#1000 = CARTESIAN_POINT ( 'NONE',  ( 24.26314457552869186, -17.18612746004505709, -0.9999999999999997780 ) ) ;
#1001 = ORIENTED_EDGE ( 'NONE', *, *, #5940, .F. ) ;
#1002 = CYLINDRICAL_SURFACE ( 'NONE', #151, 3.000000000000000444 ) ;
#1003 = ORIENTED_EDGE ( 'NONE', *, *, #5273, .T. ) ;
#1004 = ORIENTED_EDGE ( 'NONE', *, *, #10378, .T. ) ;
#1005 = CARTESIAN_POINT ( 'NONE',  ( 0.9232102171129938917, 0.000000000000000000, -4.522129901861164925 ) ) ;
#1006 = CARTESIAN_POINT ( 'NONE',  ( -3.162550801365593856, 2.752080473201636845, -2.228590825266444142 ) ) ;
#1007 = CARTESIAN_POINT ( 'NONE',  ( 19.06772426462030623, -16.20389337104299798, 1.500000000000000000 ) ) ;
#1008 = FACE_OUTER_BOUND ( 'NONE', #32534, .T. ) ;
#1010 = ORIENTED_EDGE ( 'NONE', *, *, #29590, .T. ) ;
#1009 = DIRECTION ( 'NONE',  ( 0.000000000000000000, -6.938893903907225222E-15, 1.000000000000000000 ) ) ;
#1011 = CARTESIAN_POINT ( 'NONE',  ( -6.837550801365593678, -3.675193018007246071, 1.088641768524163167 ) ) ;
#1012 = CARTESIAN_POINT ( 'NONE',  ( 9.547359219815096054, 1.400520851204822392, 1.500000000000000000 ) ) ;
#1013 = CARTESIAN_POINT ( 'NONE',  ( 0.000000000000000000, 5.904264776415100613, 2.046865518294726627 ) ) ;
#1014 = CARTESIAN_POINT ( 'NONE',  ( 21.67250000136559507, 2.363507492473148286, 1.913930629741525058 ) ) ;
#1015 = EDGE_CURVE ( 'NONE', #23179, #12214, #24823, .T. ) ;
#1017 = ORIENTED_EDGE ( 'NONE', *, *, #11179, .F. ) ;
#1016 = CARTESIAN_POINT ( 'NONE',  ( 0.000000000000000000, 0.000000000000000000, 0.000000000000000000 ) ) ;
#1018 = EDGE_CURVE ( 'NONE', #19569, #19561, #13314, .T. ) ;
#1019 = CARTESIAN_POINT ( 'NONE',  ( -29.35928501929439705, 7.719156497800170769, 2.044692901794244122 ) ) ;
#1020 = CARTESIAN_POINT ( 'NONE',  ( 21.54750000273118715, -0.7685399846772070775, 2.594547506269381465 ) ) ;
#1021 = EDGE_CURVE ( 'NONE', #6901, #10948, #8474, .T. ) ;
#1022 = EDGE_CURVE ( 'NONE', #31391, #30146, #21347, .T. ) ;
#1023 = CARTESIAN_POINT ( 'NONE',  ( -23.54713438637982748, 3.998227953278294944, 2.146185852361370383 ) ) ;
#1024 = DIRECTION ( 'NONE',  ( -0.000000000000000000, -0.000000000000000000, 1.000000000000000000 ) ) ;
#1025 = PLANE ( 'NONE',  #30600 ) ;
#1026 = CARTESIAN_POINT ( 'NONE',  ( 3.020080166740162664, -2.264483761671757467, 8.666653390676586355 ) ) ;
#1027 = DIRECTION ( 'NONE',  ( 0.000000000000000000, 0.2079116908177532919, 0.9781476007338069101 ) ) ;
#1028 = CARTESIAN_POINT ( 'NONE',  ( -5.187550801365593323, -3.521866450007987037, -0.3701630799359323931 ) ) ;
#1029 = VERTEX_POINT ( 'NONE', #2843 ) ;
#1030 = CARTESIAN_POINT ( 'NONE',  ( 7.064423600674403225, 8.466096581344354277, -2.210816291637329734 ) ) ;
#1032 = CARTESIAN_POINT ( 'NONE',  ( 7.249760686538667009, 0.000000000000000000, 0.000000000000000000 ) ) ;
#1031 = LINE ( 'NONE', #3560, #15028 ) ;
#1033 = ORIENTED_EDGE ( 'NONE', *, *, #16433, .F. ) ;
#1034 = EDGE_CURVE ( 'NONE', #3368, #31265, #2709, .T. ) ;
#1035 = AXIS2_PLACEMENT_3D ( 'NONE', #12260, #29838, #22470 ) ;
#1036 = PRODUCT_DEFINITION ( 'UNKNOWN', '', #17797, #7461 ) ;
#1037 = CARTESIAN_POINT ( 'NONE',  ( -57.40374817251313999, -2.616512360834426509, 5.949999999999999289 ) ) ;
#1038 = ORIENTED_EDGE ( 'NONE', *, *, #29832, .T. ) ;
#1039 = CARTESIAN_POINT ( 'NONE',  ( 25.75960661490314507, 24.76082900280850652, -0.4463807625373402699 ) ) ;
#1041 = ORIENTED_EDGE ( 'NONE', *, *, #12240, .F. ) ;
#1040 = DIRECTION ( 'NONE',  ( 0.000000000000000000, 0.000000000000000000, -1.000000000000000000 ) ) ;
#1042 = ORIENTED_EDGE ( 'NONE', *, *, #27738, .F. ) ;
#1043 = DIRECTION ( 'NONE',  ( 0.000000000000000000, 0.000000000000000000, 1.000000000000000000 ) ) ;
#1044 = DIRECTION ( 'NONE',  ( 1.000000000000000000, 0.000000000000000000, 0.000000000000000000 ) ) ;
#1046 = ORIENTED_EDGE ( 'NONE', *, *, #11544, .F. ) ;
#1045 = CARTESIAN_POINT ( 'NONE',  ( 10.57125986779756843, -0.8254815157535575487, 4.681538312723514395 ) ) ;
#1047 = CARTESIAN_POINT ( 'NONE',  ( -34.31843563627105453, 19.51744974835125035, -1.818740222761503045 ) ) ;
#1048 = DIRECTION ( 'NONE',  ( 0.07581065956227724112, 0.4221436659004729197, 0.9033534575330094407 ) ) ;
#1049 = CARTESIAN_POINT ( 'NONE',  ( 10.57125986779756843, -4.681538312723523276, 0.8254815157535098091 ) ) ;
#1050 = CARTESIAN_POINT ( 'NONE',  ( 11.72844750001322822, -13.05523934058288837, -1.000000000000000000 ) ) ;
#1051 = CARTESIAN_POINT ( 'NONE',  ( 107.4502834832519937, -17.36344364793921713, -4.530928846047229896 ) ) ;
#1052 = CARTESIAN_POINT ( 'NONE',  ( -4.850050802731186828, -2.331437884370912705, 1.887961173149512062 ) ) ;
#1053 = ADVANCED_FACE ( 'NONE', ( #20714 ), #9096, .T. ) ;
#1054 = CIRCLE ( 'NONE', #19739, 0.5000000000000003331 ) ;
#1055 = AXIS2_PLACEMENT_3D ( 'NONE', #15949, #19630, #27138 ) ;
#1056 = DIRECTION ( 'NONE',  ( -1.000000000000000000, -0.000000000000000000, -0.000000000000000000 ) ) ;
#1057 = CARTESIAN_POINT ( 'NONE',  ( 0.000000000000000000, 0.5174497483512452423, 0.000000000000000000 ) ) ;
#1058 = B_SPLINE_CURVE_WITH_KNOTS ( 'NONE', 3,
 ( #9443, #29853, #6935, #14138, #17134, #8946, #24338, #1450, #32034, #9104, #27343, #4464, #12281, #4950, #10454, #33029 ),
 .UNSPECIFIED., .F., .F.,
 ( 4, 2, 2, 2, 2, 2, 2, 4 ),
 ( 0.005048008663721728281, 0.006023483056901835289, 0.006511220253491893997, 0.006755088851786918147, 0.006877023150934431089, 0.006937990300508186693, 0.006968473875295064929, 0.006998957450081943164 ),
 .UNSPECIFIED. ) ;
#1059 = DIRECTION ( 'NONE',  ( -1.000000000000000000, 0.000000000000000000, -0.000000000000000000 ) ) ;
#1060 = CARTESIAN_POINT ( 'NONE',  ( 5.612718825656738630, 5.126902779943868893, -6.420171604529136822 ) ) ;
#1061 = AXIS2_PLACEMENT_3D ( 'NONE', #5420, #20648, #10437 ) ;
#1062 = ORIENTED_EDGE ( 'NONE', *, *, #23763, .F. ) ;
#1063 = DIRECTION ( 'NONE',  ( 0.000000000000000000, 0.000000000000000000, 1.000000000000000000 ) ) ;
#1064 = CARTESIAN_POINT ( 'NONE',  ( 17.33093461831347781, -21.43932300456618378, 1.500000000000000000 ) ) ;
#1065 = ORIENTED_EDGE ( 'NONE', *, *, #22651, .T. ) ;
#1066 = CARTESIAN_POINT ( 'NONE',  ( 25.28062539936192721, -0.8645097064285574007, 2.400641828158613489 ) ) ;
#1067 = CARTESIAN_POINT ( 'NONE',  ( 19.72835230534338891, -21.42792461751427169, 1.670332045613381222 ) ) ;
#1068 = ORIENTED_EDGE ( 'NONE', *, *, #31884, .F. ) ;
#1069 = CARTESIAN_POINT ( 'NONE',  ( 2.382865613620175349, 0.000000000000000000, 1.508259000770581615 ) ) ;
#1070 = DIRECTION ( 'NONE',  ( -0.3346727028291937578, 0.9423344321317153049, 1.601937360755264745E-18 ) ) ;
#1071 = ADVANCED_FACE ( 'NONE', ( #10502 ), #26054, .F. ) ;
#1072 = ORIENTED_EDGE ( 'NONE', *, *, #24945, .T. ) ;
#1073 = CIRCLE ( 'NONE', #24010, 12.00121908859764552 ) ;
#1074 = VECTOR ( 'NONE', #8549, 1000.000000000000000 ) ;
#1075 = EDGE_LOOP ( 'NONE', ( #18603, #16367, #22713, #25854, #6679 ) ) ;
#1076 = CARTESIAN_POINT ( 'NONE',  ( 25.52557118915443723, -17.56218954043521308, -1.000000000000000444 ) ) ;
#1077 = COORDINATED_UNIVERSAL_TIME_OFFSET ( 0, 0, .AHEAD. ) ;
#1079 = VERTEX_POINT ( 'NONE', #18857 ) ;
#1078 = DIRECTION ( 'NONE',  ( 0.000000000000000000, 0.9961946980917452121, 0.08715574274766220431 ) ) ;
#1080 = ORIENTED_EDGE ( 'NONE', *, *, #6143, .T. ) ;
#1081 = DIRECTION ( 'NONE',  ( -1.000000000000000000, 8.574039729943019576E-17, -6.162975822039154730E-33 ) ) ;
#1082 = VERTEX_POINT ( 'NONE', #29061 ) ;
#1084 = AXIS2_PLACEMENT_3D ( 'NONE', #25186, #12492, #22701 ) ;
#1083 = CARTESIAN_POINT ( 'NONE',  ( 11.04311965146447427, 15.00000000000002132, 1.508259000770581615 ) ) ;
#1085 = SHAPE_REPRESENTATION ( 'MAS-163', ( #22067, #26854, #25800, #11372, #1240, #5522, #25262, #32754, #15113 ), #24729 ) ;
#1086 = DIRECTION ( 'NONE',  ( -0.4999999999999978906, -0.8660254037844399289, 0.000000000000000000 ) ) ;
#1088 = ORIENTED_EDGE ( 'NONE', *, *, #4910, .T. ) ;
#1087 = DIRECTION ( 'NONE',  ( 0.000000000000000000, 0.9961946980917455452, -0.08715574274765797158 ) ) ;
#1089 = DIRECTION ( 'NONE',  ( -0.000000000000000000, -1.000000000000000000, -0.000000000000000000 ) ) ;
#1090 = DIRECTION ( 'NONE',  ( 0.000000000000000000, 0.000000000000000000, 1.000000000000000000 ) ) ;
#1091 = EDGE_CURVE ( 'NONE', #926, #21122, #3685, .T. ) ;
#1092 = DIRECTION ( 'NONE',  ( 1.387778780781445676E-14, -1.000000000000000000, -9.540979117872439019E-15 ) ) ;
#1093 = CARTESIAN_POINT ( 'NONE',  ( 4.749760686538667009, 7.892520144992453801, -1.391664247347147443 ) ) ;
#1094 = EDGE_CURVE ( 'NONE', #6248, #3262, #23369, .T. ) ;
#1095 = CARTESIAN_POINT ( 'NONE',  ( 108.0601430345486307, -18.93540685241356769, 4.558616106265892753 ) ) ;
#1096 = EDGE_CURVE ( 'NONE', #7166, #773, #22970, .T. ) ;
#1097 = CARTESIAN_POINT ( 'NONE',  ( -23.54713438637982748, 8.443947424854778561, 8.182767265444946148 ) ) ;
#1098 = DIRECTION ( 'NONE',  ( 0.000000000000000000, 0.000000000000000000, 1.000000000000000000 ) ) ;
#1099 = LINE ( 'NONE', #9089, #14117 ) ;
#1100 = AXIS2_PLACEMENT_3D ( 'NONE', #29549, #24495, #31890 ) ;
#1101 = AXIS2_PLACEMENT_3D ( 'NONE', #31790, #3547, #23907 ) ;
#1102 = CARTESIAN_POINT ( 'NONE',  ( 4.749760686538667009, -1.391664247347281780, 7.892520144992429820 ) ) ;
#1103 = CARTESIAN_POINT ( 'NONE',  ( 25.75999999999999801, -2.208672634433321348E-15, 0.000000000000000000 ) ) ;
#1104 = CARTESIAN_POINT ( 'NONE',  ( 108.1960732670207079, 19.26997324246909926, -4.614321361849296643 ) ) ;
#1105 = CARTESIAN_POINT ( 'NONE',  ( 24.00111451137534146, -6.623356326098185375E-16, -2.499999999999998224 ) ) ;
#1106 = AXIS2_PLACEMENT_3D ( 'NONE', #13582, #15922, #8262 ) ;
#1107 = LINE ( 'NONE', #18839, #22532 ) ;
#1108 = AXIS2_PLACEMENT_3D ( 'NONE', #17154, #27684, #24680 ) ;
#1109 = CARTESIAN_POINT ( 'NONE',  ( -2.562550801365592879, -2.228590825266444586, -2.752080473201636401 ) ) ;
#1110 = ORIENTED_EDGE ( 'NONE', *, *, #1444, .T. ) ;
#1111 = CARTESIAN_POINT ( 'NONE',  ( -6.000050800000000351, 2.331437884370912705, -1.887961173149511618 ) ) ;
#1112 = AXIS2_PLACEMENT_3D ( 'NONE', #18340, #28543, #26030 ) ;
#1113 = CARTESIAN_POINT ( 'NONE',  ( 108.1401284731860528, 18.95845055555492564, 5.012270609766838803 ) ) ;
#1114 = DIRECTION ( 'NONE',  ( 0.000000000000000000, 0.000000000000000000, 1.000000000000000000 ) ) ;
#1115 = CARTESIAN_POINT ( 'NONE',  ( 7.637044423814637994, -3.948987408041380487, 1.000000000000000000 ) ) ;
#1116 = ORIENTED_EDGE ( 'NONE', *, *, #29397, .F. ) ;
#1117 = CARTESIAN_POINT ( 'NONE',  ( 19.06772426461969516, -16.20389337104281680, -1.500000000000000666 ) ) ;
#1118 = EDGE_LOOP ( 'NONE', ( #5295, #20471, #21757 ) ) ;
#1119 = CARTESIAN_POINT ( 'NONE',  ( 0.5495841022003185028, -7.012970908023616445, 1.500000000000000000 ) ) ;
#1120 = PERSON_AND_ORGANIZATION ( #6766, #25292 ) ;
#1121 = CIRCLE ( 'NONE', #19809, 5.010000000000000675 ) ;
#1122 = CARTESIAN_POINT ( 'NONE',  ( 28.69034050020728799, -5.741730000312176507, 4.155404940063129438 ) ) ;
#1123 = VECTOR ( 'NONE', #33016, 1000.000000000000000 ) ;
#1124 = AXIS2_PLACEMENT_3D ( 'NONE', #32785, #9864, #25050 ) ;
#1125 = EDGE_CURVE ( 'NONE', #15674, #3548, #10832, .T. ) ;
#1126 = CARTESIAN_POINT ( 'NONE',  ( 3.063284526839887167, -8.734705317681623171, -0.4999240074895356933 ) ) ;
#1127 = AXIS2_PLACEMENT_3D ( 'NONE', #23045, #5329, #12525 ) ;
#1128 = CARTESIAN_POINT ( 'NONE',  ( 2.661997753583457360, -0.9074203448822719675, 10.09011512947412115 ) ) ;
#1129 = DIRECTION ( 'NONE',  ( 0.9842544651762055175, -0.1767573132311700268, 0.000000000000000000 ) ) ;
#1130 = VERTEX_POINT ( 'NONE', #1126 ) ;
#1131 = ADVANCED_FACE ( 'NONE', ( #26684 ), #13968, .T. ) ;
#1132 = EDGE_CURVE ( 'NONE', #7771, #5615, #12546, .T. ) ;
#1133 = DIRECTION ( 'NONE',  ( 0.000000000000000000, -1.000000000000000000, 0.000000000000000000 ) ) ;
#1134 = PLANE ( 'NONE',  #5432 ) ;
#1135 = LINE ( 'NONE', #32247, #28459 ) ;
#1136 = ADVANCED_FACE ( 'NONE', ( #32236 ), #24349, .T. ) ;
#1137 = CIRCLE ( 'NONE', #22467, 6.249000000000000554 ) ;
#1139 = VERTEX_POINT ( 'NONE', #9301 ) ;
#1138 = DIRECTION ( 'NONE',  ( -1.000000000000000000, 0.000000000000000000, 0.000000000000000000 ) ) ;
#1140 = CARTESIAN_POINT ( 'NONE',  ( 21.08401840680153327, -16.78474387323987926, -1.949999999999999512 ) ) ;
#1141 = DIRECTION ( 'NONE',  ( 0.000000000000000000, 0.000000000000000000, -1.000000000000000000 ) ) ;
#1142 = DIRECTION ( 'NONE',  ( -6.062761635205589313E-17, -0.7071067811865484609, -0.7071067811865465735 ) ) ;
#1143 = DIRECTION ( 'NONE',  ( 1.000000000000000000, 0.000000000000000000, 0.000000000000000000 ) ) ;
#1144 = FACE_OUTER_BOUND ( 'NONE', #1534, .T. ) ;
#1145 = DIRECTION ( 'NONE',  ( 1.000000000000000000, -0.000000000000000000, -0.000000000000000000 ) ) ;
#1146 = CARTESIAN_POINT ( 'NONE',  ( 6.399351475474185591, -16.64279405589157079, 5.485967528433935314 ) ) ;
#1147 = EDGE_LOOP ( 'NONE', ( #4926, #9709, #30639, #13226 ) ) ;
#1148 = AXIS2_PLACEMENT_3D ( 'NONE', #3104, #13259, #23460 ) ;
#1149 = CARTESIAN_POINT ( 'NONE',  ( 29.35001421184127324, -4.582605737176274729, 4.522129901861162260 ) ) ;
#1150 = ORIENTED_EDGE ( 'NONE', *, *, #13653, .F. ) ;
#1151 = VECTOR ( 'NONE', #9511, 1000.000000000000000 ) ;
#1152 = CIRCLE ( 'NONE', #10759, 0.4999999999999996669 ) ;
#1153 = CARTESIAN_POINT ( 'NONE',  ( 5.612718622971679672, 2.621884781721373070, -7.786491723834085832 ) ) ;
#1154 = DIRECTION ( 'NONE',  ( 1.000000000000000000, -0.000000000000000000, -0.000000000000000000 ) ) ;
#1155 = AXIS2_PLACEMENT_3D ( 'NONE', #16083, #31977, #19263 ) ;
#1156 = CARTESIAN_POINT ( 'NONE',  ( -3.387550801365593056, 0.3701630799359330593, -3.521866450007987037 ) ) ;
#1157 = DIRECTION ( 'NONE',  ( -1.000000000000000000, 0.000000000000000000, 0.000000000000000000 ) ) ;
#1158 = CARTESIAN_POINT ( 'NONE',  ( 18.65791233782715963, -7.001076235476726417, 2.184956778830005941 ) ) ;
#1159 = VERTEX_POINT ( 'NONE', #3799 ) ;
#1160 = DIRECTION ( 'NONE',  ( 1.000000000000000000, -0.000000000000000000, 0.000000000000000000 ) ) ;
#1161 = AXIS2_PLACEMENT_3D ( 'NONE', #25032, #16900, #27564 ) ;
#1163 = ADVANCED_FACE ( 'NONE', ( #24677 ), #6449, .T. ) ;
#1162 = ORIENTED_EDGE ( 'NONE', *, *, #10095, .F. ) ;
#1164 = APPROVAL_DATE_TIME ( #8681, #17193 ) ;
#1165 = CARTESIAN_POINT ( 'NONE',  ( 40.88399151329760883, -6.896594116963963295, 3.993433839888539172 ) ) ;
#1166 = EDGE_CURVE ( 'NONE', #27059, #7057, #19779, .T. ) ;
#1167 = DIRECTION ( 'NONE',  ( 0.000000000000000000, 0.000000000000000000, 1.000000000000000000 ) ) ;
#1168 = ORIENTED_EDGE ( 'NONE', *, *, #30070, .F. ) ;
#1169 = CARTESIAN_POINT ( 'NONE',  ( -3.222375984151267581, 0.000000000000000000, -1.000000000000000000 ) ) ;
#1170 = ORIENTED_EDGE ( 'NONE', *, *, #25908, .F. ) ;
#1171 = ORIENTED_EDGE ( 'NONE', *, *, #17491, .T. ) ;
#1172 = EDGE_CURVE ( 'NONE', #10298, #5929, #13617, .T. ) ;
#1173 = CARTESIAN_POINT ( 'NONE',  ( 3.249999999999999556, -8.152713396088739017, -3.174628368996162298 ) ) ;
#1174 = CARTESIAN_POINT ( 'NONE',  ( -4.062550801365593323, 0.3701630799359330593, -3.521866450007987037 ) ) ;
#1175 = AXIS2_PLACEMENT_3D ( 'NONE', #26703, #3817, #13994 ) ;
#1176 = CARTESIAN_POINT ( 'NONE',  ( 22.29750000000000654, -0.7685399846772070775, 2.594547506269381465 ) ) ;
#1177 = LINE ( 'NONE', #26260, #11840 ) ;
#1179 = ORIENTED_EDGE ( 'NONE', *, *, #17111, .F. ) ;
#1178 = DIRECTION ( 'NONE',  ( 0.000000000000000000, 0.000000000000000000, 1.000000000000000000 ) ) ;
#1180 = CARTESIAN_POINT ( 'NONE',  ( -5.387550801365593500, -0.3701630799359326152, 3.521866450007987037 ) ) ;
#1181 = AXIS2_PLACEMENT_3D ( 'NONE', #22571, #24901, #7342 ) ;
#1182 = CARTESIAN_POINT ( 'NONE',  ( 14.99916604752485583, 9.584522669699346409, 1.050000000000000044 ) ) ;
#1183 = EDGE_CURVE ( 'NONE', #26824, #12879, #7478, .T. ) ;
#1184 = CARTESIAN_POINT ( 'NONE',  ( 10.25014922901193692, -19.98138187138910737, 1.499999999999999112 ) ) ;
#1185 = CARTESIAN_POINT ( 'NONE',  ( -23.54713438637982748, 6.487496165429137207, 7.419273015635701185 ) ) ;
#1186 = CIRCLE ( 'NONE', #32696, 0.5000000000000000000 ) ;
#1187 = ORIENTED_EDGE ( 'NONE', *, *, #25876, .F. ) ;
#1188 = AXIS2_PLACEMENT_3D ( 'NONE', #13728, #6065, #26611 ) ;
#1189 = CIRCLE ( 'NONE', #5468, 8.749000000000002331 ) ;
#1190 = CARTESIAN_POINT ( 'NONE',  ( 22.98500000273118715, -0.2613211581691358698, -2.486304738420681559 ) ) ;
#1191 = EDGE_CURVE ( 'NONE', #17091, #14136, #16829, .T. ) ;
#1192 = CARTESIAN_POINT ( 'NONE',  ( 5.489321486716459475, -1.307389195612923327, -8.012877392144808653 ) ) ;
#1193 = ADVANCED_FACE ( 'NONE', ( #11322 ), #21529, .F. ) ;
#1194 = CARTESIAN_POINT ( 'NONE',  ( 18.71626227658832065, -6.348841026559134626, -3.236291062301399180 ) ) ;
#1195 = CARTESIAN_POINT ( 'NONE',  ( -4.147447373149248051, -6.154642429219350674, -1.745243162019930239 ) ) ;
#1196 = CIRCLE ( 'NONE', #734, 8.749000000000002331 ) ;
#1197 = CARTESIAN_POINT ( 'NONE',  ( 0.6791199890552930274, -5.814932665552347224, -7.071625480714448742 ) ) ;
#1198 = AXIS2_PLACEMENT_3D ( 'NONE', #27477, #14755, #22445 ) ;
#1199 = VECTOR ( 'NONE', #21108, 1000.000000000000114 ) ;
#1200 = DIRECTION ( 'NONE',  ( 0.000000000000000000, 0.000000000000000000, -1.000000000000000000 ) ) ;
#1201 = LINE ( 'NONE', #11398, #24197 ) ;
#1202 = VERTEX_POINT ( 'NONE', #25175 ) ;
#1203 = ADVANCED_FACE ( 'NONE', ( #17151 ), #4968, .T. ) ;
#1204 = AXIS2_PLACEMENT_3D ( 'NONE', #2043, #27104, #27457 ) ;
#1205 = CIRCLE ( 'NONE', #12962, 11.00000000000000000 ) ;
#1206 = CIRCLE ( 'NONE', #5996, 0.4500000000000000111 ) ;
#1207 = CARTESIAN_POINT ( 'NONE',  ( 20.72551590764672724, -21.66366526924204194, 1.459983613673395908 ) ) ;
#1208 = CARTESIAN_POINT ( 'NONE',  ( 7.249760686538667009, -8.721381771256204729, 0.7071067811865423547 ) ) ;
#1211 = LINE ( 'NONE', #11221, #18226 ) ;
#1210 = FACE_OUTER_BOUND ( 'NONE', #15996, .T. ) ;
#1209 = AXIS2_PLACEMENT_3D ( 'NONE', #24034, #13190, #3670 ) ;
#1212 = EDGE_LOOP ( 'NONE', ( #12042, #3122, #11676, #30079, #26435, #23259 ) ) ;
#1213 = AXIS2_PLACEMENT_3D ( 'NONE', #32282, #22223, #21875 ) ;
#1214 = DIRECTION ( 'NONE',  ( 0.000000000000000000, 0.2588190451025258465, -0.9659258262890669799 ) ) ;
#1215 = ORIENTED_EDGE ( 'NONE', *, *, #29793, .F. ) ;
#1216 = DIRECTION ( 'NONE',  ( -0.000000000000000000, 0.000000000000000000, 1.000000000000000000 ) ) ;
#1218 = ORIENTED_EDGE ( 'NONE', *, *, #23365, .T. ) ;
#1217 = CARTESIAN_POINT ( 'NONE',  ( 40.87773744809802423, -5.749688186340451423, -3.995006151633446745 ) ) ;
#1219 = EDGE_LOOP ( 'NONE', ( #4424, #27223, #30890, #20774 ) ) ;
#1220 = CARTESIAN_POINT ( 'NONE',  ( 28.63490450844110313, -5.610497434542901729, 3.993434336046763899 ) ) ;
#1221 = EDGE_CURVE ( 'NONE', #24949, #4203, #9804, .T. ) ;
#1222 = EDGE_CURVE ( 'NONE', #24417, #4009, #22338, .T. ) ;
#1223 = DIRECTION ( 'NONE',  ( 0.000000000000000000, 0.9063077870366480493, 0.4226182617407034936 ) ) ;
#1225 = VERTEX_POINT ( 'NONE', #27681 ) ;
#1224 = CARTESIAN_POINT ( 'NONE',  ( 107.7536796087345294, 16.80655079293032017, 1.395761063491601783 ) ) ;
#1226 = AXIS2_PLACEMENT_3D ( 'NONE', #16802, #13622, #16447 ) ;
#1227 = CARTESIAN_POINT ( 'NONE',  ( 15.90893862159966865, 10.93205754344057645, -1.500000000000296208 ) ) ;
#1228 = CARTESIAN_POINT ( 'NONE',  ( -2.940577200613229358, -11.38371329336536242, -1.743664497973003158 ) ) ;
#1229 = VECTOR ( 'NONE', #241, 1000.000000000000227 ) ;
#1230 = CARTESIAN_POINT ( 'NONE',  ( -1.075551320669168476, 0.000000000000000000, 7.404527507138929820 ) ) ;
#1231 = CIRCLE ( 'NONE', #29003, 3.499999999999999556 ) ;
#1232 = CARTESIAN_POINT ( 'NONE',  ( 6.669411210323004546, -6.378078458904371750, -1.500000000000000000 ) ) ;
#1233 = ADVANCED_FACE ( 'NONE', ( #7292 ), #2295, .T. ) ;
#1234 = CARTESIAN_POINT ( 'NONE',  ( 10.00000000000000178, -8.574039729943018837E-16, 0.000000000000000000 ) ) ;
#1235 = CARTESIAN_POINT ( 'NONE',  ( 25.75999999999999801, -2.208672634433321348E-15, 0.000000000000000000 ) ) ;
#1236 = CIRCLE ( 'NONE', #3911, 6.000000000000001776 ) ;
#1237 = AXIS2_PLACEMENT_3D ( 'NONE', #23594, #717, #31311 ) ;
#1238 = DIRECTION ( 'NONE',  ( 1.000000000000000000, 0.000000000000000000, 0.000000000000000000 ) ) ;
#1239 = LINE ( 'NONE', #3914, #23234 ) ;
#1240 = AXIS2_PLACEMENT_3D ( 'NONE', #2034, #30138, #3596 ) ;
#1241 = AXIS2_PLACEMENT_3D ( 'NONE', #14417, #22656, #19987 ) ;
#1242 = EDGE_CURVE ( 'NONE', #5714, #20158, #30051, .T. ) ;
#1243 = DIRECTION ( 'NONE',  ( -0.000000000000000000, 0.000000000000000000, 1.000000000000000000 ) ) ;
#1244 = DIRECTION ( 'NONE',  ( -1.000000000000000000, 8.574039729943017111E-17, -0.000000000000000000 ) ) ;
#1245 = VERTEX_POINT ( 'NONE', #22508 ) ;
#1246 = LINE ( 'NONE', #4223, #24696 ) ;
#1247 = CARTESIAN_POINT ( 'NONE',  ( 3.249999999999999556, 0.000000000000000000, 0.000000000000000000 ) ) ;
#1248 = DIRECTION ( 'NONE',  ( 0.000000000000000000, -0.000000000000000000, -1.000000000000000000 ) ) ;
#1249 = ORIENTED_EDGE ( 'NONE', *, *, #27778, .T. ) ;
#1250 = AXIS2_PLACEMENT_3D ( 'NONE', #22194, #22345, #9624 ) ;
#1251 = VECTOR ( 'NONE', #20562, 1000.000000000000000 ) ;
#1252 = VECTOR ( 'NONE', #5654, 1000.000000000000114 ) ;
#1253 = CARTESIAN_POINT ( 'NONE',  ( 2.274274201625317460, -7.593217523260661572, 7.958834565716747633 ) ) ;
#1254 = CARTESIAN_POINT ( 'NONE',  ( 46.69789307159569347, 25.15383447853596621, -4.612695725900423760 ) ) ;
#1256 = EDGE_LOOP ( 'NONE', ( #24092, #9756, #31064, #7718 ) ) ;
#1255 = AXIS2_PLACEMENT_3D ( 'NONE', #25344, #25158, #23173 ) ;
#1257 = DIRECTION ( 'NONE',  ( -0.4030398059120889331, -0.9151824489413822317, 5.627812144739313658E-15 ) ) ;
#1258 = EDGE_CURVE ( 'NONE', #3790, #6345, #12784, .T. ) ;
#1259 = ORIENTED_EDGE ( 'NONE', *, *, #3631, .T. ) ;
#1260 = VECTOR ( 'NONE', #196, 1000.000000000000000 ) ;
#1261 = CIRCLE ( 'NONE', #32770, 0.4999999999999996114 ) ;
#1262 = EDGE_LOOP ( 'NONE', ( #12802, #23937, #26982, #20183, #3533, #31501, #28149, #28824, #16780, #16189, #11355, #27700, #28821, #16218, #927, #7872, #1965, #25359, #24449, #23284, #21082, #17252, #5551, #18711, #17175, #19865, #30878, #30833, #4783, #9452, #31844, #12473, #26550, #4502, #24505, #3026, #15582, #10297, #29237, #12506, #28495, #6404, #4976, #14184, #212, #14762 ) ) ;
#1263 = CARTESIAN_POINT ( 'NONE',  ( 24.57728726453494517, -17.46986644506281650, -1.411007141442706114 ) ) ;
#1264 = APPROVAL_ROLE ( '' ) ;
#1265 = VECTOR ( 'NONE', #16366, 1000.000000000000000 ) ;
#1267 = ORIENTED_EDGE ( 'NONE', *, *, #12098, .T. ) ;
#1266 = CYLINDRICAL_SURFACE ( 'NONE', #8001, 4.000000000000001776 ) ;
#1268 = VERTEX_POINT ( 'NONE', #27361 ) ;
#1269 = CARTESIAN_POINT ( 'NONE',  ( -38.14293509397969473, 10.97000000000000419, -1.500000000000000000 ) ) ;
#1270 = ADVANCED_FACE ( 'NONE', ( #12481 ), #5885, .F. ) ;
#1271 = LOCAL_TIME ( 16, 7, 10.00000000000000000, #6324 ) ;
#1272 = ORIENTED_EDGE ( 'NONE', *, *, #3151, .T. ) ;
#1273 = CARTESIAN_POINT ( 'NONE',  ( 6.448894291894883501, -17.04229596238074507, 4.522129901861158707 ) ) ;
#1274 = CARTESIAN_POINT ( 'NONE',  ( 3.499999999999999556, -1.179494851233943598, 6.136676046192483192 ) ) ;
#1276 = ORIENTED_EDGE ( 'NONE', *, *, #32465, .F. ) ;
#1275 = CARTESIAN_POINT ( 'NONE',  ( 19.01480233880980819, -3.011762293215292097, -0.4367666033480814836 ) ) ;
#1277 = DIRECTION ( 'NONE',  ( -1.000000000000000000, 0.000000000000000000, 0.000000000000000000 ) ) ;
#1278 = LINE ( 'NONE', #19135, #8517 ) ;
#1279 = CARTESIAN_POINT ( 'NONE',  ( 4.749760686538667009, -6.139290821770219786, -5.151476664237539360 ) ) ;
#1280 = DIRECTION ( 'NONE',  ( 0.000000000000000000, -0.5735764363510533759, 0.8191520442889866915 ) ) ;
#1281 = CARTESIAN_POINT ( 'NONE',  ( 108.0612880515141683, -18.95189481187503588, 4.515510177595837504 ) ) ;
#1282 = VECTOR ( 'NONE', #23000, 1000.000000000000114 ) ;
#1283 = CARTESIAN_POINT ( 'NONE',  ( 42.88108885377458535, -22.62752020922543750, -4.522129901861166701 ) ) ;
#1284 = DIRECTION ( 'NONE',  ( -1.000000000000000000, 8.574039729943017111E-17, -0.000000000000000000 ) ) ;
#1285 = DIRECTION ( 'NONE',  ( -0.000000000000000000, -0.000000000000000000, 1.000000000000000000 ) ) ;
#1286 = AXIS2_PLACEMENT_3D ( 'NONE', #12622, #17627, #4771 ) ;
#1287 = CIRCLE ( 'NONE', #6071, 5.010000000000000675 ) ;
#1288 = EDGE_CURVE ( 'NONE', #10646, #9547, #31984, .T. ) ;
#1289 = CARTESIAN_POINT ( 'NONE',  ( 0.000000000000000000, 18.00000000000000355, -3.750000000000000444 ) ) ;
#1290 = CARTESIAN_POINT ( 'NONE',  ( 109.7266016284591927, 16.47760998941501143, 5.471072653610988823 ) ) ;
#1291 = LINE ( 'NONE', #17427, #17757 ) ;
#1292 = LINE ( 'NONE', #14279, #2260 ) ;
#1293 = PRODUCT_DEFINITION_FORMATION_WITH_SPECIFIED_SOURCE ( 'ANY', '', #30333, .NOT_KNOWN. ) ;
#1294 = CARTESIAN_POINT ( 'NONE',  ( 32.99878091140234915, 0.000000000000000000, 0.9987809114025785195 ) ) ;
#1295 = CARTESIAN_POINT ( 'NONE',  ( -6.800050802731187893, 3.113457007523260156, -0.9222479816126439855 ) ) ;
#1296 = EDGE_LOOP ( 'NONE', ( #7344, #2499, #27989 ) ) ;
#1297 = CARTESIAN_POINT ( 'NONE',  ( -7.250050800000000351, -1.549418761218565477, 2.853674364686380471 ) ) ;
#1298 = B_SPLINE_CURVE_WITH_KNOTS ( 'NONE', 3,
 ( #27614, #12390, #32820, #25088, #2392, #27763, #4877, #15058 ),
 .UNSPECIFIED., .F., .F.,
 ( 4, 2, 2, 4 ),
 ( 5.099451029798333178E-07, 0.001229189835658059133, 0.001843529780935598741, 0.002457869726213138782 ),
 .UNSPECIFIED. ) ;
#1299 = CARTESIAN_POINT ( 'NONE',  ( 9.149098621172166546, 18.06225657836807841, -4.612695725900421984 ) ) ;
#1300 = CYLINDRICAL_SURFACE ( 'NONE', #11941, 0.5000000000000007772 ) ;
#1301 = CARTESIAN_POINT ( 'NONE',  ( -41.58734146630091999, -15.56207840271351728, 5.312698343317051375 ) ) ;
#1302 = VERTEX_POINT ( 'NONE', #30546 ) ;
#1303 = CARTESIAN_POINT ( 'NONE',  ( -17.45597128428593336, -28.43932300454937590, 11.00000000000000000 ) ) ;
#1304 = EDGE_CURVE ( 'NONE', #7488, #29208, #32077, .T. ) ;
#1305 =( BOUNDED_SURFACE ( )  B_SPLINE_SURFACE ( 3, 2, ( 
 ( #24739, #12041, #29607 ),
 ( #17027, #27233, #4350 ),
 ( #11383, #4530, #8343 ),
 ( #665, #23875, #13513 ) ),
 .UNSPECIFIED., .F., .F., .F. ) 
 B_SPLINE_SURFACE_WITH_KNOTS ( ( 4, 4 ),
 ( 3, 3 ),
 ( 0.003700663664647922940, 0.007131426728608055571 ),
 ( 0.000000000000000000, 1.000000000000000000 ),
 .UNSPECIFIED. ) 
 GEOMETRIC_REPRESENTATION_ITEM ( )  RATIONAL_B_SPLINE_SURFACE ( (
 ( 1.000000000000000000, 0.7067603058644310599, 1.000000000000000000),
 ( 1.000000000000000000, 0.7067606020011648615, 1.000000000000000000),
 ( 1.000000000000000000, 0.7067612639882160375, 1.000000000000000000),
 ( 1.000000000000000000, 0.7067623105831786212, 1.000000000000000000) ) ) 
 REPRESENTATION_ITEM ( '' )  SURFACE ( )  );
#1306 = VECTOR ( 'NONE', #15568, 1000.000000000000000 ) ;
#1307 = ORIENTED_EDGE ( 'NONE', *, *, #26956, .T. ) ;
#1308 = CARTESIAN_POINT ( 'NONE',  ( 1.872983491663670286, -10.12226979866639809, 1.499999999999999556 ) ) ;
#1309 = EDGE_CURVE ( 'NONE', #8686, #389, #31550, .T. ) ;
#1310 = PERSON_AND_ORGANIZATION ( #6766, #25292 ) ;
#1311 = ORIENTED_EDGE ( 'NONE', *, *, #30645, .F. ) ;
#1312 = CARTESIAN_POINT ( 'NONE',  ( 18.82056267271149252, -5.182971926439480015, 4.312042181588143563 ) ) ;
#1313 = DIRECTION ( 'NONE',  ( 0.000000000000000000, 1.000000000000000000, 0.000000000000000000 ) ) ;
#1314 = CARTESIAN_POINT ( 'NONE',  ( 84.99303864846685030, -4.506833362023316525, -4.312042181581901445 ) ) ;
#1315 = CARTESIAN_POINT ( 'NONE',  ( 2.274274201625309910, -1.464956435139646462, 10.90201369670501386 ) ) ;
#1316 = LINE ( 'NONE', #8818, #3838 ) ;
#1317 = ORIENTED_EDGE ( 'NONE', *, *, #12569, .T. ) ;
#1318 = ORGANIZATION ( 'NAUO-ORG3', 'UNSPECIFIED', 'UNSPECIFIED' ) ;
#1319 = DIRECTION ( 'NONE',  ( -1.000000000000000000, 0.000000000000000000, 0.000000000000000000 ) ) ;
#1320 = DIRECTION ( 'NONE',  ( 0.000000000000000000, 0.000000000000000000, 1.000000000000000000 ) ) ;
#1321 = LINE ( 'NONE', #8648, #27925 ) ;
#1323 = ORIENTED_EDGE ( 'NONE', *, *, #22495, .F. ) ;
#1322 = DIRECTION ( 'NONE',  ( -0.000000000000000000, 0.9659258262890693114, -0.2588190451025172978 ) ) ;
#1324 = CARTESIAN_POINT ( 'NONE',  ( -3.662550801365593411, -0.3701630799359326152, 3.521866450007987037 ) ) ;
#1325 = CARTESIAN_POINT ( 'NONE',  ( 47.98568197278775216, -2.821418575600922019, -0.07017451552781628354 ) ) ;
#1326 = DIRECTION ( 'NONE',  ( 1.000000000000000000, 0.000000000000000000, 0.000000000000000000 ) ) ;
#1327 = CARTESIAN_POINT ( 'NONE',  ( 108.5619817448483531, 15.65002148400675530, 0.7764623223310612721 ) ) ;
#1328 = DIRECTION ( 'NONE',  ( 0.000000000000000000, -0.2588190451025167982, -0.9659258262890694224 ) ) ;
#1329 = CARTESIAN_POINT ( 'NONE',  ( 0.000000000000000000, 0.000000000000000000, 0.000000000000000000 ) ) ;
#1330 = CIRCLE ( 'NONE', #28556, 0.5000000000000004441 ) ;
#1331 = CARTESIAN_POINT ( 'NONE',  ( -9.288857950784214168, 18.90773822806172433, 1.500000000000000222 ) ) ;
#1332 = PLANE ( 'NONE',  #680 ) ;
#1333 = CARTESIAN_POINT ( 'NONE',  ( -2.092582746845476738, -9.051626392537004406, 5.485967528433935314 ) ) ;
#1334 = ORIENTED_EDGE ( 'NONE', *, *, #10499, .T. ) ;
#1335 = CARTESIAN_POINT ( 'NONE',  ( -2.650050802731187094, 1.887961173149511618, 2.331437884370912705 ) ) ;
#1336 = ORIENTED_EDGE ( 'NONE', *, *, #31481, .F. ) ;
#1337 = CARTESIAN_POINT ( 'NONE',  ( 10.00000000000000000, 3.407865132560179422, 3.672404558090050397 ) ) ;
#1338 = CARTESIAN_POINT ( 'NONE',  ( -1.963030064606874792, 0.7837004005683814167, 3.199079356508811145 ) ) ;
#1339 = CARTESIAN_POINT ( 'NONE',  ( -2.287550801365593856, 2.228590825266444142, 2.752080473201636845 ) ) ;
#1340 = DIRECTION ( 'NONE',  ( 0.000000000000000000, 0.9961946980917459893, -0.08715574274765383600 ) ) ;
#1341 = CARTESIAN_POINT ( 'NONE',  ( 3.499999999999999556, 0.000000000000000000, 0.000000000000000000 ) ) ;
#1342 = ORIENTED_EDGE ( 'NONE', *, *, #8382, .F. ) ;
#1343 = EDGE_CURVE ( 'NONE', #5341, #24378, #12322, .T. ) ;
#1344 = CARTESIAN_POINT ( 'NONE',  ( 107.4385791398478602, 17.85938043952733878, -4.612695725900422872 ) ) ;
#1345 = EDGE_CURVE ( 'NONE', #25797, #24410, #6056, .T. ) ;
#1346 = VERTEX_POINT ( 'NONE', #30372 ) ;
#1347 = PERSON_AND_ORGANIZATION ( #6766, #25292 ) ;
#1348 = CARTESIAN_POINT ( 'NONE',  ( 69.07041625887113412, -6.115693503127433317, 3.994703126862036324 ) ) ;
#1349 = CARTESIAN_POINT ( 'NONE',  ( -3.650050802731187094, 2.331437884370912705, -1.887961173149511618 ) ) ;
#1350 = ORIENTED_EDGE ( 'NONE', *, *, #10220, .T. ) ;
#1351 = FACE_OUTER_BOUND ( 'NONE', #7864, .T. ) ;
#1352 = VERTEX_POINT ( 'NONE', #28035 ) ;
#1353 = ORIENTED_EDGE ( 'NONE', *, *, #11804, .F. ) ;
#1354 = DIRECTION ( 'NONE',  ( 1.000000000000000000, -0.000000000000000000, -0.000000000000000000 ) ) ;
#1355 = CARTESIAN_POINT ( 'NONE',  ( -4.562550801365594211, 2.228590825266444142, 2.752080473201636845 ) ) ;
#1356 = CARTESIAN_POINT ( 'NONE',  ( 23.11000000000000298, 1.942864903642424146, 1.573300977624592534 ) ) ;
#1357 = LINE ( 'NONE', #11377, #17711 ) ;
#1359 = VERTEX_POINT ( 'NONE', #2467 ) ;
#1358 = DIRECTION ( 'NONE',  ( -1.000000000000000000, -0.000000000000000000, -0.000000000000000000 ) ) ;
#1360 = CARTESIAN_POINT ( 'NONE',  ( -6.537550801365592967, 1.828967928396027176, -3.368539882008727115 ) ) ;
#1361 = CARTESIAN_POINT ( 'NONE',  ( 107.7872089731491485, 16.99325552404635076, -1.779390171460584646 ) ) ;
#1362 = B_SPLINE_CURVE_WITH_KNOTS ( 'NONE', 3,
 ( #14293, #17144, #27357, #26860, #4472, #14648, #3977, #21831, #32042, #9112 ),
 .UNSPECIFIED., .F., .F.,
 ( 4, 2, 2, 2, 4 ),
 ( 2.493548413911061648E-07, 0.0005478513795029414657, 0.001095453404164491943, 0.001643055428826042203, 0.002190657453487592464 ),
 .UNSPECIFIED. ) ;
#1363 = CARTESIAN_POINT ( 'NONE',  ( 6.883866482134012088, 2.190971798910059221, -8.452201317944583181 ) ) ;
#1364 = CARTESIAN_POINT ( 'NONE',  ( -14.62340757463330654, -21.93932300455827900, -1.000000000000000000 ) ) ;
#1365 = EDGE_LOOP ( 'NONE', ( #10471, #2774, #2252, #29150 ) ) ;
#1367 = ORIENTED_EDGE ( 'NONE', *, *, #3302, .F. ) ;
#1366 = CARTESIAN_POINT ( 'NONE',  ( 5.377543748152549874, -6.940565734314570356, -4.007137495034885255 ) ) ;
#1368 = CARTESIAN_POINT ( 'NONE',  ( 20.48500000273118715, 0.2613211581691317065, 2.486304738420681559 ) ) ;
#1369 = CARTESIAN_POINT ( 'NONE',  ( 25.47590243882417482, -17.55751406896973421, 1.147657757683672619 ) ) ;
#1370 = CARTESIAN_POINT ( 'NONE',  ( -29.77647832281567020, 15.08866638674292027, 1.500000000000000000 ) ) ;
#1371 = FACE_OUTER_BOUND ( 'NONE', #4290, .T. ) ;
#1372 = EDGE_CURVE ( 'NONE', #22295, #31644, #32843, .T. ) ;
#1373 = CARTESIAN_POINT ( 'NONE',  ( -54.10469650629801919, 5.263418255572274163, 1.500000000000000000 ) ) ;
#1374 = CARTESIAN_POINT ( 'NONE',  ( 9.286398372032465431, 0.2229077781794372437, 1.044673861545039051 ) ) ;
#1375 = CARTESIAN_POINT ( 'NONE',  ( -3.487550801365593589, -2.228590825266444586, -2.752080473201636401 ) ) ;
#1376 = DIRECTION ( 'NONE',  ( -3.469446951953478110E-15, 0.000000000000000000, 1.000000000000000000 ) ) ;
#1377 = EDGE_LOOP ( 'NONE', ( #9486, #23820, #28856 ) ) ;
#1378 = CYLINDRICAL_SURFACE ( 'NONE', #9161, 6.248999999999999666 ) ;
#1379 = EDGE_CURVE ( 'NONE', #9138, #16840, #2521, .T. ) ;
#1380 = CARTESIAN_POINT ( 'NONE',  ( 2.440333653308764728, 9.715096239907470732, -4.424884217119326557 ) ) ;
#1382 = CARTESIAN_POINT ( 'NONE',  ( 3.063284526843530031, -4.729683950890320787, 7.360373001715534436 ) ) ;
#1381 = CARTESIAN_POINT ( 'NONE',  ( 1.750000000000000222, 1.106368468154430129, 8.427689411260576691 ) ) ;
#1383 = ORIENTED_EDGE ( 'NONE', *, *, #30707, .F. ) ;
#1384 = CARTESIAN_POINT ( 'NONE',  ( -2.037945749704288773E-16, -2.376879293651036118, -4.116875700062107235 ) ) ;
#1385 = ORIENTED_EDGE ( 'NONE', *, *, #4688, .F. ) ;
#1386 = FACE_OUTER_BOUND ( 'NONE', #22890, .T. ) ;
#1388 = ORIENTED_EDGE ( 'NONE', *, *, #12943, .F. ) ;
#1387 = CARTESIAN_POINT ( 'NONE',  ( 84.96562648226598924, -4.059759578883751274, -3.994701829040198326 ) ) ;
#1389 = EDGE_CURVE ( 'NONE', #29167, #30955, #26209, .T. ) ;
#1390 = ORIENTED_EDGE ( 'NONE', *, *, #4252, .F. ) ;
#1391 = CARTESIAN_POINT ( 'NONE',  ( 107.6641398346956890, -20.45810202417174750, -1.499999999999999556 ) ) ;
#1393 = ORIENTED_EDGE ( 'NONE', *, *, #16236, .F. ) ;
#1392 = CARTESIAN_POINT ( 'NONE',  ( 107.3753443242040362, -16.28466752050562505, 2.316915192227371190 ) ) ;
#1394 = FACE_OUTER_BOUND ( 'NONE', #1540, .T. ) ;
#1395 = CARTESIAN_POINT ( 'NONE',  ( 9.031711214211194161, 0.01997115109544311817, -1.016156546702293051 ) ) ;
#1396 = EDGE_CURVE ( 'NONE', #7526, #14757, #6774, .T. ) ;
#1397 = CARTESIAN_POINT ( 'NONE',  ( 0.000000000000000000, -6.478011392632939902, 6.807171995660557862 ) ) ;
#1398 = CARTESIAN_POINT ( 'NONE',  ( 13.25896750271661517, -14.28336940137728739, -1.500000000000000000 ) ) ;
#1400 = ORIENTED_EDGE ( 'NONE', *, *, #13463, .F. ) ;
#1399 = CARTESIAN_POINT ( 'NONE',  ( 108.0017345319158295, -18.09433894470946314, -4.637781146201932714 ) ) ;
#1401 = DIRECTION ( 'NONE',  ( -0.9896144216807899463, 0.000000000000000000, -0.1437473352845038410 ) ) ;
#1402 = EDGE_CURVE ( 'NONE', #16153, #8879, #12841, .T. ) ;
#1403 = CARTESIAN_POINT ( 'NONE',  ( 0.000000000000000000, -10.82112760146737429, 1.975651141462198890 ) ) ;
#1404 = LINE ( 'NONE', #29654, #8270 ) ;
#1405 = CARTESIAN_POINT ( 'NONE',  ( 56.97280603064898941, -277.2763395528616002, 1.500000000000000000 ) ) ;
#1406 = CARTESIAN_POINT ( 'NONE',  ( 48.06508596181272708, -7.548662730768715079, -4.522129901861164036 ) ) ;
#1407 = ORIENTED_EDGE ( 'NONE', *, *, #7509, .T. ) ;
#1408 = DIRECTION ( 'NONE',  ( 0.000000000000000000, 0.000000000000000000, 1.000000000000000000 ) ) ;
#1409 = EDGE_CURVE ( 'NONE', #21301, #32600, #13383, .T. ) ;
#1410 = CARTESIAN_POINT ( 'NONE',  ( 107.4385791398478744, 17.85938043952739918, 4.629213727441585213 ) ) ;
#1411 = EDGE_CURVE ( 'NONE', #11371, #264, #7953, .T. ) ;
#1412 = DIRECTION ( 'NONE',  ( 0.000000000000000000, 0.5735764363510448272, -0.8191520442889927978 ) ) ;
#1413 = ORIENTED_EDGE ( 'NONE', *, *, #1242, .F. ) ;
#1414 = DIRECTION ( 'NONE',  ( 0.000000000000000000, 0.000000000000000000, -1.000000000000000000 ) ) ;
#1415 = CARTESIAN_POINT ( 'NONE',  ( 21.21813830868036632, -21.75718202030900983, -1.395944860339461968 ) ) ;
#1416 = ORIENTED_EDGE ( 'NONE', *, *, #33000, .T. ) ;
#1417 = CARTESIAN_POINT ( 'NONE',  ( 4.129790720829305428, -11.96909370240749482, -1.499999999999999556 ) ) ;
#1418 = VERTEX_POINT ( 'NONE', #10622 ) ;
#1419 = ORIENTED_EDGE ( 'NONE', *, *, #2054, .T. ) ;
#1420 = CARTESIAN_POINT ( 'NONE',  ( 25.43628654896174623, -17.54453578616395149, -1.000000000000000222 ) ) ;
#1422 = ORIENTED_EDGE ( 'NONE', *, *, #24866, .T. ) ;
#1421 = CARTESIAN_POINT ( 'NONE',  ( 3.063284526843530031, -4.729683950890320787, 7.360373001715534436 ) ) ;
#1423 = VERTEX_POINT ( 'NONE', #28534 ) ;
#1424 = CARTESIAN_POINT ( 'NONE',  ( 21.79750000136559507, 0.3178988483021036315, 3.024605502323848949 ) ) ;
#1425 = EDGE_CURVE ( 'NONE', #26729, #13791, #15811, .T. ) ;
#1427 = ORIENTED_EDGE ( 'NONE', *, *, #13616, .T. ) ;
#1426 = B_SPLINE_CURVE_WITH_KNOTS ( 'NONE', 3,
 ( #20510, #30720, #28173, #15639, #15450, #586, #10777, #8106 ),
 .UNSPECIFIED., .F., .F.,
 ( 4, 2, 2, 4 ),
 ( 0.000000000000000000, 0.5000000000000000000, 0.7500000000000000000, 1.000000000000000000 ),
 .UNSPECIFIED. ) ;
#1428 = CARTESIAN_POINT ( 'NONE',  ( 3.554613218822866294, -15.76807188677689631, 4.522129901861158707 ) ) ;
#1429 = CARTESIAN_POINT ( 'NONE',  ( 10.00000000000000000, -1.625881193364727917, 4.467071865485467086 ) ) ;
#1431 = ORIENTED_EDGE ( 'NONE', *, *, #24002, .F. ) ;
#1430 = FACE_OUTER_BOUND ( 'NONE', #16288, .T. ) ;
#1432 = CARTESIAN_POINT ( 'NONE',  ( 24.80306213860490061, -17.49230408913781787, -1.500000000000000000 ) ) ;
#1433 = CARTESIAN_POINT ( 'NONE',  ( 5.612718383992088889, 1.229942497144144165, -8.123482740191956708 ) ) ;
#1434 = LINE ( 'NONE', #1279, #9586 ) ;
#1435 = LINE ( 'NONE', #9086, #19970 ) ;
#1436 = DIRECTION ( 'NONE',  ( 0.000000000000000000, -0.000000000000000000, 1.000000000000000000 ) ) ;
#1437 = CARTESIAN_POINT ( 'NONE',  ( -2.819379691724354764, -6.927609664243463250, -4.522129901861166701 ) ) ;
#1438 = CARTESIAN_POINT ( 'NONE',  ( 102.5437075123492292, -5.726773290143884587, -0.4367666012718967594 ) ) ;
#1439 = CARTESIAN_POINT ( 'NONE',  ( 10.00000000000000178, 1.115095498423375409, -4.884328206559827024 ) ) ;
#1440 = EDGE_CURVE ( 'NONE', #228, #10851, #28184, .T. ) ;
#1441 = DIRECTION ( 'NONE',  ( 8.574039729943018344E-17, 1.000000000000000000, 0.000000000000000000 ) ) ;
#1442 = LINE ( 'NONE', #27158, #17729 ) ;
#1443 = DIRECTION ( 'NONE',  ( 0.000000000000000000, 0.000000000000000000, -1.000000000000000000 ) ) ;
#1444 = EDGE_CURVE ( 'NONE', #19214, #4152, #5906, .T. ) ;
#1445 = CARTESIAN_POINT ( 'NONE',  ( 0.000000000000000000, 19.50000000000000000, 0.000000000000000000 ) ) ;
#1446 = EDGE_CURVE ( 'NONE', #27971, #32312, #10186, .T. ) ;
#1447 = CARTESIAN_POINT ( 'NONE',  ( -5.300050802731187005, 1.549418761218566143, -2.853674364686379583 ) ) ;
#1448 = ORIENTED_EDGE ( 'NONE', *, *, #21254, .F. ) ;
#1449 = CARTESIAN_POINT ( 'NONE',  ( -6.700050800000000528, 2.983565686104819648, 0.3135853898029609677 ) ) ;
#1450 = CARTESIAN_POINT ( 'NONE',  ( 23.05582502382718602, -21.92970400627778460, -1.098154049131486509 ) ) ;
#1451 = CARTESIAN_POINT ( 'NONE',  ( 28.63490450844348345, -5.610497434546049433, -3.993434336023980791 ) ) ;
#1452 = CARTESIAN_POINT ( 'NONE',  ( 7.154313483739771939, -6.723190066291747868, 1.000000000000000000 ) ) ;
#1453 = ORIENTED_EDGE ( 'NONE', *, *, #16885, .F. ) ;
#1454 = CARTESIAN_POINT ( 'NONE',  ( 7.085399849431443187, -9.284427924817668654, -1.500000000000000444 ) ) ;
#1455 = ORIENTED_EDGE ( 'NONE', *, *, #8745, .F. ) ;
#1456 = CARTESIAN_POINT ( 'NONE',  ( 3.073984382316905961, -11.22322413323466606, 1.500000000000000444 ) ) ;
#1457 = DATE_AND_TIME ( #32231, #22121 ) ;
#1458 = CARTESIAN_POINT ( 'NONE',  ( -2.750050800000000351, 3.113457007523260156, -0.9222479816126439855 ) ) ;
#1459 = ORIENTED_EDGE ( 'NONE', *, *, #31745, .T. ) ;
#1460 = CARTESIAN_POINT ( 'NONE',  ( 28.67239840559724584, -6.439901994837876842, 4.275175838841350995 ) ) ;
#1461 = ADVANCED_FACE ( 'NONE', ( #16127 ), #3461, .F. ) ;
#1462 = CC_DESIGN_PERSON_AND_ORGANIZATION_ASSIGNMENT ( #31250, #28713, ( #1293 ) ) ;
#1463 = CARTESIAN_POINT ( 'NONE',  ( 19.67866930034583817, 15.15590071967975305, -1.050000000000000044 ) ) ;
#1464 = CARTESIAN_POINT ( 'NONE',  ( 40.87805050009787067, -5.806737366949438872, -4.073741263089366349 ) ) ;
#1465 = CARTESIAN_POINT ( 'NONE',  ( 10.00000000000000178, -8.574039729943018837E-16, 0.000000000000000000 ) ) ;
#1466 = CARTESIAN_POINT ( 'NONE',  ( 2.864531114197725881, 5.073635298885146305, 8.105385692883624316 ) ) ;
#1467 = B_SPLINE_CURVE_WITH_KNOTS ( 'NONE', 3,
 ( #3439, #26801, #31836, #31989, #23803, #13598, #8905, #6391, #16591, #16778 ),
 .UNSPECIFIED., .F., .F.,
 ( 4, 3, 3, 4 ),
 ( 1.734723475976807094E-18, 0.001000000000055348759, 0.002000000000112648647, 0.003363950672716857146 ),
 .UNSPECIFIED. ) ;
#1468 = ORIENTED_EDGE ( 'NONE', *, *, #11325, .T. ) ;
#1469 = CARTESIAN_POINT ( 'NONE',  ( -2.617344628312510135, 0.000000000000000000, 1.468739241856748867 ) ) ;
#1470 = CARTESIAN_POINT ( 'NONE',  ( 56.97280603064904625, -277.2763395528616002, 554.0683451991844777 ) ) ;
#1471 = CARTESIAN_POINT ( 'NONE',  ( 5.377543748152550762, -7.530955069117533540, 2.741043480754901118 ) ) ;
#1473 = ORIENTED_EDGE ( 'NONE', *, *, #11783, .T. ) ;
#1472 = CARTESIAN_POINT ( 'NONE',  ( 3.499999999999999556, 6.100541242131516384, -3.528937025535512362 ) ) ;
#1474 = LINE ( 'NONE', #19360, #22064 ) ;
#1475 = CARTESIAN_POINT ( 'NONE',  ( 23.95058674323790271, -2.449331254364353949, -0.07017451552781628354 ) ) ;
#1476 = CARTESIAN_POINT ( 'NONE',  ( 6.448894291894883501, -17.04229596238074151, -4.522129901861166701 ) ) ;
#1477 = CARTESIAN_POINT ( 'NONE',  ( -2.619932554246537343E-16, -3.055657119358776264, -3.641590349731960163 ) ) ;
#1478 = CARTESIAN_POINT ( 'NONE',  ( 2.795120570943885774, -9.022485053477835137, 3.714272345030835254 ) ) ;
#1479 = EDGE_CURVE ( 'NONE', #256, #2205, #935, .T. ) ;
#1480 = CARTESIAN_POINT ( 'NONE',  ( 5.612718383992089777, -1.229942497144091096, 8.123482740191967366 ) ) ;
#1481 = CARTESIAN_POINT ( 'NONE',  ( 24.73879325185242095, -17.41122989233535634, -1.266732818455850618 ) ) ;
#1482 = DIRECTION ( 'NONE',  ( -1.000000000000000000, 8.574039729943022041E-17, -3.081487911019577365E-33 ) ) ;
#1483 = ORIENTED_EDGE ( 'NONE', *, *, #21699, .T. ) ;
#1484 = CARTESIAN_POINT ( 'NONE',  ( 6.883866557622098981, 2.328663417917440359, 8.415306967752686162 ) ) ;
#1485 = ORIENTED_EDGE ( 'NONE', *, *, #23814, .F. ) ;
#1486 = CARTESIAN_POINT ( 'NONE',  ( 10.57125986779756843, -4.971152295393306275, 0.6226916219171877431 ) ) ;
#1487 =( BOUNDED_CURVE ( )  B_SPLINE_CURVE ( 2, ( #25849, #18969, #15798, #2966, #23323, #26007, #3113, #583, #1562, #24128, #14399 ),
 .UNSPECIFIED., .F., .F. ) 
 B_SPLINE_CURVE_WITH_KNOTS ( ( 3, 2, 2, 2, 2, 3 ),
 ( 0.8103822619934377691, 0.8125000000000000000, 0.8281250000000000000, 0.8437500000000000000, 0.8593750000000000000, 0.8728822619934377691 ),
 .UNSPECIFIED. ) 
 CURVE ( )  GEOMETRIC_REPRESENTATION_ITEM ( )  RATIONAL_B_SPLINE_CURVE ( ( 0.9821626249036861100, 0.9896829947469995004, 1.000000000000000000, 0.9238795325112867385, 1.000000000000000000, 0.9238795325112867385, 1.000000000000000000, 0.9238795325112867385, 1.000000000000000000, 0.9341965377642872381, 0.9821626249036861100 ) ) 
 REPRESENTATION_ITEM ( '' )  );
#1488 = CARTESIAN_POINT ( 'NONE',  ( -59.75626822162179508, -5.804869634004071521, 5.128141679950119602 ) ) ;
#1489 = CARTESIAN_POINT ( 'NONE',  ( 23.84310522038038727, -4.329614468550014195, -4.522129901861162260 ) ) ;
#1490 = CARTESIAN_POINT ( 'NONE',  ( 3.063284526839890276, 7.360373001730978082, -4.729683950898788680 ) ) ;
#1491 = DIRECTION ( 'NONE',  ( -1.000000000000000000, -0.000000000000000000, -0.000000000000000000 ) ) ;
#1492 = ORIENTED_EDGE ( 'NONE', *, *, #30465, .T. ) ;
#1493 = CARTESIAN_POINT ( 'NONE',  ( 107.7530755790500621, 16.80318731729051152, -2.530619919563210640 ) ) ;
#1494 = ORIENTED_EDGE ( 'NONE', *, *, #26545, .T. ) ;
#1495 = PERSON_AND_ORGANIZATION ( #6766, #25292 ) ;
#1496 = FACE_OUTER_BOUND ( 'NONE', #16801, .T. ) ;
#1497 = EDGE_CURVE ( 'NONE', #8026, #14221, #16590, .T. ) ;
#1498 = CARTESIAN_POINT ( 'NONE',  ( 7.433516504560094162, -4.668991481927904807, -1.000000000000000000 ) ) ;
#1499 = EDGE_LOOP ( 'NONE', ( #31808, #1754, #25386, #17203 ) ) ;
#1500 = CARTESIAN_POINT ( 'NONE',  ( 5.377543748152548986, -7.530955069117495349, -2.741043480755002371 ) ) ;
#1501 = ORIENTED_EDGE ( 'NONE', *, *, #21502, .T. ) ;
#1502 = ORIENTED_EDGE ( 'NONE', *, *, #6427, .T. ) ;
#1503 = CARTESIAN_POINT ( 'NONE',  ( 5.887530252753768067, 6.185189124321821552, 5.676096663009825072 ) ) ;
#1504 = PLANE ( 'NONE',  #11782 ) ;
#1505 = CARTESIAN_POINT ( 'NONE',  ( 21.67249999999999943, -1.291182301015472378, -2.378061970571982098 ) ) ;
#1506 = CARTESIAN_POINT ( 'NONE',  ( 2.821167764927612343, -11.54352467686084616, -1.759796262541038159 ) ) ;
#1508 = ORIENTED_EDGE ( 'NONE', *, *, #32177, .T. ) ;
#1507 = CARTESIAN_POINT ( 'NONE',  ( 0.000000000000000000, 0.000000000000000000, 0.000000000000000000 ) ) ;
#1509 = CARTESIAN_POINT ( 'NONE',  ( -7.137550801365592612, 3.368539882008727115, 1.828967928396026954 ) ) ;
#1510 = DIRECTION ( 'NONE',  ( 0.000000000000000000, 0.7071067811865466846, -0.7071067811865483499 ) ) ;
#1511 = CARTESIAN_POINT ( 'NONE',  ( 19.10390797508229710, -2.015740111943975066, 0.07017451552782062729 ) ) ;
#1512 = CARTESIAN_POINT ( 'NONE',  ( -33.81874022276151237, 19.50000000000000000, 1.977928362984240573 ) ) ;
#1513 = EDGE_LOOP ( 'NONE', ( #9183, #1110, #21796, #17096 ) ) ;
#1514 = EDGE_CURVE ( 'NONE', #21342, #4101, #4869, .T. ) ;
#1516 = ORIENTED_EDGE ( 'NONE', *, *, #29780, .F. ) ;
#1515 = CARTESIAN_POINT ( 'NONE',  ( -15.00903914005711925, -21.93932300455818307, 1.032046942684759161 ) ) ;
#1517 = EDGE_CURVE ( 'NONE', #25432, #22025, #1121, .T. ) ;
#1518 = CARTESIAN_POINT ( 'NONE',  ( 21.03177542174608661, -17.18603084754167298, 1.753176640694532162 ) ) ;
#1519 = EDGE_CURVE ( 'NONE', #26215, #10113, #11605, .T. ) ;
#1520 = CARTESIAN_POINT ( 'NONE',  ( 0.000000000000000000, 4.438567988583082879, 7.249076783337693008 ) ) ;
#1521 = CARTESIAN_POINT ( 'NONE',  ( 25.48500000136559507, 0.9349337715887185984, -3.156283516753368268 ) ) ;
#1522 = CARTESIAN_POINT ( 'NONE',  ( -23.54713438637982748, 18.90773822806172433, 1.500000000000000000 ) ) ;
#1523 = CARTESIAN_POINT ( 'NONE',  ( -4.184206142744113066, -5.072448364080297090, -1.499999999999959366 ) ) ;
#1524 = DIRECTION ( 'NONE',  ( 8.678904333908113252E-16, 0.000000000000000000, -1.000000000000000000 ) ) ;
#1525 = CARTESIAN_POINT ( 'NONE',  ( 68.93909985284442143, -3.497255374392779448, 1.529340295389710169 ) ) ;
#1526 = CARTESIAN_POINT ( 'NONE',  ( -3.987550801365593145, 3.521866450007987037, 0.3701630799359328372 ) ) ;
#1527 = ORIENTED_EDGE ( 'NONE', *, *, #21268, .T. ) ;
#1528 = DIRECTION ( 'NONE',  ( 1.000000000000000000, -0.000000000000000000, -0.000000000000000000 ) ) ;
#1529 = ORIENTED_EDGE ( 'NONE', *, *, #3176, .F. ) ;
#1530 = CARTESIAN_POINT ( 'NONE',  ( 7.249760686538667009, -1.391664247347281780, 7.892520144992429820 ) ) ;
#1531 = DIRECTION ( 'NONE',  ( -1.000000000000000000, -0.000000000000000000, -0.000000000000000000 ) ) ;
#1533 = DIRECTION ( 'NONE',  ( 0.000000000000000000, 0.000000000000000000, 1.000000000000000000 ) ) ;
#1532 = CARTESIAN_POINT ( 'NONE',  ( -3.700050800000000084, 0.3135853898029611342, -2.983565686104819648 ) ) ;
#1534 = EDGE_LOOP ( 'NONE', ( #13575, #12250, #8340, #1062 ) ) ;
#1535 = CARTESIAN_POINT ( 'NONE',  ( -50.81000000000000227, -10.96999999999998643, 5.700000000000000178 ) ) ;
#1536 = VERTEX_POINT ( 'NONE', #29508 ) ;
#1537 = DIRECTION ( 'NONE',  ( 0.9975973382524639943, 0.06927878976713691683, -8.540109289633579845E-19 ) ) ;
#1539 = ORIENTED_EDGE ( 'NONE', *, *, #23640, .F. ) ;
#1538 = CARTESIAN_POINT ( 'NONE',  ( 54.94558419843593100, -5.363357418298841495, -3.999773680160701783 ) ) ;
#1540 = EDGE_LOOP ( 'NONE', ( #14662, #16932, #13034, #23553 ) ) ;
#1541 = DIRECTION ( 'NONE',  ( -0.7071067811865467956, 8.659560562354925463E-17, 0.7071067811865483499 ) ) ;
#1542 = CARTESIAN_POINT ( 'NONE',  ( 10.00000000000000000, -2.376879293651037006, -4.116875700062107235 ) ) ;
#1543 = EDGE_CURVE ( 'NONE', #10253, #11257, #13905, .T. ) ;
#1545 = ORIENTED_EDGE ( 'NONE', *, *, #13133, .T. ) ;
#1544 = CARTESIAN_POINT ( 'NONE',  ( 0.2309143942741746225, -15.52425963734929404, -1.499999999999999778 ) ) ;
#1546 = CARTESIAN_POINT ( 'NONE',  ( -34.48223484310472031, 0.5000000000000000000, 2.552009564962238297 ) ) ;
#1547 = CARTESIAN_POINT ( 'NONE',  ( 3.249999999999999556, -2.223716399045632119, 8.461683424509308438 ) ) ;
#1548 = FACE_OUTER_BOUND ( 'NONE', #10560, .T. ) ;
#1549 = CARTESIAN_POINT ( 'NONE',  ( 7.650166298460330694, -9.403575860117920016, -1.500000000000286438 ) ) ;
#1551 = VERTEX_POINT ( 'NONE', #24147 ) ;
#1550 = CARTESIAN_POINT ( 'NONE',  ( 107.9747431708452012, -17.70567005987862785, -5.016769268009813487 ) ) ;
#1552 = CARTESIAN_POINT ( 'NONE',  ( -4.607304909706597229, -1.062355717592097015, -2.999999999999998668 ) ) ;
#1553 = LINE ( 'NONE', #8752, #7565 ) ;
#1554 = DIRECTION ( 'NONE',  ( 0.000000000000000000, 0.7071067811865434649, 0.7071067811865516806 ) ) ;
#1555 = DIRECTION ( 'NONE',  ( -1.000000000000000000, -0.000000000000000000, -0.000000000000000000 ) ) ;
#1556 = CARTESIAN_POINT ( 'NONE',  ( 0.000000000000000000, 4.058600654062850310, 7.468451026206211374 ) ) ;
#1557 = VERTEX_POINT ( 'NONE', #9080 ) ;
#1558 = CARTESIAN_POINT ( 'NONE',  ( 0.3045634671934224214, 0.9829946734957575316, 10.22982953726899957 ) ) ;
#1559 = DIRECTION ( 'NONE',  ( 0.000000000000000000, 0.000000000000000000, 1.000000000000000000 ) ) ;
#1560 = CARTESIAN_POINT ( 'NONE',  ( -23.35000000000000142, -10.96966150227469505, -1.499999999999999556 ) ) ;
#1561 = EDGE_LOOP ( 'NONE', ( #17178, #14253, #1004, #18496 ) ) ;
#1562 = CARTESIAN_POINT ( 'NONE',  ( -2.250050802731187183, -1.887961173149512062, -2.331437884370912261 ) ) ;
#1563 = CARTESIAN_POINT ( 'NONE',  ( 2.802272078496797825, -0.3634031030573144361, -1.485394228827264351 ) ) ;
#1564 = VERTEX_POINT ( 'NONE', #1429 ) ;
#1565 = CARTESIAN_POINT ( 'NONE',  ( 7.249760686538667009, -8.014274990069656823, 8.669741416787380218E-17 ) ) ;
#1566 = EDGE_CURVE ( 'NONE', #25432, #26782, #19131, .T. ) ;
#1567 = VERTEX_POINT ( 'NONE', #1274 ) ;
#1568 = ORIENTED_EDGE ( 'NONE', *, *, #19353, .F. ) ;
#1569 = CARTESIAN_POINT ( 'NONE',  ( 69.13057415542957074, -2.987362752442195291, -2.713652344655540727 ) ) ;
#1570 = EDGE_CURVE ( 'NONE', #31361, #23619, #3258, .T. ) ;
#1572 = EDGE_LOOP ( 'NONE', ( #30390, #4020, #23354, #26459 ) ) ;
#1571 = CARTESIAN_POINT ( 'NONE',  ( 2.440333830125739567, -5.258796312403307915, 9.290196408096516478 ) ) ;
#1573 = ORIENTED_EDGE ( 'NONE', *, *, #19612, .F. ) ;
#1574 = CARTESIAN_POINT ( 'NONE',  ( 23.36000000136559507, 0.9349337715887185984, -3.156283516753368268 ) ) ;
#1575 = ORIENTED_EDGE ( 'NONE', *, *, #4757, .F. ) ;
#1576 = FACE_OUTER_BOUND ( 'NONE', #23149, .T. ) ;
#1577 = LINE ( 'NONE', #29322, #27820 ) ;
#1579 = ORIENTED_EDGE ( 'NONE', *, *, #20186, .T. ) ;
#1578 = CYLINDRICAL_SURFACE ( 'NONE', #13324, 5.010000000000000675 ) ;
#1580 = DIRECTION ( 'NONE',  ( -3.623545766764194901E-17, -0.4226182617406968878, -0.9063077870366511579 ) ) ;
#1581 = VECTOR ( 'NONE', #30520, 1000.000000000000000 ) ;
#1582 = CARTESIAN_POINT ( 'NONE',  ( 10.00000000000000000, -2.376879293651037006, -4.116875700062107235 ) ) ;
#1583 = B_SPLINE_CURVE_WITH_KNOTS ( 'NONE', 3,
 ( #26620, #5892, #8410, #28794, #13404, #6077, #23791, #21280, #19102, #18772, #3724, #20963, #31333, #748, #31479, #26478, #21616, #31183, #1228, #3243, #8265, #11421, #16081, #18457, #6376, #26311, #3424, #8561, #29290, #26784, #28977, #3577 ),
 .UNSPECIFIED., .F., .F.,
 ( 4, 2, 2, 2, 2, 2, 2, 2, 2, 2, 2, 2, 2, 2, 2, 4 ),
 ( 0.09044956997018868683, 0.09470617999383536267, 0.09896279001748202464, 0.1032194000411287005, 0.1074760100647753763, 0.1085401625706870349, 0.1096043150765987073, 0.1117326200884220522, 0.1127967725943337107, 0.1138609251002453970, 0.1149250776061570556, 0.1159892301120687419, 0.1181175351238920868, 0.1191816876298037453, 0.1202458401357154177, 0.1245024501593621075 ),
 .UNSPECIFIED. ) ;
#1584 = EDGE_CURVE ( 'NONE', #10995, #30996, #32023, .T. ) ;
#1585 = CARTESIAN_POINT ( 'NONE',  ( 101.8405149130903027, -4.601938079581686658, 3.093519980324558549 ) ) ;
#1586 = CARTESIAN_POINT ( 'NONE',  ( -8.000050800000000351, 0.000000000000000000, -3.000000000000000444 ) ) ;
#1587 = CIRCLE ( 'NONE', #29865, 0.5000000000000004441 ) ;
#1588 = CARTESIAN_POINT ( 'NONE',  ( 3.551765900376503193, -15.35947713381494673, -5.485967528433938867 ) ) ;
#1589 = FACE_OUTER_BOUND ( 'NONE', #23217, .T. ) ;
#1590 = ADVANCED_FACE ( 'NONE', ( #21650 ), #24460, .T. ) ;
#1591 = DIRECTION ( 'NONE',  ( -1.000000000000000000, 0.000000000000000000, 0.000000000000000000 ) ) ;
#1592 = CARTESIAN_POINT ( 'NONE',  ( 16.25784845243109800, -4.536028529981986301E-15, 0.000000000000000000 ) ) ;
#1593 = CARTESIAN_POINT ( 'NONE',  ( 23.67250000273118715, -2.378061970571983430, 1.291182301015471490 ) ) ;
#1594 = CARTESIAN_POINT ( 'NONE',  ( 21.25111450864416085, -3.256483526998273983E-15, 2.499999999999998668 ) ) ;
#1595 = CARTESIAN_POINT ( 'NONE',  ( -6.850050802731187716, 2.331437884370912705, -1.887961173149511618 ) ) ;
#1596 = EDGE_LOOP ( 'NONE', ( #5955, #19738, #3255, #12058 ) ) ;
#1597 = EDGE_CURVE ( 'NONE', #10281, #29127, #1577, .T. ) ;
#1598 = CARTESIAN_POINT ( 'NONE',  ( -7.687550801365593323, -2.752080473201636845, 2.228590825266444586 ) ) ;
#1599 = CIRCLE ( 'NONE', #19206, 297.9387600756452912 ) ;
#1600 = VECTOR ( 'NONE', #17835, 1000.000000000000000 ) ;
#1601 = CYLINDRICAL_SURFACE ( 'NONE', #739, 0.4500000000000004552 ) ;
#1602 = CARTESIAN_POINT ( 'NONE',  ( 3.499999999999999556, 3.771202944355777298, -4.982773259188332027 ) ) ;
#1603 = CARTESIAN_POINT ( 'NONE',  ( 8.690022415558827262, -0.1784382875756478082, 1.500000000000000000 ) ) ;
#1604 = VERTEX_POINT ( 'NONE', #13769 ) ;
#1605 = LINE ( 'NONE', #1792, #5332 ) ;
#1606 = CARTESIAN_POINT ( 'NONE',  ( -7.300050800000001061, -0.3135853898029607456, 2.983565686104819648 ) ) ;
#1607 = AXIS2_PLACEMENT_3D ( 'NONE', #226, #10895, #13366 ) ;
#1608 = VERTEX_POINT ( 'NONE', #27145 ) ;
#1609 = CARTESIAN_POINT ( 'NONE',  ( 0.2309801563857631079, -6.520475440346420903, 1.500000000000070388 ) ) ;
#1610 = COORDINATED_UNIVERSAL_TIME_OFFSET ( 0, 0, .AHEAD. ) ;
#1611 = CARTESIAN_POINT ( 'NONE',  ( -2.557304906975409686, 1.062355717592091686, 3.000000000000001332 ) ) ;
#1612 = ORIENTED_EDGE ( 'NONE', *, *, #27716, .T. ) ;
#1613 = CARTESIAN_POINT ( 'NONE',  ( 9.266707753004491011, -0.05004968855533440536, -1.221243012139963779 ) ) ;
#1614 = CARTESIAN_POINT ( 'NONE',  ( -6.000050800000000351, 2.331437884370912705, -1.887961173149511618 ) ) ;
#1615 = CARTESIAN_POINT ( 'NONE',  ( 69.05424452633151589, -5.791958783353122087, -4.275175994963405834 ) ) ;
#1616 = CARTESIAN_POINT ( 'NONE',  ( 24.37248106195859876, -17.41561295274971499, -1.432003413859580965 ) ) ;
#1618 = CARTESIAN_POINT ( 'NONE',  ( -12.44989959798873791, 20.00000000000000000, -1.818740222761504599 ) ) ;
#1617 = B_SPLINE_CURVE_WITH_KNOTS ( 'NONE', 3,
 ( #31590, #5688, #28595, #26426, #994, #15866, #31278, #8677 ),
 .UNSPECIFIED., .F., .F.,
 ( 4, 2, 2, 4 ),
 ( 2.152606640961436226E-07, 0.001262065476475215334, 0.001892990584380772065, 0.002523915692286328796 ),
 .UNSPECIFIED. ) ;
#1619 = ORIENTED_EDGE ( 'NONE', *, *, #17958, .F. ) ;
#1620 = EDGE_CURVE ( 'NONE', #32817, #4832, #29019, .T. ) ;
#1621 = VECTOR ( 'NONE', #12295, 1000.000000000000114 ) ;
#1622 = CARTESIAN_POINT ( 'NONE',  ( 25.75999999999999801, -2.208672634433321348E-15, 0.000000000000000000 ) ) ;
#1623 = EDGE_CURVE ( 'NONE', #1608, #15940, #18476, .T. ) ;
#1624 = CARTESIAN_POINT ( 'NONE',  ( 23.14329945973239333, -21.92788238883852259, -1.164089052066207941 ) ) ;
#1625 = CARTESIAN_POINT ( 'NONE',  ( 18.91888895626146905, -4.083881414823423484, -2.942177715856218789 ) ) ;
#1626 = CIRCLE ( 'NONE', #28847, 2.999999999999999112 ) ;
#1628 = ORIENTED_EDGE ( 'NONE', *, *, #28715, .T. ) ;
#1627 = CARTESIAN_POINT ( 'NONE',  ( 25.69585612515879092, 2.874579352301957602, -0.7480745300778689488 ) ) ;
#1629 = DIRECTION ( 'NONE',  ( 1.000000000000000000, -8.574039729943018344E-17, -0.000000000000000000 ) ) ;
#1630 = CIRCLE ( 'NONE', #20320, 6.248999999999999666 ) ;
#1631 = CARTESIAN_POINT ( 'NONE',  ( 85.08949032934708612, -1.315411135598755221, -0.07017451552781628354 ) ) ;
#1632 = CARTESIAN_POINT ( 'NONE',  ( 17.97422212135272446, -19.86246923125032282, -4.522129901861166701 ) ) ;
#1633 = CARTESIAN_POINT ( 'NONE',  ( 26.08945412691628007, 19.05746434167072678, 1.082350151677544448 ) ) ;
#1634 = CARTESIAN_POINT ( 'NONE',  ( 34.48223484310469900, 0.5000000000000000000, 2.482234843104950350 ) ) ;
#1635 = EDGE_CURVE ( 'NONE', #14801, #31497, #24317, .T. ) ;
#1636 = AXIS2_PLACEMENT_3D ( 'NONE', #7760, #5238, #9921 ) ;
#1637 = CARTESIAN_POINT ( 'NONE',  ( -8.000050800000002127, 3.541248556864417196, 0.01107501445590582979 ) ) ;
#1638 = DIRECTION ( 'NONE',  ( 0.000000000000000000, 0.000000000000000000, 1.000000000000000000 ) ) ;
#1639 = DIRECTION ( 'NONE',  ( 0.000000000000000000, 0.9961946980917459893, -0.08715574274765196250 ) ) ;
#1640 = PLANE ( 'NONE',  #23083 ) ;
#1641 = ORIENTED_EDGE ( 'NONE', *, *, #15129, .F. ) ;
#1642 = DIRECTION ( 'NONE',  ( -0.000000000000000000, -0.000000000000000000, -1.000000000000000000 ) ) ;
#1643 = EDGE_LOOP ( 'NONE', ( #10456, #32959, #14875, #30341, #27670, #10174, #30850, #10845, #20092, #17328, #19615 ) ) ;
#1644 = ADVANCED_FACE ( 'NONE', ( #19486 ), #23970, .T. ) ;
#1645 = DIRECTION ( 'NONE',  ( 0.000000000000000000, 0.08715574274766293983, -0.9961946980917451011 ) ) ;
#1646 = CC_DESIGN_PERSON_AND_ORGANIZATION_ASSIGNMENT ( #31359, #10614, ( #6102 ) ) ;
#1647 = PLANE ( 'NONE',  #32162 ) ;
#1648 = VECTOR ( 'NONE', #9674, 1000.000000000000000 ) ;
#1649 = DIRECTION ( 'NONE',  ( 1.000000000000000000, -0.000000000000000000, -0.000000000000000000 ) ) ;
#1650 = CARTESIAN_POINT ( 'NONE',  ( -8.000050800000000351, 0.3135937863663861291, -2.983645574069408557 ) ) ;
#1651 = CARTESIAN_POINT ( 'NONE',  ( 47.95270804829356592, -8.021719045401216164, 1.873788950397360820 ) ) ;
#1652 = ORIENTED_EDGE ( 'NONE', *, *, #5719, .T. ) ;
#1653 = CARTESIAN_POINT ( 'NONE',  ( 3.499999999999999556, 0.000000000000000000, 0.000000000000000000 ) ) ;
#1654 = AXIS2_PLACEMENT_3D ( 'NONE', #5855, #23759, #26449 ) ;
#1655 = EDGE_LOOP ( 'NONE', ( #849, #17253, #24445, #22913 ) ) ;
#1656 = PERSON_AND_ORGANIZATION ( #6766, #25292 ) ;
#1657 = CARTESIAN_POINT ( 'NONE',  ( 85.03478631109508967, -5.187975910970339832, 4.018749453427868268 ) ) ;
#1658 = CIRCLE ( 'NONE', #32090, 9.425032312242976218 ) ;
#1659 = DIRECTION ( 'NONE',  ( 1.000000000000000000, -0.000000000000000000, -0.000000000000000000 ) ) ;
#1660 = DIRECTION ( 'NONE',  ( 0.000000000000000000, 1.000000000000000000, 0.000000000000000000 ) ) ;
#1661 = ORIENTED_EDGE ( 'NONE', *, *, #372, .F. ) ;
#1662 = ORIENTED_EDGE ( 'NONE', *, *, #25580, .F. ) ;
#1663 = EDGE_CURVE ( 'NONE', #12973, #12534, #8780, .T. ) ;
#1664 = CARTESIAN_POINT ( 'NONE',  ( 7.064632951172269415, 6.226446564517915228, 6.147671362329237610 ) ) ;
#1665 = CARTESIAN_POINT ( 'NONE',  ( 6.037141869538512395, -7.552970526864664080, -3.843044125430146174 ) ) ;
#1666 = CARTESIAN_POINT ( 'NONE',  ( 25.17249999999999943, 1.291182301015469047, 2.378061970571981654 ) ) ;
#1667 = B_SPLINE_CURVE_WITH_KNOTS ( 'NONE', 3,
 ( #9661, #2653, #12671, #2343, #19886, #17374, #7180, #27567, #4666, #20211 ),
 .UNSPECIFIED., .F., .F.,
 ( 4, 2, 2, 2, 4 ),
 ( 1.968338519011545307E-07, 0.0005467926395225674360, 0.001093388445193233666, 0.001639984250863899895, 0.002186580056534566125 ),
 .UNSPECIFIED. ) ;
#1668 = CARTESIAN_POINT ( 'NONE',  ( 3.920802734502714770, -12.31850478943684557, -1.757814695358448365 ) ) ;
#1670 = VERTEX_POINT ( 'NONE', #30949 ) ;
#1669 = CARTESIAN_POINT ( 'NONE',  ( 5.885541806331896275, 3.871259391815556228, -7.447669719165293856 ) ) ;
#1671 = CARTESIAN_POINT ( 'NONE',  ( -7.962550801365594566, 2.752080473201636845, -2.228590825266444142 ) ) ;
#1672 = CARTESIAN_POINT ( 'NONE',  ( 10.00000000000000000, -4.467071865485462645, -1.625881193364742572 ) ) ;
#1673 = VECTOR ( 'NONE', #18833, 1000.000000000000000 ) ;
#1674 = CARTESIAN_POINT ( 'NONE',  ( -4.599999999999996092, 0.000000000000000000, 0.000000000000000000 ) ) ;
#1675 = DIRECTION ( 'NONE',  ( 0.000000000000000000, 0.000000000000000000, 1.000000000000000000 ) ) ;
#1676 = ORIENTED_EDGE ( 'NONE', *, *, #19097, .F. ) ;
#1678 = ORIENTED_EDGE ( 'NONE', *, *, #14870, .T. ) ;
#1677 = CARTESIAN_POINT ( 'NONE',  ( 13.62547635268499135, 21.94000000000002970, 1.081074820185998320 ) ) ;
#1679 = VECTOR ( 'NONE', #13330, 1000.000000000000000 ) ;
#1680 = AXIS2_PLACEMENT_3D ( 'NONE', #18385, #3337, #5674 ) ;
#1682 = AXIS2_PLACEMENT_3D ( 'NONE', #2754, #7773, #559 ) ;
#1681 = DIRECTION ( 'NONE',  ( 0.000000000000000000, 1.000000000000000000, 0.000000000000000000 ) ) ;
#1683 = PLANE ( 'NONE',  #18957 ) ;
#1684 = CARTESIAN_POINT ( 'NONE',  ( 24.86000000136559507, 1.570731468192929858, 2.892927487894329630 ) ) ;
#1685 = ADVANCED_FACE ( 'NONE', ( #30646 ), #28442, .T. ) ;
#1686 = CARTESIAN_POINT ( 'NONE',  ( -6.162942409646512409, 7.727249047114547632E-16, -2.999999999999999556 ) ) ;
#1687 = FACE_OUTER_BOUND ( 'NONE', #21236, .T. ) ;
#1688 = AXIS2_PLACEMENT_3D ( 'NONE', #14919, #25128, #28145 ) ;
#1689 = CARTESIAN_POINT ( 'NONE',  ( 25.10999999999999943, 1.942864903642424146, 1.573300977624592534 ) ) ;
#1690 = CARTESIAN_POINT ( 'NONE',  ( 29.33517104211142268, -3.852857368063845822, 1.169950485891758429 ) ) ;
#1691 = CARTESIAN_POINT ( 'NONE',  ( -4.037550801365593856, 3.675193018007247403, -1.088641768524161391 ) ) ;
#1692 = ORIENTED_EDGE ( 'NONE', *, *, #28673, .T. ) ;
#1693 = CARTESIAN_POINT ( 'NONE',  ( 69.42401195566041849, -8.835509274224046194, -0.07017451552783579571 ) ) ;
#1694 = ORIENTED_EDGE ( 'NONE', *, *, #27162, .F. ) ;
#1695 = CARTESIAN_POINT ( 'NONE',  ( 21.19329141388212534, -21.80292992253753326, 1.345625751490156174 ) ) ;
#1697 = VECTOR ( 'NONE', #32166, 1000.000000000000000 ) ;
#1696 = CARTESIAN_POINT ( 'NONE',  ( 0.000000000000000000, 0.000000000000000000, 0.000000000000000000 ) ) ;
#1698 = CARTESIAN_POINT ( 'NONE',  ( 19.03654924710325602, -2.768675503676416572, -2.713652344655542503 ) ) ;
#1699 = CARTESIAN_POINT ( 'NONE',  ( 1.624999999999999778, 9.915734732513284300, -4.762163868918169563 ) ) ;
#1700 = ORIENTED_EDGE ( 'NONE', *, *, #28290, .T. ) ;
#1701 = ADVANCED_FACE ( 'NONE', ( #7724 ), #13437, .T. ) ;
#1702 = TOROIDAL_SURFACE ( 'NONE', #14492, 3.895301350492843540, 15.00000000000000178 ) ;
#1703 = LINE ( 'NONE', #27097, #25690 ) ;
#1704 = AXIS2_PLACEMENT_3D ( 'NONE', #2013, #27580, #19721 ) ;
#1705 = VERTEX_POINT ( 'NONE', #15735 ) ;
#1706 = CARTESIAN_POINT ( 'NONE',  ( 2.619932554246560023E-16, 3.055657119358801133, 3.641590349731939735 ) ) ;
#1707 = ADVANCED_FACE ( 'NONE', ( #7532 ), #3073, .T. ) ;
#1709 = ORIENTED_EDGE ( 'NONE', *, *, #2626, .T. ) ;
#1708 = CARTESIAN_POINT ( 'NONE',  ( 28.69357983231036613, -5.616541217350277115, -3.994702635790153167 ) ) ;
#1710 = ORIENTED_EDGE ( 'NONE', *, *, #26107, .F. ) ;
#1711 = TOROIDAL_SURFACE ( 'NONE', #15052, 6.500000000000002665, 0.5000000000000000000 ) ;
#1712 = CARTESIAN_POINT ( 'NONE',  ( -2.921917104085873590E-16, -3.407865132560205623, 3.672404558090026860 ) ) ;
#1714 = CIRCLE ( 'NONE', #8101, 5.009999999999999787 ) ;
#1713 = CARTESIAN_POINT ( 'NONE',  ( 85.08949032934707191, -1.315411135598753445, 1.010822989962091301 ) ) ;
#1716 = ORIENTED_EDGE ( 'NONE', *, *, #10389, .T. ) ;
#1715 = DIRECTION ( 'NONE',  ( 0.000000000000000000, -8.881784197001252323E-16, 1.000000000000000000 ) ) ;
#1717 = CARTESIAN_POINT ( 'NONE',  ( 19.81525666554439269, 15.27091977432025338, -1.499999999999881428 ) ) ;
#1718 = CARTESIAN_POINT ( 'NONE',  ( -3.148734258548762383E-16, -3.672404558090014426, -3.407865132560218946 ) ) ;
#1719 = CARTESIAN_POINT ( 'NONE',  ( -3.064492245890347188, 0.000000000000000000, -1.000000000000000222 ) ) ;
#1720 = CARTESIAN_POINT ( 'NONE',  ( 9.037136197878623989, -11.91234824294515704, -1.500000000000000000 ) ) ;
#1722 = EDGE_LOOP ( 'NONE', ( #5182, #32473, #8911, #9479 ) ) ;
#1721 = CARTESIAN_POINT ( 'NONE',  ( 108.0346010918886890, -18.56760923201772329, -5.018359539779770451 ) ) ;
#1723 = CARTESIAN_POINT ( 'NONE',  ( 2.671540748214986660, 0.5000000000000006661, 1.500000000000000000 ) ) ;
#1724 = CIRCLE ( 'NONE', #13519, 0.4499999999999999001 ) ;
#1725 = AXIS2_PLACEMENT_3D ( 'NONE', #14247, #17432, #6740 ) ;
#1726 = LINE ( 'NONE', #4403, #8633 ) ;
#1727 = FACE_OUTER_BOUND ( 'NONE', #16561, .T. ) ;
#1728 = VECTOR ( 'NONE', #870, 1000.000000000000000 ) ;
#1729 = AXIS2_PLACEMENT_3D ( 'NONE', #29887, #1985, #18577 ) ;
#1730 = CARTESIAN_POINT ( 'NONE',  ( 3.499999999999999556, 6.100541242131516384, 3.528937025535512362 ) ) ;
#1731 = CARTESIAN_POINT ( 'NONE',  ( 0.3045634274093902416, -8.853895822767180235, -5.217683548413607930 ) ) ;
#1732 = ORIENTED_EDGE ( 'NONE', *, *, #12692, .F. ) ;
#1733 = CARTESIAN_POINT ( 'NONE',  ( 0.000000000000000000, 19.51744974835125035, 7.318435636271054534 ) ) ;
#1734 = AXIS2_PLACEMENT_3D ( 'NONE', #23832, #3135, #10802 ) ;
#1735 = AXIS2_PLACEMENT_3D ( 'NONE', #21226, #1160, #16206 ) ;
#1736 = DIRECTION ( 'NONE',  ( 0.9896144216807899463, -0.000000000000000000, 0.1437473352845038410 ) ) ;
#1737 = CARTESIAN_POINT ( 'NONE',  ( 2.440333863880882248, -7.210444323286300694, -7.872241054361076351 ) ) ;
#1738 = ORIENTED_EDGE ( 'NONE', *, *, #6747, .F. ) ;
#1739 = AXIS2_PLACEMENT_3D ( 'NONE', #4236, #6750, #7255 ) ;
#1740 = CARTESIAN_POINT ( 'NONE',  ( -55.59999999999999432, -10.96966150227468972, 1.500000000000000000 ) ) ;
#1741 = CARTESIAN_POINT ( 'NONE',  ( -53.47134659355816666, 5.052751005448547161, 3.951405864347744323 ) ) ;
#1742 = ORIENTED_EDGE ( 'NONE', *, *, #21414, .F. ) ;
#1743 = DIRECTION ( 'NONE',  ( 0.000000000000000000, -0.7071067811865410224, -0.7071067811865540120 ) ) ;
#1744 = EDGE_CURVE ( 'NONE', #23377, #9415, #27267, .T. ) ;
#1745 = VERTEX_POINT ( 'NONE', #213 ) ;
#1746 = EDGE_CURVE ( 'NONE', #15957, #28480, #32106, .T. ) ;
#1747 = CIRCLE ( 'NONE', #18282, 6.248999999999999666 ) ;
#1748 = ORIENTED_EDGE ( 'NONE', *, *, #7674, .T. ) ;
#1749 = CARTESIAN_POINT ( 'NONE',  ( 10.52034268205830259, 3.024842911000744206, -3.993798362933278057 ) ) ;
#1750 = COORDINATED_UNIVERSAL_TIME_OFFSET ( 0, 0, .AHEAD. ) ;
#1751 = VECTOR ( 'NONE', #28095, 1000.000000000000000 ) ;
#1753 = ORIENTED_EDGE ( 'NONE', *, *, #25497, .T. ) ;
#1752 = CARTESIAN_POINT ( 'NONE',  ( 17.39502519979081185, -21.04076415203811479, -1.751145182513948573 ) ) ;
#1754 = ORIENTED_EDGE ( 'NONE', *, *, #6925, .T. ) ;
#1755 = CARTESIAN_POINT ( 'NONE',  ( 22.17250000136559507, -2.363507492473152283, -1.913930629741525280 ) ) ;
#1756 = VECTOR ( 'NONE', #32491, 1000.000000000000000 ) ;
#1757 = AXIS2_PLACEMENT_3D ( 'NONE', #15577, #25796, #24255 ) ;
#1758 = AXIS2_PLACEMENT_3D ( 'NONE', #7273, #2271, #12455 ) ;
#1759 = ORIENTED_EDGE ( 'NONE', *, *, #29459, .T. ) ;
#1760 = CARTESIAN_POINT ( 'NONE',  ( 0.3749743454410877086, -2.260462012960331890, 9.839947797887042213 ) ) ;
#1761 = CARTESIAN_POINT ( 'NONE',  ( -1.218076164763124636, -14.00532792343563848, -1.500000000000000000 ) ) ;
#1763 = ORIENTED_EDGE ( 'NONE', *, *, #19526, .T. ) ;
#1762 = CARTESIAN_POINT ( 'NONE',  ( 102.5305753040692878, -0.1042037546421146210, -0.07017451552781628354 ) ) ;
#1764 = CARTESIAN_POINT ( 'NONE',  ( 0.000000000000000000, 0.000000000000000000, 0.000000000000000000 ) ) ;
#1765 = DIRECTION ( 'NONE',  ( 0.000000000000000000, 0.000000000000000000, -1.000000000000000000 ) ) ;
#1766 = CARTESIAN_POINT ( 'NONE',  ( 6.038144853276843804, 1.027626812408000800, 8.412419482080409239 ) ) ;
#1767 = CARTESIAN_POINT ( 'NONE',  ( 20.98500000136559862, -0.9349337715887248157, 3.156283516753367824 ) ) ;
#1768 = DIRECTION ( 'NONE',  ( 0.000000000000000000, 0.2588190451025176309, 0.9659258262890692004 ) ) ;
#1769 = AXIS2_PLACEMENT_3D ( 'NONE', #30449, #25430, #7870 ) ;
#1770 = CARTESIAN_POINT ( 'NONE',  ( -2.408800074497261079, -5.498703686517334432, -5.485967528433938867 ) ) ;
#1771 = CARTESIAN_POINT ( 'NONE',  ( 23.61221640758335027, -8.051464822112823327, -0.4367666033548386340 ) ) ;
#1772 = CARTESIAN_POINT ( 'NONE',  ( 10.43095328441111924, 21.14375246189590030, -1.491740999229418385 ) ) ;
#1773 = VECTOR ( 'NONE', #10695, 1000.000000000000000 ) ;
#1774 = CARTESIAN_POINT ( 'NONE',  ( -1.149978682276028286, 0.000000000000000000, 7.916915373446320459 ) ) ;
#1775 = AXIS2_PLACEMENT_3D ( 'NONE', #31225, #26180, #5639 ) ;
#1776 = DIRECTION ( 'NONE',  ( 0.000000000000000000, -0.9510565162951500895, -0.3090169943749582204 ) ) ;
#1777 = CARTESIAN_POINT ( 'NONE',  ( 10.00000000000000000, 1.625881193364696831, 4.467071865485476856 ) ) ;
#1778 = AXIS2_PLACEMENT_3D ( 'NONE', #15682, #31062, #31244 ) ;
#1779 = AXIS2_PLACEMENT_3D ( 'NONE', #14596, #14098, #9407 ) ;
#1780 = CARTESIAN_POINT ( 'NONE',  ( 3.249999999999999556, -3.174628368996019301, -8.152713396088794084 ) ) ;
#1781 = CARTESIAN_POINT ( 'NONE',  ( -7.100050802731186828, -2.853674364686378695, -1.549418761218566809 ) ) ;
#1782 = VERTEX_POINT ( 'NONE', #5366 ) ;
#1783 = CIRCLE ( 'NONE', #12992, 0.4500000000000017875 ) ;
#1784 = CARTESIAN_POINT ( 'NONE',  ( -4.500050800000000351, 0.3135853898029611342, -2.983565686104819648 ) ) ;
#1785 = EDGE_CURVE ( 'NONE', #3483, #11786, #17671, .T. ) ;
#1786 = B_SPLINE_CURVE_WITH_KNOTS ( 'NONE', 3,
 ( #3765, #4104, #26830, #19492, #14270, #1766, #24466, #32369, #29684, #4253 ),
 .UNSPECIFIED., .F., .F.,
 ( 4, 2, 2, 2, 4 ),
 ( 1.968338519010709921E-07, 0.0005467928198071728228, 0.001093388805762444439, 0.001639984791717716056, 0.002186580777672988106 ),
 .UNSPECIFIED. ) ;
#1787 = VECTOR ( 'NONE', #25428, 1000.000000000000000 ) ;
#1788 = FACE_OUTER_BOUND ( 'NONE', #20620, .T. ) ;
#1789 = CARTESIAN_POINT ( 'NONE',  ( 3.499999999999999556, 0.000000000000000000, 0.000000000000000000 ) ) ;
#1790 = LOCAL_TIME ( 16, 7, 10.00000000000000000, #24717 ) ;
#1791 = ORIENTED_EDGE ( 'NONE', *, *, #12541, .F. ) ;
#1792 = CARTESIAN_POINT ( 'NONE',  ( -1.444447458290426890E-30, -1.659765939693074585E-14, 4.753758587302147731 ) ) ;
#1793 = CARTESIAN_POINT ( 'NONE',  ( 56.97280603064898941, -277.2763395528616002, -5.471072653611070535 ) ) ;
#1794 = ADVANCED_FACE ( 'NONE', ( #8029 ), #364, .T. ) ;
#1795 = ORIENTED_EDGE ( 'NONE', *, *, #13088, .F. ) ;
#1796 = CARTESIAN_POINT ( 'NONE',  ( 18.46877649744746819, -16.82957494019613520, 1.753327325565563921 ) ) ;
#1797 = COORDINATED_UNIVERSAL_TIME_OFFSET ( 0, 0, .AHEAD. ) ;
#1799 = EDGE_CURVE ( 'NONE', #15924, #27103, #20883, .T. ) ;
#1798 = CARTESIAN_POINT ( 'NONE',  ( 107.3476768466457401, -15.88628154573096651, 1.500000000000000000 ) ) ;
#1800 = EDGE_LOOP ( 'NONE', ( #30781, #31477, #20672, #13523 ) ) ;
#1801 = CARTESIAN_POINT ( 'NONE',  ( -4.181783187175765804, -9.389479943443376442, 1.500000000000000000 ) ) ;
#1802 = CARTESIAN_POINT ( 'NONE',  ( 10.49234587624072290, 2.036894776009066987, -1.050000000000000044 ) ) ;
#1803 = AXIS2_PLACEMENT_3D ( 'NONE', #12447, #22662, #7414 ) ;
#1804 = CARTESIAN_POINT ( 'NONE',  ( 102.4008411508948768, -3.675699656443788044, -4.275175836096084758 ) ) ;
#1805 = CARTESIAN_POINT ( 'NONE',  ( 5.489321486716459475, -1.512021494499641294, 7.976795196726682136 ) ) ;
#1806 = LINE ( 'NONE', #32733, #32147 ) ;
#1807 = AXIS2_PLACEMENT_3D ( 'NONE', #3221, #28474, #5081 ) ;
#1808 = ORIENTED_EDGE ( 'NONE', *, *, #19732, .T. ) ;
#1809 = EDGE_CURVE ( 'NONE', #18943, #32789, #31602, .T. ) ;
#1810 = VECTOR ( 'NONE', #18847, 1000.000000000000000 ) ;
#1811 = CARTESIAN_POINT ( 'NONE',  ( -3.222375984151269357, 0.000000000000000000, 1.000000000000000000 ) ) ;
#1812 = CARTESIAN_POINT ( 'NONE',  ( 23.22050010672911569, -21.93619796768840047, -1.062839084286906211 ) ) ;
#1813 = AXIS2_PLACEMENT_3D ( 'NONE', #13429, #5274, #23649 ) ;
#1814 = DIRECTION ( 'NONE',  ( 3.469446951953478110E-15, 1.087146173449926665E-32, -1.000000000000000000 ) ) ;
#1815 = AXIS2_PLACEMENT_3D ( 'NONE', #11513, #13677, #21554 ) ;
#1817 = ORIENTED_EDGE ( 'NONE', *, *, #10529, .F. ) ;
#1816 = FACE_OUTER_BOUND ( 'NONE', #25502, .T. ) ;
#1818 = CARTESIAN_POINT ( 'NONE',  ( 6.038144483126824724, -8.463061282283012687, -0.4487862922133540877 ) ) ;
#1819 = LINE ( 'NONE', #13986, #16551 ) ;
#1820 = CARTESIAN_POINT ( 'NONE',  ( -10.00000000000000000, 0.000000000000000000, 0.000000000000000000 ) ) ;
#1821 = EDGE_CURVE ( 'NONE', #11829, #4589, #18560, .T. ) ;
#1822 = DIRECTION ( 'NONE',  ( 0.000000000000000000, 1.000000000000000000, 0.000000000000000000 ) ) ;
#1823 = FACE_OUTER_BOUND ( 'NONE', #30371, .T. ) ;
#1824 = PRODUCT_DEFINITION_FORMATION_WITH_SPECIFIED_SOURCE ( 'ANY', '', #4694, .NOT_KNOWN. ) ;
#1825 = CARTESIAN_POINT ( 'NONE',  ( 5.885541416630537093, 0.3712256868992431236, 8.385500676968929312 ) ) ;
#1826 = CARTESIAN_POINT ( 'NONE',  ( 25.38257154049698272, -17.53428803818666992, -1.078154016645389790 ) ) ;
#1827 = FACE_OUTER_BOUND ( 'NONE', #29736, .T. ) ;
#1828 = CARTESIAN_POINT ( 'NONE',  ( -24.00194742982113638, 3.998227953278373992, 2.146185852361368607 ) ) ;
#1829 = ORIENTED_EDGE ( 'NONE', *, *, #18613, .T. ) ;
#1830 = EDGE_CURVE ( 'NONE', #1536, #7257, #16371, .T. ) ;
#1831 = CARTESIAN_POINT ( 'NONE',  ( 10.55147673363119232, 4.208382051008229929, -2.718385644597129502 ) ) ;
#1832 = ORIENTED_EDGE ( 'NONE', *, *, #14959, .F. ) ;
#1833 = CARTESIAN_POINT ( 'NONE',  ( -8.054531657079158080, -1.545410377633946286, 2.846291840500174697 ) ) ;
#1834 = AXIS2_PLACEMENT_3D ( 'NONE', #1634, #11654, #6964 ) ;
#1835 = CARTESIAN_POINT ( 'NONE',  ( 101.6441386174529953, -1.774168274679931212, 2.184956718805492581 ) ) ;
#1836 = CIRCLE ( 'NONE', #20524, 10.94895958125474245 ) ;
#1837 = CARTESIAN_POINT ( 'NONE',  ( 69.18703749905368738, -4.112663945007549060, -4.522129901861162260 ) ) ;
#1838 = EDGE_CURVE ( 'NONE', #7133, #16940, #6477, .T. ) ;
#1839 = CARTESIAN_POINT ( 'NONE',  ( 2.661997850953047973, 8.696442646092101825, -5.196702353893110526 ) ) ;
#1840 = CARTESIAN_POINT ( 'NONE',  ( 2.342933509396896152, -0.1895978275999587181, 1.757325986342921587 ) ) ;
#1841 = EDGE_LOOP ( 'NONE', ( #15800, #19619, #650, #24516 ) ) ;
#1842 = FACE_OUTER_BOUND ( 'NONE', #18102, .T. ) ;
#1843 = EDGE_CURVE ( 'NONE', #9763, #13750, #19058, .T. ) ;
#1844 = ORIENTED_EDGE ( 'NONE', *, *, #26197, .F. ) ;
#1845 = CALENDAR_DATE ( 2026, 6, 10 ) ;
#1847 = CARTESIAN_POINT ( 'NONE',  ( 28.66420361012185936, -6.761305300330741730, 3.999773682894746774 ) ) ;
#1846 = LOCAL_TIME ( 16, 7, 10.00000000000000000, #10782 ) ;
#1848 = EDGE_CURVE ( 'NONE', #30559, #10039, #18747, .T. ) ;
#1849 = CARTESIAN_POINT ( 'NONE',  ( 10.00000000000000178, -3.024842911000664269, -3.993798362933342894 ) ) ;
#1851 = DIRECTION ( 'NONE',  ( 0.000000000000000000, 0.5735764363510594821, -0.8191520442889824727 ) ) ;
#1850 = CARTESIAN_POINT ( 'NONE',  ( 7.249760686538667009, 3.748318449932293905, 7.906491560603678082 ) ) ;
#1852 = VERTEX_POINT ( 'NONE', #11038 ) ;
#1853 = ORIENTED_EDGE ( 'NONE', *, *, #21991, .T. ) ;
#1854 = CARTESIAN_POINT ( 'NONE',  ( 6.357668022120092743, 6.210015626210386053, 5.959864878090697538 ) ) ;
#1855 = DIRECTION ( 'NONE',  ( 0.000000000000000000, 0.000000000000000000, -1.000000000000000000 ) ) ;
#1856 = CARTESIAN_POINT ( 'NONE',  ( 23.29750000000000654, -0.7685399846772070775, 2.594547506269381465 ) ) ;
#1857 = ADVANCED_FACE ( 'NONE', ( #24049 ), #21574, .T. ) ;
#1858 = CARTESIAN_POINT ( 'NONE',  ( 1.563235467773296250, -10.39397044182024921, -1.763951029879659460 ) ) ;
#1860 = ORIENTED_EDGE ( 'NONE', *, *, #25337, .T. ) ;
#1859 = DIRECTION ( 'NONE',  ( 1.000000000000000000, -8.574039729943018344E-17, -0.000000000000000000 ) ) ;
#1861 = VECTOR ( 'NONE', #23980, 1000.000000000000000 ) ;
#1862 = CARTESIAN_POINT ( 'NONE',  ( -4.387550801365594388, -3.521866450007987037, -0.3701630799359323931 ) ) ;
#1863 = LINE ( 'NONE', #21887, #1648 ) ;
#1864 = CARTESIAN_POINT ( 'NONE',  ( 1.624999999999999778, -1.464956435139619151, 10.90201369670498366 ) ) ;
#1865 = DIRECTION ( 'NONE',  ( -1.000000000000000000, 0.000000000000000000, 0.000000000000000000 ) ) ;
#1866 = ORIENTED_EDGE ( 'NONE', *, *, #5979, .F. ) ;
#1868 = ORIENTED_EDGE ( 'NONE', *, *, #5727, .T. ) ;
#1867 = LINE ( 'NONE', #14533, #23003 ) ;
#1869 = ADVANCED_FACE ( 'NONE', ( #861 ), #16027, .T. ) ;
#1870 = CARTESIAN_POINT ( 'NONE',  ( 107.3934790618724406, 17.60822615140890335, 4.091707453491133961 ) ) ;
#1871 = DIRECTION ( 'NONE',  ( -3.623545766764218936E-17, -0.4226182617406998854, -0.9063077870366498257 ) ) ;
#1872 = EDGE_CURVE ( 'NONE', #30338, #9983, #20082, .T. ) ;
#1873 = CARTESIAN_POINT ( 'NONE',  ( 24.92250000136559507, 0.3178988483021036315, 3.024605502323848949 ) ) ;
#1874 = DIRECTION ( 'NONE',  ( -1.000000000000000000, 8.574039729943017111E-17, -0.000000000000000000 ) ) ;
#1875 = CARTESIAN_POINT ( 'NONE',  ( 2.226843223301624430, -16.57429286563273862, -1.499999999999679146 ) ) ;
#1876 = CARTESIAN_POINT ( 'NONE',  ( 24.75111450864415730, -6.623356326098185375E-16, -2.499999999999998224 ) ) ;
#1877 = EDGE_CURVE ( 'NONE', #5412, #4370, #16219, .T. ) ;
#1878 = CARTESIAN_POINT ( 'NONE',  ( 41.34499449510862235, -4.297820755683611438, 1.873789611272388189 ) ) ;
#1879 = DIRECTION ( 'NONE',  ( 0.000000000000000000, 0.000000000000000000, 1.000000000000000000 ) ) ;
#1880 = ORIENTED_EDGE ( 'NONE', *, *, #2324, .T. ) ;
#1881 = LINE ( 'NONE', #19431, #27332 ) ;
#1882 = ORIENTED_EDGE ( 'NONE', *, *, #12809, .T. ) ;
#1883 = EDGE_CURVE ( 'NONE', #9751, #2084, #25940, .T. ) ;
#1884 = TOROIDAL_SURFACE ( 'NONE', #287, 6.923700951379997193, 9.000000000000000000 ) ;
#1885 = FACE_OUTER_BOUND ( 'NONE', #29245, .T. ) ;
#1886 = SHAPE_REPRESENTATION_RELATIONSHIP ( 'NONE' , 'NONE' ,  #13, #11140 ) ;
#1887 = CARTESIAN_POINT ( 'NONE',  ( 23.90742340929273624, -3.204431202270332513, -2.713652344655542503 ) ) ;
#1888 = DIRECTION ( 'NONE',  ( -1.000000000000000000, 0.000000000000000000, 0.000000000000000000 ) ) ;
#1889 = ORIENTED_EDGE ( 'NONE', *, *, #18735, .T. ) ;
#1890 = DIRECTION ( 'NONE',  ( -1.000000000000000000, -0.000000000000000000, 0.000000000000000000 ) ) ;
#1891 = VERTEX_POINT ( 'NONE', #3537 ) ;
#1892 = CARTESIAN_POINT ( 'NONE',  ( -7.000050800000000351, 0.000000000000000000, 0.000000000000000000 ) ) ;
#1894 = ORIENTED_EDGE ( 'NONE', *, *, #31040, .F. ) ;
#1893 = CARTESIAN_POINT ( 'NONE',  ( 28.69353846085885706, -5.618139531230570860, -3.997238537426948568 ) ) ;
#1895 = ORIENTED_EDGE ( 'NONE', *, *, #20380, .T. ) ;
#1896 = CARTESIAN_POINT ( 'NONE',  ( 2.492101788275272067, -9.149023314703491394, 5.239665997526232744 ) ) ;
#1897 = EDGE_CURVE ( 'NONE', #10078, #7472, #22848, .T. ) ;
#1898 = CARTESIAN_POINT ( 'NONE',  ( 19.10390797508228999, -2.015740111943971957, 1.010822989962091301 ) ) ;
#1899 = PRODUCT_DEFINITION ( 'UNKNOWN', '', #4466, #24870 ) ;
#1901 = ORIENTED_EDGE ( 'NONE', *, *, #24305, .T. ) ;
#1900 = DIRECTION ( 'NONE',  ( 8.281886410780504864E-17, 0.9659258262890672020, 0.2588190451025252359 ) ) ;
#1902 = CARTESIAN_POINT ( 'NONE',  ( 23.22564588060097890, -22.38932300456763969, 1.000000000000000000 ) ) ;
#1903 = CYLINDRICAL_SURFACE ( 'NONE', #9030, 3.000000000000000444 ) ;
#1904 = FACE_OUTER_BOUND ( 'NONE', #28144, .T. ) ;
#1905 = CARTESIAN_POINT ( 'NONE',  ( 2.661997913519439596, 9.876677602395393052, -2.255009087902827503 ) ) ;
#1907 = EDGE_LOOP ( 'NONE', ( #20317, #8545, #22276, #29830 ) ) ;
#1906 = CARTESIAN_POINT ( 'NONE',  ( 107.9489733406790037, -17.33459091623378256, -4.544509996648006478 ) ) ;
#1908 = DIRECTION ( 'NONE',  ( 1.000000000000000000, -8.574039729943018344E-17, -0.000000000000000000 ) ) ;
#1909 = FACE_OUTER_BOUND ( 'NONE', #30106, .T. ) ;
#1910 = DIRECTION ( 'NONE',  ( 1.000000000000000000, 0.000000000000000000, 0.000000000000000000 ) ) ;
#1911 = EDGE_CURVE ( 'NONE', #25076, #31964, #6186, .T. ) ;
#1912 = CYLINDRICAL_SURFACE ( 'NONE', #11887, 4.000000000000002665 ) ;
#1913 = DIRECTION ( 'NONE',  ( 1.000000000000000000, 0.000000000000000000, 0.000000000000000000 ) ) ;
#1914 = CARTESIAN_POINT ( 'NONE',  ( 10.55147673363119054, 4.208382051008190849, 2.718385644597189454 ) ) ;
#1915 = ORIENTED_EDGE ( 'NONE', *, *, #1566, .F. ) ;
#1916 = CARTESIAN_POINT ( 'NONE',  ( -34.48223484310472031, 0.5000000000000000000, 2.552009564962238741 ) ) ;
#1917 = EDGE_CURVE ( 'NONE', #3400, #22947, #4520, .T. ) ;
#1918 = CARTESIAN_POINT ( 'NONE',  ( -3.683682291401270757E-13, 9.884132761439586190, -4.709950686175258916 ) ) ;
#1919 = CARTESIAN_POINT ( 'NONE',  ( -5.287550801365593856, -2.752080473201636845, 2.228590825266444586 ) ) ;
#1920 = ORIENTED_EDGE ( 'NONE', *, *, #26984, .F. ) ;
#1921 =( BOUNDED_CURVE ( )  B_SPLINE_CURVE ( 3, ( #9458, #9808, #2117, #12297 ),
 .UNSPECIFIED., .F., .F. ) 
 B_SPLINE_CURVE_WITH_KNOTS ( ( 4, 4 ),
 ( 3.141592653589800221, 3.761815862121093090 ),
 .UNSPECIFIED. ) 
 CURVE ( )  GEOMETRIC_REPRESENTATION_ITEM ( )  RATIONAL_B_SPLINE_CURVE ( ( 1.000000000000000000, 0.9681996787398556847, 0.9681996787398556847, 1.000000000000000000 ) ) 
 REPRESENTATION_ITEM ( '' )  );
#1922 = DIRECTION ( 'NONE',  ( 1.000000000000000000, -0.000000000000000000, 0.000000000000000000 ) ) ;
#1923 = CARTESIAN_POINT ( 'NONE',  ( 2.913020537602763582, 0.09936728819754167552, -1.050862340634153291 ) ) ;
#1924 = ORIENTED_EDGE ( 'NONE', *, *, #4851, .T. ) ;
#1925 = DIRECTION ( 'NONE',  ( 0.000000000000000000, -1.000000000000000000, 0.000000000000000000 ) ) ;
#1926 = EDGE_LOOP ( 'NONE', ( #4636, #2359, #17058, #4963 ) ) ;
#1927 = ORIENTED_EDGE ( 'NONE', *, *, #22837, .T. ) ;
#1928 = PLANE ( 'NONE',  #20947 ) ;
#1930 = ORIENTED_EDGE ( 'NONE', *, *, #13371, .T. ) ;
#1929 = CARTESIAN_POINT ( 'NONE',  ( 5.612974044843318744, -8.123783100924557132, 1.229732182294874354 ) ) ;
#1931 = ORIENTED_EDGE ( 'NONE', *, *, #14870, .F. ) ;
#1932 = CARTESIAN_POINT ( 'NONE',  ( 22.48500000136559507, 2.892927487894327410, -1.570731468192931635 ) ) ;
#1933 = VERTEX_POINT ( 'NONE', #32095 ) ;
#1934 = B_SPLINE_CURVE_WITH_KNOTS ( 'NONE', 3,
 ( #23308, #18286, #12930, #12754, #18459, #10932, #13251, #20794, #28498, #22959 ),
 .UNSPECIFIED., .F., .F.,
 ( 4, 3, 3, 4 ),
 ( 0.000000000000000000, 0.0005351973326734103635, 0.001070394665346820727, 0.002130599681840938692 ),
 .UNSPECIFIED. ) ;
#1935 = CARTESIAN_POINT ( 'NONE',  ( -83.35439080561378944, -0.0003384977252891612984, 1.500000000000000000 ) ) ;
#1937 = ORIENTED_EDGE ( 'NONE', *, *, #28996, .F. ) ;
#1936 = CARTESIAN_POINT ( 'NONE',  ( 29.31981545345093920, -4.303267367677382715, -2.184956339556331173 ) ) ;
#1938 = CARTESIAN_POINT ( 'NONE',  ( -56.35387370928786765, 0.005482903227124292372, -1.004960936152643702 ) ) ;
#1939 = CARTESIAN_POINT ( 'NONE',  ( 4.749760686538667009, -5.151476664237435443, -6.139290821770307716 ) ) ;
#1940 = CARTESIAN_POINT ( 'NONE',  ( 22.61000000136559507, 3.156283516753366047, 0.9349337715887203748 ) ) ;
#1941 = CARTESIAN_POINT ( 'NONE',  ( 108.0981717737594749, -19.48301123669095247, 2.289311975388307108 ) ) ;
#1942 = CARTESIAN_POINT ( 'NONE',  ( -1.921189184902703406, -10.44034746380417289, -4.522129901861166701 ) ) ;
#1943 = CARTESIAN_POINT ( 'NONE',  ( 1.624999999999999778, -7.958834565716711218, -7.593217523260671342 ) ) ;
#1944 = EDGE_CURVE ( 'NONE', #30369, #3680, #23277, .T. ) ;
#1945 = ADVANCED_FACE ( 'NONE', ( #14025 ), #12426, .F. ) ;
#1946 = DIRECTION ( 'NONE',  ( -1.000000000000000000, 0.000000000000000000, 0.000000000000000000 ) ) ;
#1947 = CARTESIAN_POINT ( 'NONE',  ( -1.824298235657122902, -2.866444442092977329, 5.485967528433935314 ) ) ;
#1948 = DIRECTION ( 'NONE',  ( 0.000000000000000000, 0.5877852522924689183, 0.8090169943749504489 ) ) ;
#1949 = CARTESIAN_POINT ( 'NONE',  ( -23.54713438637982748, 10.71031731502107576, 2.573304945315896042 ) ) ;
#1950 = ADVANCED_FACE ( 'NONE', ( #32435 ), #9666, .F. ) ;
#1951 = CARTESIAN_POINT ( 'NONE',  ( 29.25343337322282622, -7.426690278353109242, 4.522129901861163148 ) ) ;
#1952 = CARTESIAN_POINT ( 'NONE',  ( -6.000050802731188959, 3.113457007523260156, -0.9222479816126439855 ) ) ;
#1953 = ORIENTED_EDGE ( 'NONE', *, *, #10639, .F. ) ;
#1954 = CARTESIAN_POINT ( 'NONE',  ( -3.200050800000000528, -2.331437884370912705, 1.887961173149512062 ) ) ;
#1955 = B_SPLINE_CURVE_WITH_KNOTS ( 'NONE', 3,
 ( #8617, #32022, #16455, #19322, #19144, #21182, #9092, #23983, #3775, #26663 ),
 .UNSPECIFIED., .F., .F.,
 ( 4, 2, 2, 2, 4 ),
 ( 1.968338519012340988E-07, 0.0005467927057105487470, 0.001093388577569196288, 0.001639984449427843395, 0.002186580321286490502 ),
 .UNSPECIFIED. ) ;
#1956 = CARTESIAN_POINT ( 'NONE',  ( 107.1769020805352142, 16.40214705320008903, -1.491740999229418829 ) ) ;
#1957 = CYLINDRICAL_SURFACE ( 'NONE', #17789, 0.5000000000000000000 ) ;
#1958 = EDGE_LOOP ( 'NONE', ( #5140, #30611, #5689, #10172 ) ) ;
#1959 = LINE ( 'NONE', #11981, #24534 ) ;
#1960 = DIRECTION ( 'NONE',  ( -1.000000000000000000, 0.000000000000000000, 0.000000000000000000 ) ) ;
#1961 = ORIENTED_EDGE ( 'NONE', *, *, #28424, .F. ) ;
#1962 = CARTESIAN_POINT ( 'NONE',  ( 12.13210218395027162, -15.56661508947843764, 1.754034462302825892 ) ) ;
#1963 = CALENDAR_DATE ( 2026, 6, 10 ) ;
#1964 = CARTESIAN_POINT ( 'NONE',  ( 25.98690466878739613, 22.56136012750964426, -0.4463807625373771293 ) ) ;
#1965 = ORIENTED_EDGE ( 'NONE', *, *, #32430, .T. ) ;
#1966 = CYLINDRICAL_SURFACE ( 'NONE', #614, 0.5000000000000000000 ) ;
#1967 = DIRECTION ( 'NONE',  ( -0.1027947991993876792, 0.9947025833170222153, 0.000000000000000000 ) ) ;
#1968 = CARTESIAN_POINT ( 'NONE',  ( 85.00835009346432969, -4.756612885510127953, -4.312042181587000478 ) ) ;
#1969 = LINE ( 'NONE', #17339, #20889 ) ;
#1970 = CYLINDRICAL_SURFACE ( 'NONE', #27252, 5.010000000000000675 ) ;
#1971 = VERTEX_POINT ( 'NONE', #27224 ) ;
#1972 = CARTESIAN_POINT ( 'NONE',  ( 23.25968158267518149, -21.94039639562157618, -1.058068363327190564 ) ) ;
#1973 = CARTESIAN_POINT ( 'NONE',  ( 10.00000000000000000, -0.8254815157535575487, 4.681538312723514395 ) ) ;
#1974 = ADVANCED_FACE ( 'NONE', ( #16709 ), #24540, .F. ) ;
#1976 = ORIENTED_EDGE ( 'NONE', *, *, #21065, .F. ) ;
#1975 = CYLINDRICAL_SURFACE ( 'NONE', #32083, 8.500000000000000000 ) ;
#1977 = CARTESIAN_POINT ( 'NONE',  ( 0.000000000000000000, 0.000000000000000000, 0.000000000000000000 ) ) ;
#1978 = CARTESIAN_POINT ( 'NONE',  ( 85.08949032934708612, -1.315411135598755221, 0.07017451552781951707 ) ) ;
#1979 = CARTESIAN_POINT ( 'NONE',  ( -4.300050802731187005, 2.853674364686379583, 1.549418761218565921 ) ) ;
#1980 = CARTESIAN_POINT ( 'NONE',  ( 4.013969549054183686E-16, 4.681538312723517059, 0.8254815157535410064 ) ) ;
#1981 = DIRECTION ( 'NONE',  ( 0.000000000000000000, 0.000000000000000000, -1.000000000000000000 ) ) ;
#1982 = DIRECTION ( 'NONE',  ( 0.000000000000000000, 0.000000000000000000, 1.000000000000000000 ) ) ;
#1983 = CARTESIAN_POINT ( 'NONE',  ( 24.54848581754903236, -17.37474206563366508, -1.294224261558855060 ) ) ;
#1984 = CARTESIAN_POINT ( 'NONE',  ( -23.35000000000000142, -10.96966150227469505, -11.50000000000000000 ) ) ;
#1985 = DIRECTION ( 'NONE',  ( -0.9873162094019954926, 0.1587661886299326364, 1.242416025591495175E-13 ) ) ;
#1986 = ORIENTED_EDGE ( 'NONE', *, *, #21805, .T. ) ;
#1987 = LINE ( 'NONE', #32417, #24169 ) ;
#1988 = ORIENTED_EDGE ( 'NONE', *, *, #16813, .T. ) ;
#1989 = CARTESIAN_POINT ( 'NONE',  ( -5.354531657079158791, -0.9198621039125872700, -3.105402419394638791 ) ) ;
#1990 = CARTESIAN_POINT ( 'NONE',  ( 25.17250000136559507, -3.024605502323851169, 0.3178988483021052969 ) ) ;
#1991 = CARTESIAN_POINT ( 'NONE',  ( 69.29300722455955963, -6.224615717686389438, -5.695980980372493008 ) ) ;
#1992 = CARTESIAN_POINT ( 'NONE',  ( 3.499999999999999556, -4.147285340411824173, 5.698247474649390298 ) ) ;
#1993 = DIRECTION ( 'NONE',  ( 0.000000000000000000, 0.000000000000000000, 1.000000000000000000 ) ) ;
#1994 = VERTEX_POINT ( 'NONE', #19713 ) ;
#1995 = DIRECTION ( 'NONE',  ( 0.000000000000000000, 1.000000000000000000, 0.000000000000000000 ) ) ;
#1996 = ORIENTED_EDGE ( 'NONE', *, *, #9439, .T. ) ;
#1997 = PERSON_AND_ORGANIZATION ( #6766, #25292 ) ;
#1998 = ADVANCED_FACE ( 'NONE', ( #29753 ), #10831, .T. ) ;
#1999 = CARTESIAN_POINT ( 'NONE',  ( 69.06996892930607146, -6.106740143811350663, 4.008637876655180676 ) ) ;
#2000 = CARTESIAN_POINT ( 'NONE',  ( -56.29198263848482497, 0.01337210975256776860, -1.132057944610920686 ) ) ;
#2002 = CARTESIAN_POINT ( 'NONE',  ( 5.489343555808770425, -0.1039150536217892384, -8.118190043691532409 ) ) ;
#2001 = DIRECTION ( 'NONE',  ( 0.000000000000000000, -0.8191520442889993481, 0.5735764363510352792 ) ) ;
#2003 = ADVANCED_FACE ( 'NONE', ( #19893 ), #22068, .T. ) ;
#2004 = ORIENTED_EDGE ( 'NONE', *, *, #27657, .F. ) ;
#2005 = CARTESIAN_POINT ( 'NONE',  ( 5.377543748152551650, 6.139290821770257089, 5.151476664237498504 ) ) ;
#2006 = CARTESIAN_POINT ( 'NONE',  ( 2.857987933988744622, 9.536462466408302419, -0.6743480930095767656 ) ) ;
#2007 = CARTESIAN_POINT ( 'NONE',  ( 23.67250000136559507, 3.024605502323846729, -0.3178988483021056854 ) ) ;
#2008 = CARTESIAN_POINT ( 'NONE',  ( 0.2521526662550623299, -7.034850097465708885, -1.499999999999965139 ) ) ;
#2010 = ORIENTED_EDGE ( 'NONE', *, *, #7749, .F. ) ;
#2009 = CARTESIAN_POINT ( 'NONE',  ( 107.5415233712214871, 18.44887242198213073, 5.148260821734984560 ) ) ;
#2011 = CARTESIAN_POINT ( 'NONE',  ( -3.487550801365593589, -2.228590825266444586, -2.752080473201636401 ) ) ;
#2012 = FACE_OUTER_BOUND ( 'NONE', #25615, .T. ) ;
#2013 = CARTESIAN_POINT ( 'NONE',  ( 56.97280603064898941, -277.2763395528616002, -4.612695725900422872 ) ) ;
#2015 = EDGE_CURVE ( 'NONE', #22347, #9445, #22227, .T. ) ;
#2014 = CARTESIAN_POINT ( 'NONE',  ( 21.98499999999999943, 2.486304738420679783, -0.2613211581691337604 ) ) ;
#2016 = EDGE_LOOP ( 'NONE', ( #25355, #28526, #8995 ) ) ;
#2018 = ORIENTED_EDGE ( 'NONE', *, *, #4844, .T. ) ;
#2017 = PLANE ( 'NONE',  #28323 ) ;
#2019 = ADVANCED_FACE ( 'NONE', ( #29912 ), #14335, .F. ) ;
#2020 = CARTESIAN_POINT ( 'NONE',  ( 10.00000000000000178, -8.574039729943018837E-16, 0.000000000000000000 ) ) ;
#2021 = CARTESIAN_POINT ( 'NONE',  ( 6.883866482134012976, 8.452201317944600945, 2.190971798909973067 ) ) ;
#2022 = EDGE_CURVE ( 'NONE', #19954, #15334, #11262, .T. ) ;
#2023 = CARTESIAN_POINT ( 'NONE',  ( 24.54750000136559507, 1.913930629741522838, -2.363507492473150062 ) ) ;
#2024 = CARTESIAN_POINT ( 'NONE',  ( -6.556376981307135310, -0.1572233378491242062, 2.999999999999999556 ) ) ;
#2025 = CARTESIAN_POINT ( 'NONE',  ( 3.379177507580384709, -17.49396809222194094, -1.499999999999999112 ) ) ;
#2026 = CARTESIAN_POINT ( 'NONE',  ( 5.377543748152548986, 8.014274990069656823, -8.669741416787380218E-17 ) ) ;
#2027 = PRODUCT ( 'Part4_Gear', 'Part4_Gear', '', ( #29746 ) ) ;
#2028 = CARTESIAN_POINT ( 'NONE',  ( 23.84149738812723740, -4.050734785762162282, 2.184956778860680959 ) ) ;
#2029 = CARTESIAN_POINT ( 'NONE',  ( 0.000000000000000000, 7.944914065997111585, 7.533794289458081828 ) ) ;
#2030 = ORIENTED_EDGE ( 'NONE', *, *, #23669, .F. ) ;
#2031 = ORIENTED_EDGE ( 'NONE', *, *, #11415, .T. ) ;
#2032 = EDGE_CURVE ( 'NONE', #7398, #5630, #9695, .T. ) ;
#2033 = DIRECTION ( 'NONE',  ( 0.9947025833170223263, 0.1027947991993880261, 0.000000000000000000 ) ) ;
#2034 = CARTESIAN_POINT ( 'NONE',  ( 0.2099999999999758171, 0.0003384977254328180862, -2.168404344971008868E-16 ) ) ;
#2035 = DIRECTION ( 'NONE',  ( -0.1908089953765452484, 0.000000000000000000, 0.9816271834476638647 ) ) ;
#2036 = ORIENTED_EDGE ( 'NONE', *, *, #30254, .T. ) ;
#2037 = FACE_OUTER_BOUND ( 'NONE', #13424, .T. ) ;
#2038 = ORIENTED_EDGE ( 'NONE', *, *, #13264, .T. ) ;
#2039 = PLANE ( 'NONE',  #13486 ) ;
#2041 = ORIENTED_EDGE ( 'NONE', *, *, #12215, .T. ) ;
#2040 = CARTESIAN_POINT ( 'NONE',  ( 28.69343354123121514, -5.622193070524895475, -4.003574682336918933 ) ) ;
#2042 = VERTEX_POINT ( 'NONE', #30411 ) ;
#2043 = CARTESIAN_POINT ( 'NONE',  ( 0.000000000000000000, -7.009698679648281860, -0.7308381473897611613 ) ) ;
#2044 = CARTESIAN_POINT ( 'NONE',  ( -2.794738735352966685, 0.000000000000000000, -1.491740999229417941 ) ) ;
#2046 = ORIENTED_EDGE ( 'NONE', *, *, #9841, .T. ) ;
#2045 = CARTESIAN_POINT ( 'NONE',  ( 10.18192333485687406, -19.96327110613152556, -1.499999999999998890 ) ) ;
#2047 = CARTESIAN_POINT ( 'NONE',  ( 0.000000000000000000, -8.264486777890077462, -4.472189673936872722 ) ) ;
#2048 = CARTESIAN_POINT ( 'NONE',  ( 3.249999999999999556, -8.475820894093002877, 4.057423117305364535 ) ) ;
#2049 = LINE ( 'NONE', #15063, #16097 ) ;
#2050 = EDGE_CURVE ( 'NONE', #29481, #2193, #17690, .T. ) ;
#2051 = FACE_OUTER_BOUND ( 'NONE', #27992, .T. ) ;
#2053 = ORIENTED_EDGE ( 'NONE', *, *, #5956, .F. ) ;
#2052 = CARTESIAN_POINT ( 'NONE',  ( 108.0105747311263258, -18.22163561417639954, -4.627746478616681536 ) ) ;
#2054 = EDGE_CURVE ( 'NONE', #16287, #14398, #28816, .T. ) ;
#2055 = CARTESIAN_POINT ( 'NONE',  ( 2.357329973329929551, -9.815384016743289308, -4.593471141847171424 ) ) ;
#2056 = B_SPLINE_CURVE_WITH_KNOTS ( 'NONE', 3,
 ( #5431, #10944, #26330, #277, #13597, #23802, #915, #30862, #23639, #21292 ),
 .UNSPECIFIED., .F., .F.,
 ( 4, 2, 2, 2, 4 ),
 ( 2.740849916261192663E-07, 0.0005478761651001754851, 0.001095478245208724843, 0.001643080325317274092, 0.002190682405425823341 ),
 .UNSPECIFIED. ) ;
#2057 = CARTESIAN_POINT ( 'NONE',  ( -42.85764933975779201, 24.74387538314362800, -1.050000000000000044 ) ) ;
#2058 = CARTESIAN_POINT ( 'NONE',  ( 23.98500000136559507, -2.892927487894331406, 1.570731468192932301 ) ) ;
#2059 = CARTESIAN_POINT ( 'NONE',  ( 107.6876980308802985, 19.28759250760272437, -4.757993698474195732 ) ) ;
#2060 = DIRECTION ( 'NONE',  ( 0.000000000000000000, 0.000000000000000000, -1.000000000000000000 ) ) ;
#2061 = CARTESIAN_POINT ( 'NONE',  ( -3.135269660805079628, -0.5000000000000013323, -1.500000000000000000 ) ) ;
#2062 = VERTEX_POINT ( 'NONE', #2658 ) ;
#2063 = DIRECTION ( 'NONE',  ( 0.000000000000000000, -0.08715574274766195451, 0.9961946980917452121 ) ) ;
#2064 = CYLINDRICAL_SURFACE ( 'NONE', #13985, 2.999999999999999112 ) ;
#2065 = CARTESIAN_POINT ( 'NONE',  ( -5.587550801365593678, 3.521866450007987037, 0.3701630799359328372 ) ) ;
#2066 = ORIENTED_EDGE ( 'NONE', *, *, #4474, .F. ) ;
#2067 = ADVANCED_FACE ( 'NONE', ( #27903 ), #30598, .T. ) ;
#2068 = PRODUCT_DEFINITION ( 'UNKNOWN', '', #3447, #11579 ) ;
#2069 = DIRECTION ( 'NONE',  ( 0.000000000000000000, 0.000000000000000000, -1.000000000000000000 ) ) ;
#2070 = CARTESIAN_POINT ( 'NONE',  ( 0.000000000000000000, -1.464956435139465052, -10.90201369670500142 ) ) ;
#2071 = ORIENTED_EDGE ( 'NONE', *, *, #26877, .F. ) ;
#2072 = DIRECTION ( 'NONE',  ( -1.000000000000000000, 0.000000000000000000, -0.000000000000000000 ) ) ;
#2073 = ORIENTED_EDGE ( 'NONE', *, *, #10428, .T. ) ;
#2074 = ORIENTED_EDGE ( 'NONE', *, *, #2480, .T. ) ;
#2075 = DIRECTION ( 'NONE',  ( 1.000000000000000000, -8.574039729943018344E-17, -0.000000000000000000 ) ) ;
#2077 = ORIENTED_EDGE ( 'NONE', *, *, #13405, .T. ) ;
#2076 = PLANE ( 'NONE',  #5865 ) ;
#2078 = ORIENTED_EDGE ( 'NONE', *, *, #21914, .F. ) ;
#2079 = CARTESIAN_POINT ( 'NONE',  ( 108.7297614063222113, 16.58428484178599405, -3.222654696952903741 ) ) ;
#2080 = EDGE_CURVE ( 'NONE', #22347, #11908, #19171, .T. ) ;
#2081 = ORIENTED_EDGE ( 'NONE', *, *, #26832, .T. ) ;
#2082 = CARTESIAN_POINT ( 'NONE',  ( 0.7632845268398871230, 8.152713396088806519, -3.174628368995990879 ) ) ;
#2084 = VERTEX_POINT ( 'NONE', #165 ) ;
#2083 = FACE_OUTER_BOUND ( 'NONE', #20688, .T. ) ;
#2085 = CARTESIAN_POINT ( 'NONE',  ( 2.440333710190582650, 2.130583817697960569, -10.46055952248790533 ) ) ;
#2086 = DIRECTION ( 'NONE',  ( -0.03488359650710497195, -0.9989355049964838695, 0.03018263660036222401 ) ) ;
#2087 = CARTESIAN_POINT ( 'NONE',  ( 25.42250000136559507, 1.913930629741522838, -2.363507492473150062 ) ) ;
#2088 = DIRECTION ( 'NONE',  ( -1.000000000000000000, 8.574039729943018344E-17, -3.081487911019577365E-33 ) ) ;
#2089 = DIRECTION ( 'NONE',  ( 1.000000000000000000, 0.000000000000000000, 0.000000000000000000 ) ) ;
#2090 = CARTESIAN_POINT ( 'NONE',  ( 107.9808716746043160, -17.79391898944944117, -4.343976358951705308 ) ) ;
#2091 = DIRECTION ( 'NONE',  ( -0.000000000000000000, -0.000000000000000000, -1.000000000000000000 ) ) ;
#2092 = DIRECTION ( 'NONE',  ( 0.000000000000000000, 0.000000000000000000, 1.000000000000000000 ) ) ;
#2093 = CARTESIAN_POINT ( 'NONE',  ( 29.11693253002209403, -8.303828435806185126, -0.02339150517595086839 ) ) ;
#2094 = CARTESIAN_POINT ( 'NONE',  ( 23.84714171513466141, -3.444070612163574463, -0.07017451552781628354 ) ) ;
#2095 =( BOUNDED_SURFACE ( )  B_SPLINE_SURFACE ( 3, 2, ( 
 ( #24591, #9721, #4394 ),
 ( #14739, #19262, #19947 ),
 ( #22271, #6874, #32642 ),
 ( #1395, #9224, #27462 ),
 ( #27617, #12076, #12222 ),
 ( #14232, #22426, #30155 ) ),
 .UNSPECIFIED., .F., .F., .F. ) 
 B_SPLINE_SURFACE_WITH_KNOTS ( ( 4, 2, 4 ),
 ( 3, 3 ),
 ( 6.884163014324140129, 7.369072324149311015, 7.853981633974482790 ),
 ( 0.000000000000000000, 1.000000000000000000 ),
 .UNSPECIFIED. ) 
 GEOMETRIC_REPRESENTATION_ITEM ( )  RATIONAL_B_SPLINE_SURFACE ( (
 ( 1.000000000000000000, 0.8123215895924605912, 1.000000000000000000),
 ( 1.000000000000000000, 0.8591172521900167780, 1.000000000000000000),
 ( 1.000000000000000000, 0.9088222585364039707, 1.000000000000000000),
 ( 1.000000000000000000, 0.9794174349135039703, 1.000000000000000000),
 ( 1.000000000000000000, 1.000375673120272202, 1.000000000000000000),
 ( 1.000000000000000000, 1.000000000000000000, 1.000000000000000000) ) ) 
 REPRESENTATION_ITEM ( '' )  SURFACE ( )  );
#2096 = CARTESIAN_POINT ( 'NONE',  ( -38.14293509397969473, 10.97000000000000419, -1.050000000000000044 ) ) ;
#2097 = CARTESIAN_POINT ( 'NONE',  ( -2.550050802731187005, -0.3135853898029607456, 2.983565686104819648 ) ) ;
#2098 = EDGE_LOOP ( 'NONE', ( #27076, #14372 ) ) ;
#2099 = CARTESIAN_POINT ( 'NONE',  ( -3.600050800000000883, 2.331437884370912705, -1.887961173149511618 ) ) ;
#2100 = CARTESIAN_POINT ( 'NONE',  ( 0.1574692293610879257, 4.391622967208396844, 9.672096048330979912 ) ) ;
#2101 = CARTESIAN_POINT ( 'NONE',  ( -4.512942406915326998, 4.884725290497410777E-15, -2.999999999999999556 ) ) ;
#2102 = EDGE_LOOP ( 'NONE', ( #6416, #17791, #19276, #30267 ) ) ;
#2103 = DIRECTION ( 'NONE',  ( 0.9896144216807899463, 8.678901113238557421E-19, 0.1437473352845038133 ) ) ;
#2104 = DIRECTION ( 'NONE',  ( 1.000000000000000000, 0.000000000000000000, 0.000000000000000000 ) ) ;
#2105 = VERTEX_POINT ( 'NONE', #12524 ) ;
#2106 = B_SPLINE_CURVE_WITH_KNOTS ( 'NONE', 3,
 ( #33010, #30505, #2586, #21131, #24099, #554, #23936, #25983, #21277, #8741 ),
 .UNSPECIFIED., .F., .F.,
 ( 4, 3, 3, 4 ),
 ( 0.000000000000000000, 0.0005352520061641840221, 0.001070504012328368695, 0.002130599681840939126 ),
 .UNSPECIFIED. ) ;
#2107 = CARTESIAN_POINT ( 'NONE',  ( 9.015741301869967472, -14.64812015776037235, 1.754831107654766909 ) ) ;
#2108 = DATE_AND_TIME ( #20513, #23733 ) ;
#2109 = CARTESIAN_POINT ( 'NONE',  ( -10.00000000000000000, 0.000000000000000000, 0.000000000000000000 ) ) ;
#2110 = ORIENTED_EDGE ( 'NONE', *, *, #22872, .T. ) ;
#2111 = CARTESIAN_POINT ( 'NONE',  ( 4.749760686538667009, -4.007137495034861274, 6.940565734314584567 ) ) ;
#2112 = ADVANCED_FACE ( 'NONE', ( #23228, #10351 ), #9853, .T. ) ;
#2113 = EDGE_CURVE ( 'NONE', #9966, #24417, #15124, .T. ) ;
#2114 = ORIENTED_EDGE ( 'NONE', *, *, #12286, .T. ) ;
#2115 = CARTESIAN_POINT ( 'NONE',  ( -3.122314033877847442E-16, -3.641590349731908649, -3.055657119358837992 ) ) ;
#2116 = CARTESIAN_POINT ( 'NONE',  ( 9.288464280921653327, 0.2259206803923255180, -1.047120714225419524 ) ) ;
#2117 = CARTESIAN_POINT ( 'NONE',  ( -56.78550605763575732, 0.5559970271814609344, 1.681829461946841908 ) ) ;
#2118 = CARTESIAN_POINT ( 'NONE',  ( 107.4811544939907293, -15.87715700148073239, -1.499966567242897009 ) ) ;
#2119 = EDGE_CURVE ( 'NONE', #23619, #22462, #4826, .T. ) ;
#2120 = VERTEX_POINT ( 'NONE', #25227 ) ;
#2121 = DIRECTION ( 'NONE',  ( 0.000000000000000000, 0.000000000000000000, 1.000000000000000000 ) ) ;
#2122 = CARTESIAN_POINT ( 'NONE',  ( 110.6444052656891159, 21.58830278953162107, -0.4463807625373413246 ) ) ;
#2124 = ORIENTED_EDGE ( 'NONE', *, *, #16433, .T. ) ;
#2123 = CARTESIAN_POINT ( 'NONE',  ( -3.300050802731187449, -1.549418761218565255, 2.853674364686380471 ) ) ;
#2125 = CARTESIAN_POINT ( 'NONE',  ( 0.000000000000000000, -0.1221666339523235223, -6.247805719894684806 ) ) ;
#2126 = CARTESIAN_POINT ( 'NONE',  ( -1.921189184902703406, -10.44034746380417289, -4.522129901861166701 ) ) ;
#2127 = CARTESIAN_POINT ( 'NONE',  ( -14.63259398290947289, -21.93932300455829676, -0.9045955023117272509 ) ) ;
#2128 = CARTESIAN_POINT ( 'NONE',  ( 10.00000000000000178, -8.574039729943018837E-16, 0.000000000000000000 ) ) ;
#2129 = VECTOR ( 'NONE', #29857, 1000.000000000000000 ) ;
#2130 = CARTESIAN_POINT ( 'NONE',  ( -8.000050799999998574, 2.743648536415450145, 2.018700866895823065 ) ) ;
#2131 = PLANE ( 'NONE',  #10758 ) ;
#2132 = CARTESIAN_POINT ( 'NONE',  ( -56.30179757781805705, 0.05506136597571936742, -1.235259460217722483 ) ) ;
#2133 = DIRECTION ( 'NONE',  ( -1.000000000000000000, -5.361488761196502513E-16, 0.000000000000000000 ) ) ;
#2134 = CIRCLE ( 'NONE', #16517, 0.5000000000000000000 ) ;
#2135 = ORIENTED_EDGE ( 'NONE', *, *, #2417, .T. ) ;
#2136 = CARTESIAN_POINT ( 'NONE',  ( -7.862550801365593145, 3.521866450007987037, 0.3701630799359328372 ) ) ;
#2137 = ORIENTED_EDGE ( 'NONE', *, *, #17572, .F. ) ;
#2138 = CARTESIAN_POINT ( 'NONE',  ( -7.554531657079158968, 3.105402419394639235, -0.9198621039125850496 ) ) ;
#2139 = AXIS2_PLACEMENT_3D ( 'NONE', #26654, #24322, #8930 ) ;
#2140 = CARTESIAN_POINT ( 'NONE',  ( 25.48500000136559862, 0.9349337715887185984, -3.156283516753368268 ) ) ;
#2141 = CARTESIAN_POINT ( 'NONE',  ( 29.27825211595695976, -6.695835137279975591, -5.695980980372493008 ) ) ;
#2142 = CARTESIAN_POINT ( 'NONE',  ( 0.1913146712875998523, -7.518111206453180984, 1.774246272807403768 ) ) ;
#2143 = CARTESIAN_POINT ( 'NONE',  ( 12.44989959798868817, 0.5000000000000000000, 13.00000000000004441 ) ) ;
#2144 = EDGE_LOOP ( 'NONE', ( #32983, #26016, #28137, #342 ) ) ;
#2145 = DIRECTION ( 'NONE',  ( -1.000000000000000000, 0.000000000000000000, 0.000000000000000000 ) ) ;
#2146 = ORIENTED_EDGE ( 'NONE', *, *, #25842, .T. ) ;
#2147 = CARTESIAN_POINT ( 'NONE',  ( 5.612718825656738630, -5.126902779943826260, 6.420171604529170573 ) ) ;
#2148 = APPROVAL_ROLE ( '' ) ;
#2149 = CARTESIAN_POINT ( 'NONE',  ( 18.75975746536424538, -5.862652109951548951, 4.018750267660987419 ) ) ;
#2150 = EDGE_CURVE ( 'NONE', #10646, #11, #7704, .T. ) ;
#2151 = EDGE_CURVE ( 'NONE', #13430, #28488, #2934, .T. ) ;
#2152 = CIRCLE ( 'NONE', #27218, 2.999999999999999112 ) ;
#2153 = FACE_OUTER_BOUND ( 'NONE', #10144, .T. ) ;
#2154 = AXIS2_PLACEMENT_3D ( 'NONE', #7909, #2426, #12917 ) ;
#2156 = DIRECTION ( 'NONE',  ( -1.000000000000000000, 0.000000000000000000, 0.000000000000000000 ) ) ;
#2155 = CARTESIAN_POINT ( 'NONE',  ( 5.887530180601101115, 3.870837198608099161, 7.449245365665808194 ) ) ;
#2157 = VERTEX_POINT ( 'NONE', #23373 ) ;
#2158 = CARTESIAN_POINT ( 'NONE',  ( -8.000050800000003903, -2.956547957031034457, 0.5836481786531007021 ) ) ;
#2159 = CARTESIAN_POINT ( 'NONE',  ( 3.249999999999999556, -4.057423117305452465, 8.475820894092962021 ) ) ;
#2160 = CARTESIAN_POINT ( 'NONE',  ( 23.92250000136559507, 0.3178988483021036315, 3.024605502323848949 ) ) ;
#2161 = CARTESIAN_POINT ( 'NONE',  ( 0.2669967855539195911, -7.206639073886805136, -1.500000000000035083 ) ) ;
#2163 = ORIENTED_EDGE ( 'NONE', *, *, #5095, .T. ) ;
#2162 = CARTESIAN_POINT ( 'NONE',  ( -1.047937531484010476, -4.989690239014954010, 4.522129901861157819 ) ) ;
#2164 = CARTESIAN_POINT ( 'NONE',  ( -2.337550801365593678, 3.368539882008727115, 1.828967928396026954 ) ) ;
#2165 = CARTESIAN_POINT ( 'NONE',  ( 0.000000000000000000, -0.5000000000000000000, 1.000000000000000000 ) ) ;
#2166 = FACE_OUTER_BOUND ( 'NONE', #3125, .T. ) ;
#2167 = PLANE ( 'NONE',  #24609 ) ;
#2168 = ORIENTED_EDGE ( 'NONE', *, *, #24650, .F. ) ;
#2170 = VERTEX_POINT ( 'NONE', #25905 ) ;
#2169 = CARTESIAN_POINT ( 'NONE',  ( -3.078042720788275233, 4.239848598108476807, 5.465019080499222248 ) ) ;
#2171 = B_SPLINE_CURVE_WITH_KNOTS ( 'NONE', 3,
 ( #28398, #16179, #5668, #31402, #648, #28878, #15511, #26060 ),
 .UNSPECIFIED., .F., .F.,
 ( 4, 2, 2, 4 ),
 ( 2.737843117611516695E-07, 0.001261207499628693753, 0.001891674357287160451, 0.002522141214945628450 ),
 .UNSPECIFIED. ) ;
#2172 = DIRECTION ( 'NONE',  ( 0.000000000000000000, 0.4067366430758009299, -0.9135454576426005335 ) ) ;
#2173 = DIRECTION ( 'NONE',  ( 0.000000000000000000, 0.000000000000000000, 1.000000000000000000 ) ) ;
#2174 = AXIS2_PLACEMENT_3D ( 'NONE', #20918, #16378, #6032 ) ;
#2175 = DIRECTION ( 'NONE',  ( 1.000000000000000000, 0.000000000000000000, 0.000000000000000000 ) ) ;
#2176 = CARTESIAN_POINT ( 'NONE',  ( -22.61376412419456727, 18.90773822806010429, 1.500000000000000000 ) ) ;
#2177 = AXIS2_PLACEMENT_3D ( 'NONE', #4127, #19833, #24670 ) ;
#2178 = CARTESIAN_POINT ( 'NONE',  ( -29.27706164892578045, 7.575660699118165198, 1.500000000003544498 ) ) ;
#2179 = CARTESIAN_POINT ( 'NONE',  ( -3.000167615074412097, -11.27277999132675923, -1.743644601730333532 ) ) ;
#2180 = DIRECTION ( 'NONE',  ( 1.000000000000000000, -8.574039729943018344E-17, -0.000000000000000000 ) ) ;
#2181 = CIRCLE ( 'NONE', #20865, 4.499999999999997335 ) ;
#2182 = EDGE_CURVE ( 'NONE', #21075, #3311, #19413, .T. ) ;
#2183 = CARTESIAN_POINT ( 'NONE',  ( 84.86147853070771419, -2.382337935103847393, 0.8105612886933132311 ) ) ;
#2184 = CARTESIAN_POINT ( 'NONE',  ( 107.9497830788478296, -17.34625094442536408, 4.563380564801009065 ) ) ;
#2185 = ORIENTED_EDGE ( 'NONE', *, *, #12245, .F. ) ;
#2186 = DIRECTION ( 'NONE',  ( -0.04852105321274767513, 0.4695180821586621978, -0.8815886103626665582 ) ) ;
#2187 = CIRCLE ( 'NONE', #3270, 0.4999999999999995559 ) ;
#2188 = EDGE_CURVE ( 'NONE', #28886, #9056, #31197, .T. ) ;
#2189 = CARTESIAN_POINT ( 'NONE',  ( 2.864531314636033166, 6.140839842381263125, -7.330015575757827584 ) ) ;
#2190 = EDGE_CURVE ( 'NONE', #25433, #6855, #26216, .T. ) ;
#2191 = ORIENTED_EDGE ( 'NONE', *, *, #14033, .F. ) ;
#2192 = CARTESIAN_POINT ( 'NONE',  ( 107.9275968081481523, 17.77499038371486151, -4.611092782519706113 ) ) ;
#2193 = VERTEX_POINT ( 'NONE', #31562 ) ;
#2194 = CARTESIAN_POINT ( 'NONE',  ( 0.000000000000000000, -7.851777359433977921, -3.255701506262514311 ) ) ;
#2196 = ORIENTED_EDGE ( 'NONE', *, *, #8745, .T. ) ;
#2195 = CARTESIAN_POINT ( 'NONE',  ( 102.3445399775881555, -2.862965201256810310, -4.006107067522454379 ) ) ;
#2197 = VECTOR ( 'NONE', #9590, 1000.000000000000114 ) ;
#2198 = EDGE_CURVE ( 'NONE', #19976, #24335, #6493, .T. ) ;
#2199 = VERTEX_POINT ( 'NONE', #23530 ) ;
#2200 = AXIS2_PLACEMENT_3D ( 'NONE', #31856, #21490, #19303 ) ;
#2201 = DIRECTION ( 'NONE',  ( -1.000000000000000000, 0.000000000000000000, 0.000000000000000000 ) ) ;
#2202 = AXIS2_PLACEMENT_3D ( 'NONE', #7305, #22852, #14974 ) ;
#2203 = DIRECTION ( 'NONE',  ( 1.000000000000000000, 0.000000000000000000, 0.000000000000000000 ) ) ;
#2205 = VERTEX_POINT ( 'NONE', #8646 ) ;
#2204 = LINE ( 'NONE', #15556, #30468 ) ;
#2206 = CARTESIAN_POINT ( 'NONE',  ( 21.09752163284169768, 16.24116300003629121, -1.500000000000059508 ) ) ;
#2207 = VECTOR ( 'NONE', #30222, 1000.000000000000000 ) ;
#2208 = PLANE ( 'NONE',  #10703 ) ;
#2209 = EDGE_CURVE ( 'NONE', #25625, #22238, #27212, .T. ) ;
#2210 = CARTESIAN_POINT ( 'NONE',  ( 9.187365643239731483, 0.07845480144325879535, 1.031721989605144829 ) ) ;
#2211 = CARTESIAN_POINT ( 'NONE',  ( 9.283830569141848343, -0.1241467202047346063, -1.000000000000000000 ) ) ;
#2213 = ORIENTED_EDGE ( 'NONE', *, *, #4011, .F. ) ;
#2212 = CARTESIAN_POINT ( 'NONE',  ( 107.6641398346956890, -20.45810202417174750, -1.499999999999999556 ) ) ;
#2214 = CARTESIAN_POINT ( 'NONE',  ( 2.274274201625313907, -9.915734732513202587, -4.762163868918404930 ) ) ;
#2215 = CIRCLE ( 'NONE', #9128, 10.52000000000000135 ) ;
#2216 = CARTESIAN_POINT ( 'NONE',  ( -60.31029867951531998, -5.485000000000008313, 1.500000000000000222 ) ) ;
#2217 = CARTESIAN_POINT ( 'NONE',  ( 24.79750000136559507, 0.3178988483021036315, 3.024605502323848949 ) ) ;
#2218 = ADVANCED_FACE ( 'NONE', ( #11149 ), #13498, .F. ) ;
#2219 = CARTESIAN_POINT ( 'NONE',  ( 3.249999999999999556, 8.461683424509315543, 2.223716399045601921 ) ) ;
#2220 = CARTESIAN_POINT ( 'NONE',  ( 10.55147673363118876, 2.718385644597232975, -4.208382051008164204 ) ) ;
#2221 = CARTESIAN_POINT ( 'NONE',  ( 12.44989959798868817, 0.000000000000000000, 13.00000000000004441 ) ) ;
#2222 = ORIENTED_EDGE ( 'NONE', *, *, #29350, .T. ) ;
#2223 = PLANE ( 'NONE',  #27907 ) ;
#2224 = EDGE_CURVE ( 'NONE', #22885, #32298, #26393, .T. ) ;
#2225 = AXIS2_PLACEMENT_3D ( 'NONE', #10557, #32835, #7388 ) ;
#2226 = CARTESIAN_POINT ( 'NONE',  ( 2.274274201625327230, 10.90201369670498543, 1.464956435139579183 ) ) ;
#2227 = CARTESIAN_POINT ( 'NONE',  ( -6.737550801365594033, -3.368539882008727115, -1.828967928396027842 ) ) ;
#2228 = ORIENTED_EDGE ( 'NONE', *, *, #31560, .F. ) ;
#2229 = VECTOR ( 'NONE', #30387, 999.9999999999998863 ) ;
#2230 = AXIS2_PLACEMENT_3D ( 'NONE', #28008, #22162, #9936 ) ;
#2231 = CIRCLE ( 'NONE', #23030, 297.9081695149526468 ) ;
#2232 = CARTESIAN_POINT ( 'NONE',  ( 0.000000000000000000, 7.003298780661491918, -4.817032923780496745 ) ) ;
#2233 = CARTESIAN_POINT ( 'NONE',  ( -41.30970132048468457, -16.45499999999997343, 0.000000000000000000 ) ) ;
#2235 = EDGE_CURVE ( 'NONE', #32250, #14334, #11327, .T. ) ;
#2234 = APPLICATION_CONTEXT ( 'configuration controlled 3d designs of mechanical parts and assemblies' ) ;
#2236 = CARTESIAN_POINT ( 'NONE',  ( 3.063284526839887167, 0.000000000000000000, 0.000000000000000000 ) ) ;
#2237 = ORIENTED_EDGE ( 'NONE', *, *, #13779, .T. ) ;
#2239 = CARTESIAN_POINT ( 'NONE',  ( 1.998430852895130228, -1.623920106752339221, -1.500000000000000444 ) ) ;
#2238 = AXIS2_PLACEMENT_3D ( 'NONE', #2944, #16567, #13733 ) ;
#2240 = EDGE_CURVE ( 'NONE', #4740, #32685, #18913, .T. ) ;
#2241 = ORIENTED_EDGE ( 'NONE', *, *, #2988, .T. ) ;
#2242 = VECTOR ( 'NONE', #818, 1000.000000000000000 ) ;
#2243 = VECTOR ( 'NONE', #23041, 1000.000000000000000 ) ;
#2244 = CARTESIAN_POINT ( 'NONE',  ( -41.54586029198078023, -15.55146752323317116, 5.221982333014083544 ) ) ;
#2245 = ORIENTED_EDGE ( 'NONE', *, *, #26632, .T. ) ;
#2246 = DIRECTION ( 'NONE',  ( 0.000000000000000000, -0.4226182617406868403, -0.9063077870366559319 ) ) ;
#2248 = VERTEX_POINT ( 'NONE', #11003 ) ;
#2247 = DIRECTION ( 'NONE',  ( 0.000000000000000000, 0.000000000000000000, -1.000000000000000000 ) ) ;
#2249 = ORIENTED_EDGE ( 'NONE', *, *, #27712, .T. ) ;
#2250 = CYLINDRICAL_SURFACE ( 'NONE', #6459, 2.499999999999997780 ) ;
#2251 = EDGE_CURVE ( 'NONE', #7955, #11449, #29580, .T. ) ;
#2252 = ORIENTED_EDGE ( 'NONE', *, *, #26390, .F. ) ;
#2253 = DIRECTION ( 'NONE',  ( 0.000000000000000000, 0.7071067811865510144, -0.7071067811865441310 ) ) ;
#2255 = EDGE_LOOP ( 'NONE', ( #19539, #23813, #8408, #3849, #9389, #29009, #23566, #16293, #23949, #22491, #18386, #25816, #17016, #5848, #19508 ) ) ;
#2254 = CARTESIAN_POINT ( 'NONE',  ( 41.06247019076344884, -19.55897407381494091, 1.500000000000000000 ) ) ;
#2256 = CARTESIAN_POINT ( 'NONE',  ( -56.56234538287964142, 0.08413247787389122045, -1.028003236817250698 ) ) ;
#2257 = CARTESIAN_POINT ( 'NONE',  ( 2.274274201625315683, -4.762163868918371179, 9.915734732513216798 ) ) ;
#2258 = DIRECTION ( 'NONE',  ( 0.000000000000000000, 0.000000000000000000, 1.000000000000000000 ) ) ;
#2259 = VECTOR ( 'NONE', #30566, 1000.000000000000114 ) ;
#2261 = ADVANCED_FACE ( 'NONE', ( #15700 ), #19173, .T. ) ;
#2260 = VECTOR ( 'NONE', #27159, 1000.000000000000000 ) ;
#2262 = AXIS2_PLACEMENT_3D ( 'NONE', #21932, #22272, #32824 ) ;
#2263 = CARTESIAN_POINT ( 'NONE',  ( 6.530491241813344061, 8.637950316517745364, 0.6236753264480845438 ) ) ;
#2264 = CYLINDRICAL_SURFACE ( 'NONE', #4901, 4.000000000000001776 ) ;
#2265 = CARTESIAN_POINT ( 'NONE',  ( 25.06773407388143582, -17.47416606015757878, 1.197364706238863263 ) ) ;
#2266 = AXIS2_PLACEMENT_3D ( 'NONE', #30921, #28399, #7685 ) ;
#2267 = AXIS2_PLACEMENT_3D ( 'NONE', #19979, #27136, #6902 ) ;
#2268 = CARTESIAN_POINT ( 'NONE',  ( 0.000000000000000000, -1.975651141462165139, -10.82112760146738317 ) ) ;
#2269 = CARTESIAN_POINT ( 'NONE',  ( 35.16139127360178662, -8.400504373793673096, -0.07017451552783579571 ) ) ;
#2270 = CARTESIAN_POINT ( 'NONE',  ( 0.3786097929198382617, 8.648460131863847877, 5.187364053035338429 ) ) ;
#2271 = DIRECTION ( 'NONE',  ( 1.000000000000000000, 0.000000000000000000, 0.000000000000000000 ) ) ;
#2272 = CARTESIAN_POINT ( 'NONE',  ( 85.33608266635168604, -5.304379108986591262, 5.695980980372492120 ) ) ;
#2273 = EDGE_CURVE ( 'NONE', #11269, #32858, #22107, .T. ) ;
#2274 = CARTESIAN_POINT ( 'NONE',  ( -3.150050802731187538, -2.983565686104819648, -0.3135853898029605791 ) ) ;
#2275 = ORIENTED_EDGE ( 'NONE', *, *, #24314, .T. ) ;
#2276 = CARTESIAN_POINT ( 'NONE',  ( -4.250050800000000351, 2.853674364686379583, 1.549418761218565921 ) ) ;
#2277 = AXIS2_PLACEMENT_3D ( 'NONE', #13772, #1089, #32009 ) ;
#2278 = CYLINDRICAL_SURFACE ( 'NONE', #21046, 8.500000000000000000 ) ;
#2279 = ADVANCED_FACE ( 'NONE', ( #17156 ), #23675, .T. ) ;
#2280 = DIRECTION ( 'NONE',  ( 1.000000000000000000, 0.000000000000000000, 0.000000000000000000 ) ) ;
#2282 = ORIENTED_EDGE ( 'NONE', *, *, #3154, .T. ) ;
#2281 = AXIS2_PLACEMENT_3D ( 'NONE', #27471, #23985, #29973 ) ;
#2283 = DIRECTION ( 'NONE',  ( -0.000000000000000000, -0.000000000000000000, 1.000000000000000000 ) ) ;
#2284 = CIRCLE ( 'NONE', #11860, 6.249000000000001442 ) ;
#2285 = CARTESIAN_POINT ( 'NONE',  ( 107.9601777634633635, -17.49593181718839574, 4.828277428366157586 ) ) ;
#2286 = AXIS2_PLACEMENT_3D ( 'NONE', #29302, #21628, #6390 ) ;
#2287 = ORIENTED_EDGE ( 'NONE', *, *, #5697, .T. ) ;
#2288 = CARTESIAN_POINT ( 'NONE',  ( 9.144569539486429477, -14.26359586708033156, 1.499999999999999112 ) ) ;
#2289 = VECTOR ( 'NONE', #15237, 1000.000000000000000 ) ;
#2290 = CARTESIAN_POINT ( 'NONE',  ( 10.00000000000000178, -5.003758587302150396, -0.2500000000000023870 ) ) ;
#2291 = ORIENTED_EDGE ( 'NONE', *, *, #33027, .F. ) ;
#2292 = CARTESIAN_POINT ( 'NONE',  ( 10.18185458677248967, -19.96325353452428786, 1.499999999999999778 ) ) ;
#2293 = EDGE_CURVE ( 'NONE', #29995, #6237, #29872, .T. ) ;
#2294 = ORIENTED_EDGE ( 'NONE', *, *, #12893, .T. ) ;
#2295 = CYLINDRICAL_SURFACE ( 'NONE', #575, 0.4500000000000025646 ) ;
#2296 = FACE_OUTER_BOUND ( 'NONE', #18324, .T. ) ;
#2297 = CARTESIAN_POINT ( 'NONE',  ( 10.57125986779756843, 4.681538312723528605, -0.8254815157534771686 ) ) ;
#2298 = CARTESIAN_POINT ( 'NONE',  ( 107.6149215477164205, -15.92400613423469302, -1.487010776595593331 ) ) ;
#2299 = CARTESIAN_POINT ( 'NONE',  ( 21.43024762280364470, -21.75451284338814162, -1.453503648288084760 ) ) ;
#2300 = DIRECTION ( 'NONE',  ( 8.574039729943018344E-17, 1.000000000000000000, 0.000000000000000000 ) ) ;
#2301 = EDGE_CURVE ( 'NONE', #5840, #28620, #26805, .T. ) ;
#2302 = VERTEX_POINT ( 'NONE', #11644 ) ;
#2303 = CC_DESIGN_DATE_AND_TIME_ASSIGNMENT ( #27402, #32086, ( #14051 ) ) ;
#2304 = VECTOR ( 'NONE', #24685, 1000.000000000000000 ) ;
#2305 = B_SPLINE_CURVE_WITH_KNOTS ( 'NONE', 3,
 ( #18952, #8893, #26314, #16574, #4067, #21446, #5893, #11422, #26621, #23940, #8746, #21768, #8411 ),
 .UNSPECIFIED., .F., .F.,
 ( 4, 3, 3, 3, 4 ),
 ( 1.301042606982605513E-18, 0.0005988814224540803992, 0.001512661714883095426, 0.002883332157778191723, 0.003274339315335596419 ),
 .UNSPECIFIED. ) ;
#2306 =( BOUNDED_CURVE ( )  B_SPLINE_CURVE ( 2, ( #6498, #31928, #6676, #9341, #1349, #31775, #14508, #8846, #27062, #19053, #16703 ),
 .UNSPECIFIED., .F., .F. ) 
 B_SPLINE_CURVE_WITH_KNOTS ( ( 3, 2, 2, 2, 2, 3 ),
 ( 0.6228822619934377691, 0.6250000000000000000, 0.6406250000000000000, 0.6562500000000000000, 0.6718750000000000000, 0.6853822619934377691 ),
 .UNSPECIFIED. ) 
 CURVE ( )  GEOMETRIC_REPRESENTATION_ITEM ( )  RATIONAL_B_SPLINE_CURVE ( ( 0.9821626249036861100, 0.9896829947469995004, 1.000000000000000000, 0.9238795325112867385, 1.000000000000000000, 0.9238795325112867385, 1.000000000000000000, 0.9238795325112867385, 1.000000000000000000, 0.9341965377642872381, 0.9821626249036861100 ) ) 
 REPRESENTATION_ITEM ( '' )  );
#2307 = VECTOR ( 'NONE', #19080, 1000.000000000000000 ) ;
#2308 = CARTESIAN_POINT ( 'NONE',  ( -31.06438740200783855, 3.643637926576053676, 8.172925694146080389 ) ) ;
#2309 = B_SPLINE_CURVE_WITH_KNOTS ( 'NONE', 3,
 ( #13115, #20655, #20803, #15791 ),
 .UNSPECIFIED., .F., .F.,
 ( 4, 4 ),
 ( 0.000000000000000000, 2.202191994273081657E-08 ),
 .UNSPECIFIED. ) ;
#2310 = CARTESIAN_POINT ( 'NONE',  ( 109.4744264295851082, 15.07339897850246579, -2.806473568333506474 ) ) ;
#2311 = CARTESIAN_POINT ( 'NONE',  ( 2.274274201625317016, -1.975651141462152482, -10.82112760146740982 ) ) ;
#2312 = CARTESIAN_POINT ( 'NONE',  ( 101.7092342197782671, -2.711528754415359455, -3.693496777363507899 ) ) ;
#2313 = CIRCLE ( 'NONE', #12958, 6.250000000000000000 ) ;
#2314 = AXIS2_PLACEMENT_3D ( 'NONE', #2221, #7240, #4575 ) ;
#2315 = CIRCLE ( 'NONE', #22061, 297.9387600756452912 ) ;
#2316 = LINE ( 'NONE', #9826, #27373 ) ;
#2317 = CARTESIAN_POINT ( 'NONE',  ( 8.883366670699761071E-16, -1.425064293572414265, 10.85582367538893855 ) ) ;
#2318 = CARTESIAN_POINT ( 'NONE',  ( -56.76591339919558976, 0.3588337185217547742, -1.487708500135610290 ) ) ;
#2319 = CARTESIAN_POINT ( 'NONE',  ( 22.65740490676230579, -21.90673157959312434, 1.180310388834064028 ) ) ;
#2320 = ORIENTED_EDGE ( 'NONE', *, *, #32476, .T. ) ;
#2321 = CIRCLE ( 'NONE', #9769, 5.009999999999999787 ) ;
#2322 = CARTESIAN_POINT ( 'NONE',  ( -7.312550801365594211, -1.088641768524163389, -3.675193018007246071 ) ) ;
#2323 = VERTEX_POINT ( 'NONE', #4135 ) ;
#2324 = EDGE_CURVE ( 'NONE', #32756, #6345, #14156, .T. ) ;
#2325 = CARTESIAN_POINT ( 'NONE',  ( -6.204531657079157547, -1.883076972206379818, -2.325406398514292761 ) ) ;
#2326 = B_SPLINE_CURVE_WITH_KNOTS ( 'NONE', 3,
 ( #4626, #20172, #26017, #10467, #23334, #2465 ),
 .UNSPECIFIED., .F., .F.,
 ( 4, 2, 4 ),
 ( 0.0008064882591616886988, 0.001631107178945768489, 0.002455726098729848171 ),
 .UNSPECIFIED. ) ;
#2327 = CARTESIAN_POINT ( 'NONE',  ( 25.36000000136559862, -1.570731468192933633, -2.892927487894330074 ) ) ;
#2328 = ADVANCED_FACE ( 'NONE', ( #9307 ), #24354, .T. ) ;
#2329 = CARTESIAN_POINT ( 'NONE',  ( 56.97280603064898941, -277.2763395528616002, -0.4463807625373593657 ) ) ;
#2330 = CARTESIAN_POINT ( 'NONE',  ( 2.482257818914018088, 0.000000000000000000, -1.712210361609936005 ) ) ;
#2331 = CARTESIAN_POINT ( 'NONE',  ( 2.410813113191278223, -0.09135288944859165650, 1.740945950647664331 ) ) ;
#2332 = ORIENTED_EDGE ( 'NONE', *, *, #22581, .T. ) ;
#2333 = CARTESIAN_POINT ( 'NONE',  ( 0.7632845268398871230, -8.152713396088739017, -3.174628368996162298 ) ) ;
#2334 = AXIS2_PLACEMENT_3D ( 'NONE', #19138, #3766, #3950 ) ;
#2335 = ORIENTED_EDGE ( 'NONE', *, *, #14787, .F. ) ;
#2336 = CARTESIAN_POINT ( 'NONE',  ( -3.706376978575949277, 0.1572233378491263989, -2.999999999999999556 ) ) ;
#2338 = AXIS2_PLACEMENT_3D ( 'NONE', #11838, #22363, #29393 ) ;
#2337 = PERSON_AND_ORGANIZATION_ROLE ( 'design_supplier' ) ;
#2339 = CARTESIAN_POINT ( 'NONE',  ( 54.97704564079767664, -6.500107750844804855, 4.003574679610500731 ) ) ;
#2340 = CIRCLE ( 'NONE', #27406, 10.99999999999999822 ) ;
#2341 = TOROIDAL_SURFACE ( 'NONE', #18867, 6.000000000000000000, 2.750000000000000444 ) ;
#2342 = CIRCLE ( 'NONE', #16123, 6.248999999999998778 ) ;
#2343 = CARTESIAN_POINT ( 'NONE',  ( 6.530491712438077023, 4.859093986587958547, -7.168846788212641208 ) ) ;
#2345 = DIRECTION ( 'NONE',  ( 0.000000000000000000, 0.000000000000000000, -1.000000000000000000 ) ) ;
#2344 = CARTESIAN_POINT ( 'NONE',  ( 72.90878003214282899, -18.24052684336788488, -1.499999999999999556 ) ) ;
#2346 = AXIS2_PLACEMENT_3D ( 'NONE', #27753, #13689, #11033 ) ;
#2347 = ORIENTED_EDGE ( 'NONE', *, *, #10593, .F. ) ;
#2348 = APPROVAL_PERSON_ORGANIZATION ( #23739, #16568, #10869 ) ;
#2349 = CARTESIAN_POINT ( 'NONE',  ( -8.000050800000000351, -1.352866546975186379, -2.692392053336499114 ) ) ;
#2350 = DIRECTION ( 'NONE',  ( 0.000000000000000000, 1.000000000000000000, 0.000000000000000000 ) ) ;
#2351 = CARTESIAN_POINT ( 'NONE',  ( 22.67250000136559507, 3.024605502323846729, -0.3178988483021056854 ) ) ;
#2352 = CARTESIAN_POINT ( 'NONE',  ( 21.03177542174492487, -17.18603084754148469, -1.753176640694678712 ) ) ;
#2354 = ORIENTED_EDGE ( 'NONE', *, *, #9148, .T. ) ;
#2353 = CARTESIAN_POINT ( 'NONE',  ( 3.527557386959605967, -11.88551672347146848, 0.9788672205888330202 ) ) ;
#2355 = CARTESIAN_POINT ( 'NONE',  ( -4.762550801365593500, 2.752080473201636845, -2.228590825266444142 ) ) ;
#2356 = CARTESIAN_POINT ( 'NONE',  ( 3.249999999999999556, 6.478011392632983423, -6.807171995660517005 ) ) ;
#2357 = DIRECTION ( 'NONE',  ( 0.000000000000000000, 1.000000000000000000, 0.000000000000000000 ) ) ;
#2358 = DIRECTION ( 'NONE',  ( 0.000000000000000000, -0.000000000000000000, 1.000000000000000000 ) ) ;
#2359 = ORIENTED_EDGE ( 'NONE', *, *, #3562, .T. ) ;
#2361 = VERTEX_POINT ( 'NONE', #6798 ) ;
#2360 = DIRECTION ( 'NONE',  ( 0.9842544651762055175, -0.1767573132311700268, 0.000000000000000000 ) ) ;
#2362 = CIRCLE ( 'NONE', #9272, 0.4500000000000033418 ) ;
#2363 = AXIS2_PLACEMENT_3D ( 'NONE', #27858, #7809, #30226 ) ;
#2364 = CARTESIAN_POINT ( 'NONE',  ( 13.23555367686087259, 7.539807145823324674, 1.500000000000000222 ) ) ;
#2365 = CARTESIAN_POINT ( 'NONE',  ( 3.063284526839887167, 0.000000000000000000, 0.000000000000000000 ) ) ;
#2366 = VECTOR ( 'NONE', #53, 1000.000000000000114 ) ;
#2367 = ADVANCED_FACE ( 'NONE', ( #24683 ), #29210, .F. ) ;
#2368 = CARTESIAN_POINT ( 'NONE',  ( 22.29750000136559507, -2.363507492473152283, -1.913930629741525280 ) ) ;
#2369 = ADVANCED_FACE ( 'NONE', ( #27367 ), #31895, .F. ) ;
#2370 = CARTESIAN_POINT ( 'NONE',  ( 84.89587746248274414, -2.934653466126000421, 2.184955971586097778 ) ) ;
#2371 = CARTESIAN_POINT ( 'NONE',  ( -0.1324184762035490182, -14.88641855047732143, -1.499999999999879874 ) ) ;
#2372 = CARTESIAN_POINT ( 'NONE',  ( -56.28351068137280322, 0.4500000000000000111, -1.000000000000000000 ) ) ;
#2373 = PRODUCT_DEFINITION_FORMATION_WITH_SPECIFIED_SOURCE ( 'ANY', '', #12431, .NOT_KNOWN. ) ;
#2374 = DIRECTION ( 'NONE',  ( 8.541412920197209954E-17, 0.9961946980917444350, 0.08715574274767161345 ) ) ;
#2375 = CARTESIAN_POINT ( 'NONE',  ( 69.32965659118902124, -6.955028994486257332, 4.522129901861162260 ) ) ;
#2376 = EDGE_LOOP ( 'NONE', ( #2741, #23359, #6753, #23925 ) ) ;
#2377 = CARTESIAN_POINT ( 'NONE',  ( 3.020080256209070502, 6.926136578651395759, -5.680439424473750165 ) ) ;
#2378 = PERSON_AND_ORGANIZATION ( #6766, #25292 ) ;
#2379 = DIRECTION ( 'NONE',  ( -1.000000000000000000, -0.000000000000000000, 0.000000000000000000 ) ) ;
#2380 = ORIENTED_EDGE ( 'NONE', *, *, #17335, .T. ) ;
#2381 = CIRCLE ( 'NONE', #28006, 5.010000000000000675 ) ;
#2382 = CARTESIAN_POINT ( 'NONE',  ( 107.4617478720205099, 17.99143216401991197, -4.844664824704018713 ) ) ;
#2383 = ORIENTED_EDGE ( 'NONE', *, *, #22399, .T. ) ;
#2384 = CARTESIAN_POINT ( 'NONE',  ( -5.007304909706597584, 1.062355717592095683, 2.999999999999999112 ) ) ;
#2386 = ORIENTED_EDGE ( 'NONE', *, *, #7504, .T. ) ;
#2385 = CARTESIAN_POINT ( 'NONE',  ( 54.94565165835368958, -5.365794815109278026, -4.003574679618516541 ) ) ;
#2387 = ORIENTED_EDGE ( 'NONE', *, *, #14627, .T. ) ;
#2388 = CARTESIAN_POINT ( 'NONE',  ( -1.996286585346912723, 1.323625320507515246, 3.284597389079959573 ) ) ;
#2389 = FACE_OUTER_BOUND ( 'NONE', #26903, .T. ) ;
#2390 = DIRECTION ( 'NONE',  ( 1.000000000000000000, 0.000000000000000000, 0.000000000000000000 ) ) ;
#2391 = CARTESIAN_POINT ( 'NONE',  ( 69.38611993481310947, -8.080330187051609769, -2.713652344655542059 ) ) ;
#2393 = ORIENTED_EDGE ( 'NONE', *, *, #13040, .T. ) ;
#2392 = CARTESIAN_POINT ( 'NONE',  ( 0.5640492482744796643, 5.053269777826659315, 8.091724846332267518 ) ) ;
#2394 = CARTESIAN_POINT ( 'NONE',  ( 19.81525666539894459, 15.27091977451247828, -1.050000000000000044 ) ) ;
#2395 = CARTESIAN_POINT ( 'NONE',  ( 6.220890055303850197, -15.20372210278348035, 4.522129901861156931 ) ) ;
#2396 = CARTESIAN_POINT ( 'NONE',  ( 6.038145077921538650, -3.316258947000913615, 7.799182446117183254 ) ) ;
#2397 = LOCAL_TIME ( 16, 7, 10.00000000000000000, #9956 ) ;
#2398 = CARTESIAN_POINT ( 'NONE',  ( 2.864530965498453874, 9.276519854389890796, -2.320611941139828716 ) ) ;
#2400 = EDGE_LOOP ( 'NONE', ( #9114, #15035, #17606 ) ) ;
#2399 = CARTESIAN_POINT ( 'NONE',  ( 33.81874022276150527, 19.50000000000000000, -1.977928362984233246 ) ) ;
#2401 = CARTESIAN_POINT ( 'NONE',  ( 2.440333863880882248, -7.872241054361043489, 7.210444323286330004 ) ) ;
#2402 = EDGE_CURVE ( 'NONE', #7529, #22183, #5682, .T. ) ;
#2403 = DIRECTION ( 'NONE',  ( 7.023442172597821116E-17, 0.8191520442889873577, 0.5735764363510524877 ) ) ;
#2404 = CARTESIAN_POINT ( 'NONE',  ( 24.42250000136559507, 1.913930629741522838, -2.363507492473150062 ) ) ;
#2405 = DIRECTION ( 'NONE',  ( -0.000000000000000000, 0.000000000000000000, 1.000000000000000000 ) ) ;
#2406 = CARTESIAN_POINT ( 'NONE',  ( 18.93617721851659041, -3.890633339435721982, 4.522129901861162260 ) ) ;
#2407 = DIRECTION ( 'NONE',  ( 0.000000000000000000, 0.000000000000000000, 1.000000000000000000 ) ) ;
#2408 = CIRCLE ( 'NONE', #25152, 5.010000000000000675 ) ;
#2409 = ORIENTED_EDGE ( 'NONE', *, *, #1584, .F. ) ;
#2410 = FACE_OUTER_BOUND ( 'NONE', #22658, .T. ) ;
#2411 = DIRECTION ( 'NONE',  ( -1.000000000000000000, 0.000000000000000000, 0.000000000000000000 ) ) ;
#2412 = CARTESIAN_POINT ( 'NONE',  ( -6.637550801365594388, -1.088641768524163611, -3.675193018007245627 ) ) ;
#2413 = ORIENTED_EDGE ( 'NONE', *, *, #18188, .F. ) ;
#2414 = ADVANCED_BREP_SHAPE_REPRESENTATION ( '', ( #9961, #2865 ), #30610 ) ;
#2415 = CARTESIAN_POINT ( 'NONE',  ( 4.749760686538667009, 6.139290821770257089, 5.151476664237498504 ) ) ;
#2416 = CARTESIAN_POINT ( 'NONE',  ( -2.617344628312510135, 0.000000000000000000, 1.468739241856748867 ) ) ;
#2417 = EDGE_CURVE ( 'NONE', #15974, #4298, #4790, .T. ) ;
#2418 = CARTESIAN_POINT ( 'NONE',  ( 108.6155529559672885, -15.79924867777639186, -1.500000000000000444 ) ) ;
#2419 = ORIENTED_EDGE ( 'NONE', *, *, #20954, .T. ) ;
#2420 = CARTESIAN_POINT ( 'NONE',  ( 14.14625720941031339, -14.08932802803050066, 0.9999999999999995559 ) ) ;
#2421 = ORIENTED_EDGE ( 'NONE', *, *, #22042, .T. ) ;
#2422 = FACE_OUTER_BOUND ( 'NONE', #28113, .T. ) ;
#2424 = VERTEX_POINT ( 'NONE', #12641 ) ;
#2423 = B_SPLINE_CURVE_WITH_KNOTS ( 'NONE', 3,
 ( #26564, #3664, #8837, #19041, #29232, #3828, #14003, #1338, #21221, #21708, #29388, #26238, #31419, #18695, #6004 ),
 .UNSPECIFIED., .F., .F.,
 ( 4, 1, 2, 2, 2, 2, 2, 4 ),
 ( 0.000000000000000000, 0.1250000000000004996, 0.1875000000000005274, 0.2500000000000005551, 0.3750000000000003886, 0.5000000000000002220, 0.7500000000000001110, 1.000000000000000000 ),
 .UNSPECIFIED. ) ;
#2425 = CARTESIAN_POINT ( 'NONE',  ( -2.861038829132344752, 0.01832029024769343817, 1.013940918434999672 ) ) ;
#2427 = ORIENTED_EDGE ( 'NONE', *, *, #267, .F. ) ;
#2426 = DIRECTION ( 'NONE',  ( 1.000000000000000000, -8.574039729943018344E-17, -0.000000000000000000 ) ) ;
#2428 = ADVANCED_FACE ( 'NONE', ( #30377 ), #25679, .T. ) ;
#2429 = EDGE_LOOP ( 'NONE', ( #22197, #11013, #30995, #28304 ) ) ;
#2430 = DIRECTION ( 'NONE',  ( 7.472768010110926752E-18, 0.08715574274765534868, 0.9961946980917457672 ) ) ;
#2431 = ORIENTED_EDGE ( 'NONE', *, *, #23196, .F. ) ;
#2432 = DIRECTION ( 'NONE',  ( 0.000000000000000000, -0.4226182617407029940, -0.9063077870366482713 ) ) ;
#2434 = ORIENTED_EDGE ( 'NONE', *, *, #7297, .F. ) ;
#2433 = CARTESIAN_POINT ( 'NONE',  ( 12.65465643788354200, -15.70291107026620914, -1.500000000000000000 ) ) ;
#2435 = CARTESIAN_POINT ( 'NONE',  ( 3.403631140498738272, -11.97511429332634947, -1.758598531020624467 ) ) ;
#2436 = EDGE_CURVE ( 'NONE', #24201, #7257, #30554, .T. ) ;
#2437 = CARTESIAN_POINT ( 'NONE',  ( 22.92640216610100623, -21.90430348730661692, -1.195188340063571886 ) ) ;
#2438 = DIRECTION ( 'NONE',  ( 0.000000000000000000, -0.9945218953682744001, 0.1045284632676436593 ) ) ;
#2439 = LINE ( 'NONE', #17610, #22610 ) ;
#2440 = DIRECTION ( 'NONE',  ( 1.000000000000000000, -8.574039729943018344E-17, -0.000000000000000000 ) ) ;
#2441 = FACE_OUTER_BOUND ( 'NONE', #5767, .T. ) ;
#2442 = CARTESIAN_POINT ( 'NONE',  ( 25.10129074172987274, -17.52164282029619358, 1.281897516810119209 ) ) ;
#2443 = EDGE_CURVE ( 'NONE', #22183, #13510, #28012, .T. ) ;
#2444 = ADVANCED_FACE ( 'NONE', ( #4633 ), #10309, .T. ) ;
#2445 = CARTESIAN_POINT ( 'NONE',  ( 8.930755659325141593, 0.5000000000000008882, 1.500000000000000000 ) ) ;
#2446 = CARTESIAN_POINT ( 'NONE',  ( 54.77277180716814087, -8.244003004416214253, -0.07017451552783579571 ) ) ;
#2447 = DIRECTION ( 'NONE',  ( 0.000000000000000000, 1.000000000000000000, -1.224646799147353207E-16 ) ) ;
#2448 = CARTESIAN_POINT ( 'NONE',  ( 47.68482864957696421, -3.825617316378856714, 0.02339150516272765420 ) ) ;
#2449 = CARTESIAN_POINT ( 'NONE',  ( 4.749760686538667009, 1.391664247347333294, -7.892520144992419162 ) ) ;
#2450 = CARTESIAN_POINT ( 'NONE',  ( -3.850050802731187272, -1.887961173149512062, -2.331437884370912261 ) ) ;
#2451 = ORIENTED_EDGE ( 'NONE', *, *, #3980, .T. ) ;
#2452 = CARTESIAN_POINT ( 'NONE',  ( -4.337550801365595454, -3.368539882008727115, -1.828967928396028064 ) ) ;
#2453 = DIRECTION ( 'NONE',  ( -1.000000000000000000, -0.000000000000000000, -0.000000000000000000 ) ) ;
#2454 = FACE_OUTER_BOUND ( 'NONE', #2925, .T. ) ;
#2455 = EDGE_LOOP ( 'NONE', ( #980, #31284, #17475, #11594, #15851, #9299 ) ) ;
#2456 = DIRECTION ( 'NONE',  ( -1.000000000000000000, 0.000000000000000000, 0.000000000000000000 ) ) ;
#2457 = CARTESIAN_POINT ( 'NONE',  ( 6.524595623740805372, -6.028129343649572647, -6.215987993068505801 ) ) ;
#2458 = EDGE_CURVE ( 'NONE', #24580, #4070, #22014, .T. ) ;
#2459 = EDGE_LOOP ( 'NONE', ( #29247, #23738, #22150, #15242 ) ) ;
#2460 = CARTESIAN_POINT ( 'NONE',  ( 3.249999999999999556, -3.174628368996134320, 8.152713396088753228 ) ) ;
#2461 = COORDINATED_UNIVERSAL_TIME_OFFSET ( 0, 0, .AHEAD. ) ;
#2463 = ORIENTED_EDGE ( 'NONE', *, *, #16487, .F. ) ;
#2462 = CARTESIAN_POINT ( 'NONE',  ( 3.249999999999999556, -9.241976615262169403, 1.699438267350338982 ) ) ;
#2464 = ORIENTED_EDGE ( 'NONE', *, *, #14920, .F. ) ;
#2465 = CARTESIAN_POINT ( 'NONE',  ( -3.687551352559800218E-13, 10.76487093102146098, 1.999317321091203192 ) ) ;
#2466 = EDGE_LOOP ( 'NONE', ( #6872, #30643, #24132, #30804 ) ) ;
#2467 = CARTESIAN_POINT ( 'NONE',  ( 0.000000000000000000, 1.425064293572489094, -10.85582367538892790 ) ) ;
#2469 = EDGE_LOOP ( 'NONE', ( #16835, #18940, #12887, #30734 ) ) ;
#2468 = CARTESIAN_POINT ( 'NONE',  ( 4.546085788309846232E-16, -9.884132761439026638, -4.709950686174718903 ) ) ;
#2470 = CARTESIAN_POINT ( 'NONE',  ( 10.00000000000000178, -8.574039729943018837E-16, 0.000000000000000000 ) ) ;
#2471 = LINE ( 'NONE', #23340, #24041 ) ;
#2472 = EDGE_CURVE ( 'NONE', #3311, #21158, #9273, .T. ) ;
#2473 = CARTESIAN_POINT ( 'NONE',  ( 21.38384797955244565, -21.75816543643470169, -1.434735962053344416 ) ) ;
#2474 = CARTESIAN_POINT ( 'NONE',  ( -4.013969549054180728E-16, -4.681538312723511730, -0.8254815157535732029 ) ) ;
#2475 = ORIENTED_EDGE ( 'NONE', *, *, #21718, .F. ) ;
#2476 = DIRECTION ( 'NONE',  ( 1.000000000000000000, 0.000000000000000000, 0.000000000000000000 ) ) ;
#2477 = FACE_OUTER_BOUND ( 'NONE', #20771, .T. ) ;
#2478 = CARTESIAN_POINT ( 'NONE',  ( 48.53640747082131668, 22.19355195243385026, -1.491740999229419273 ) ) ;
#2479 = PLANE ( 'NONE',  #30141 ) ;
#2480 = EDGE_CURVE ( 'NONE', #16558, #6094, #12789, .T. ) ;
#2481 = ADVANCED_FACE ( 'NONE', ( #15470 ), #25304, .T. ) ;
#2482 = CARTESIAN_POINT ( 'NONE',  ( 3.063284526839887167, 8.152713396088806519, -3.174628368995990879 ) ) ;
#2483 = CARTESIAN_POINT ( 'NONE',  ( 0.7632845268398871230, -0.4999240074895051067, 8.734705317681624948 ) ) ;
#2484 = CARTESIAN_POINT ( 'NONE',  ( -56.69688924229027549, 0.2251703961848605107, -1.041696575785743484 ) ) ;
#2485 = CARTESIAN_POINT ( 'NONE',  ( 22.49117028854453793, -21.89694127986719963, 1.202706146049940639 ) ) ;
#2486 = VERTEX_POINT ( 'NONE', #17342 ) ;
#2487 = CARTESIAN_POINT ( 'NONE',  ( -6.212550801365593678, 3.368539882008727115, 1.828967928396026954 ) ) ;
#2488 = VERTEX_POINT ( 'NONE', #28350 ) ;
#2489 = CARTESIAN_POINT ( 'NONE',  ( -6.854531657079157903, 1.545410377633947174, -2.846291840500173365 ) ) ;
#2490 = CARTESIAN_POINT ( 'NONE',  ( 23.04750000136559862, -1.913930629741527500, 2.363507492473149618 ) ) ;
#2491 = DIRECTION ( 'NONE',  ( -7.023442172597817418E-17, -0.8191520442889869136, -0.5735764363510531538 ) ) ;
#2492 = CARTESIAN_POINT ( 'NONE',  ( 8.184049377293504790, -14.35829901518298435, 1.755177411681289712 ) ) ;
#2493 = CYLINDRICAL_SURFACE ( 'NONE', #18346, 8.500000000000000000 ) ;
#2494 = ORIENTED_EDGE ( 'NONE', *, *, #13332, .T. ) ;
#2495 = CARTESIAN_POINT ( 'NONE',  ( -31.59999999999999787, -25.93932300454937945, 1.500000000000000000 ) ) ;
#2496 = EDGE_CURVE ( 'NONE', #17041, #12973, #604, .T. ) ;
#2497 = CC_DESIGN_PERSON_AND_ORGANIZATION_ASSIGNMENT ( #1347, #6987, ( #17797 ) ) ;
#2498 = LINE ( 'NONE', #14364, #26672 ) ;
#2499 = ORIENTED_EDGE ( 'NONE', *, *, #29364, .T. ) ;
#2500 = CARTESIAN_POINT ( 'NONE',  ( -3.600050800000000883, 2.331437884370912705, -1.887961173149511618 ) ) ;
#2501 = PERSON_AND_ORGANIZATION ( #6766, #25292 ) ;
#2502 = CARTESIAN_POINT ( 'NONE',  ( 85.03368400521037529, -5.169987188093748465, 4.043899880995859952 ) ) ;
#2503 = FACE_BOUND ( 'NONE', #5219, .T. ) ;
#2505 = CARTESIAN_POINT ( 'NONE',  ( 6.880160201030086853, -0.6895871680712554186, -8.703862158141015826 ) ) ;
#2504 = CARTESIAN_POINT ( 'NONE',  ( 109.1472041058640912, 18.90877050785832836, -4.999054092451833853 ) ) ;
#2506 = EDGE_LOOP ( 'NONE', ( #21648, #5634, #16217 ) ) ;
#2507 = CARTESIAN_POINT ( 'NONE',  ( -8.000050800000000351, -2.031504781066817422, -2.211944486005439359 ) ) ;
#2508 = DIRECTION ( 'NONE',  ( 0.000000000000000000, 1.000000000000000000, 0.000000000000000000 ) ) ;
#2509 = ADVANCED_FACE ( 'NONE', ( #10797 ), #13286, .T. ) ;
#2510 = CARTESIAN_POINT ( 'NONE',  ( 22.42250000136559507, -0.3178988483021076838, -3.024605502323848949 ) ) ;
#2511 = CARTESIAN_POINT ( 'NONE',  ( 14.73499698773293787, -15.74765953506444838, -1.500000000000000000 ) ) ;
#2513 = VERTEX_POINT ( 'NONE', #16134 ) ;
#2512 = CARTESIAN_POINT ( 'NONE',  ( 12.57238041616097313, -15.42470150510370530, 0.9788672205888330202 ) ) ;
#2514 = CARTESIAN_POINT ( 'NONE',  ( -6.862550801365594033, -0.3701630799359326152, 3.521866450007987037 ) ) ;
#2515 = DIRECTION ( 'NONE',  ( 8.281886410780486375E-17, 0.9659258262890655367, 0.2588190451025310090 ) ) ;
#2516 = DIRECTION ( 'NONE',  ( -0.000000000000000000, 0.000000000000000000, 1.000000000000000000 ) ) ;
#2517 = LINE ( 'NONE', #4681, #12874 ) ;
#2518 = ORIENTED_EDGE ( 'NONE', *, *, #6096, .T. ) ;
#2520 = VERTEX_POINT ( 'NONE', #18150 ) ;
#2519 = CARTESIAN_POINT ( 'NONE',  ( 0.1606233060840195348, 4.384181225613662747, -9.683549581718697397 ) ) ;
#2521 = B_SPLINE_CURVE_WITH_KNOTS ( 'NONE', 3,
 ( #21167, #21005, #31218, #2980 ),
 .UNSPECIFIED., .F., .F.,
 ( 4, 4 ),
 ( 0.000000000000000000, 0.07623956525986190502 ),
 .UNSPECIFIED. ) ;
#2522 = LINE ( 'NONE', #20575, #5427 ) ;
#2523 = CARTESIAN_POINT ( 'NONE',  ( 3.499999999999999556, -5.522688772756351838, -6.461416928141299643 ) ) ;
#2524 = CARTESIAN_POINT ( 'NONE',  ( 24.04750000136559507, -1.913930629741527500, 2.363507492473149618 ) ) ;
#2525 = CARTESIAN_POINT ( 'NONE',  ( 54.93487251132799543, -4.984033517862624052, 3.390608480937900460 ) ) ;
#2526 = CARTESIAN_POINT ( 'NONE',  ( -1.397888388080156474, -14.12209114206489957, -1.500000000000000444 ) ) ;
#2527 = CARTESIAN_POINT ( 'NONE',  ( 2.494186907641620987, -10.32103073665143533, 2.161749562925007417 ) ) ;
#2528 = CARTESIAN_POINT ( 'NONE',  ( -2.619932554246580731E-16, -3.055657119358825557, 3.641590349731918863 ) ) ;
#2529 = CARTESIAN_POINT ( 'NONE',  ( 10.52034268205830614, 3.641590349731970822, -3.055657119358763829 ) ) ;
#2530 = ORIENTED_EDGE ( 'NONE', *, *, #6923, .T. ) ;
#2531 = CARTESIAN_POINT ( 'NONE',  ( -5.338982705820479523E-17, -0.6226916219171703126, -4.971152295393308052 ) ) ;
#2532 = EDGE_CURVE ( 'NONE', #10028, #24965, #27978, .T. ) ;
#2533 = COORDINATED_UNIVERSAL_TIME_OFFSET ( 0, 0, .AHEAD. ) ;
#2534 = CARTESIAN_POINT ( 'NONE',  ( 3.063284526839890720, 5.538577986808988385, -6.772677083992317826 ) ) ;
#2535 = ORIENTED_EDGE ( 'NONE', *, *, #6188, .T. ) ;
#2536 = CARTESIAN_POINT ( 'NONE',  ( 108.1401923855166842, 18.95880644471085574, -4.995517669168206609 ) ) ;
#2537 = ORIENTED_EDGE ( 'NONE', *, *, #16337, .T. ) ;
#2538 = CARTESIAN_POINT ( 'NONE',  ( -23.54713438637982748, 18.46223496596754288, 1.773004750130224627 ) ) ;
#2540 = EDGE_LOOP ( 'NONE', ( #27901, #4885, #17701, #14869 ) ) ;
#2539 = CARTESIAN_POINT ( 'NONE',  ( 54.94569726418254163, -5.367442601113908474, -4.006107073548754727 ) ) ;
#2541 = EDGE_LOOP ( 'NONE', ( #23957, #31888, #19910, #25346 ) ) ;
#2542 = ADVANCED_FACE ( 'NONE', ( #26026 ), #21316, .T. ) ;
#2543 = CARTESIAN_POINT ( 'NONE',  ( -2.962992063741595405, -11.77309494928644185, -1.500000000000000000 ) ) ;
#2544 = CARTESIAN_POINT ( 'NONE',  ( -7.862550801365593145, 3.521866450007987037, 0.3701630799359328372 ) ) ;
#2545 = EDGE_CURVE ( 'NONE', #22465, #24269, #28540, .T. ) ;
#2546 = DIRECTION ( 'NONE',  ( 1.000000000000000000, -0.000000000000000000, -0.000000000000000000 ) ) ;
#2547 = DIRECTION ( 'NONE',  ( 1.000000000000000000, 0.000000000000000000, 0.000000000000000000 ) ) ;
#2549 = ORIENTED_EDGE ( 'NONE', *, *, #10611, .F. ) ;
#2548 = DIRECTION ( 'NONE',  ( -8.574039729943018344E-17, -1.000000000000000000, 0.000000000000000000 ) ) ;
#2550 = CARTESIAN_POINT ( 'NONE',  ( -50.81000000000000227, -10.96999999999998643, 5.700000000000000178 ) ) ;
#2551 = CARTESIAN_POINT ( 'NONE',  ( 10.25005080000000035, 0.000000000000000000, 0.000000000000000000 ) ) ;
#2552 = EDGE_CURVE ( 'NONE', #30559, #31355, #1836, .T. ) ;
#2553 = CARTESIAN_POINT ( 'NONE',  ( -4.524743775585262640, -7.612468530177983972, 1.499999999999999556 ) ) ;
#2554 = CARTESIAN_POINT ( 'NONE',  ( 102.6609843814833027, -1.982062027707615970, 4.522129901861162260 ) ) ;
#2556 = ORIENTED_EDGE ( 'NONE', *, *, #26972, .F. ) ;
#2555 = CARTESIAN_POINT ( 'NONE',  ( 1.615481217893400349E-16, -4.709950686174685153, 9.884132761439042625 ) ) ;
#2557 = CARTESIAN_POINT ( 'NONE',  ( 34.49361350329744624, 0.1741578047003297103, 2.493613503297694933 ) ) ;
#2558 = CARTESIAN_POINT ( 'NONE',  ( 10.00000000000000178, -8.574039729943018837E-16, 0.000000000000000000 ) ) ;
#2559 = CARTESIAN_POINT ( 'NONE',  ( 23.98500000273118715, -0.2613211581691358698, -2.486304738420681559 ) ) ;
#2560 = DIRECTION ( 'NONE',  ( 1.000000000000000000, -8.574039729943018344E-17, -0.000000000000000000 ) ) ;
#2561 = CARTESIAN_POINT ( 'NONE',  ( -29.02642725384296440, 4.820254766716771222, 1.500000000000000000 ) ) ;
#2562 = CARTESIAN_POINT ( 'NONE',  ( 17.99869063402067226, -21.49583829453746731, -1.499999999999980904 ) ) ;
#2563 = ORIENTED_EDGE ( 'NONE', *, *, #12056, .T. ) ;
#2564 = CYLINDRICAL_SURFACE ( 'NONE', #25794, 2.499999999999997780 ) ;
#2565 = DIRECTION ( 'NONE',  ( 1.000000000000000000, -0.000000000000000000, -0.000000000000000000 ) ) ;
#2566 = CARTESIAN_POINT ( 'NONE',  ( -7.537550801365592967, -3.368539882008727115, -1.828967928396027842 ) ) ;
#2567 = ORIENTED_EDGE ( 'NONE', *, *, #4723, .F. ) ;
#2568 =( BOUNDED_CURVE ( )  B_SPLINE_CURVE ( 3, ( #12890, #26105, #8235, #5571 ),
 .UNSPECIFIED., .F., .F. ) 
 B_SPLINE_CURVE_WITH_KNOTS ( ( 4, 4 ),
 ( 4.520402762665447050, 4.712388980384689674 ),
 .UNSPECIFIED. ) 
 CURVE ( )  GEOMETRIC_REPRESENTATION_ITEM ( )  RATIONAL_B_SPLINE_CURVE ( ( 1.000000000000000000, 0.9969307989114568613, 0.9969307989114568613, 1.000000000000000000 ) ) 
 REPRESENTATION_ITEM ( '' )  );
#2569 = DIRECTION ( 'NONE',  ( 0.000000000000000000, -0.5735764363510388320, -0.8191520442889969056 ) ) ;
#2570 = CARTESIAN_POINT ( 'NONE',  ( 6.357667975083866274, 7.724391461487844168, -3.797112024431936295 ) ) ;
#2571 = CARTESIAN_POINT ( 'NONE',  ( 0.8032528114568866506, -4.297275870435939282, -0.9788672205888330202 ) ) ;
#2572 = ORIENTED_EDGE ( 'NONE', *, *, #16111, .F. ) ;
#2573 = CARTESIAN_POINT ( 'NONE',  ( 11.84970817546995114, -13.11509834239990013, 1.000000000000000222 ) ) ;
#2574 = ORIENTED_EDGE ( 'NONE', *, *, #27807, .T. ) ;
#2575 = EDGE_CURVE ( 'NONE', #31833, #21433, #15960, .T. ) ;
#2576 = CARTESIAN_POINT ( 'NONE',  ( 0.6791198108364936425, -3.345077512921525553, -8.522429291907481996 ) ) ;
#2577 = VERTEX_POINT ( 'NONE', #31224 ) ;
#2578 = CARTESIAN_POINT ( 'NONE',  ( -2.037945749704337831E-16, -2.376879293651093406, 4.116875700062075261 ) ) ;
#2579 = PRODUCT_DEFINITION_SHAPE ( 'NONE', 'NONE',  #1899 ) ;
#2581 = ORIENTED_EDGE ( 'NONE', *, *, #10917, .T. ) ;
#2580 = CARTESIAN_POINT ( 'NONE',  ( -3.086647630617488147, -0.4418915582519432617, 1.500000000000000222 ) ) ;
#2582 = ORIENTED_EDGE ( 'NONE', *, *, #11610, .T. ) ;
#2583 = CARTESIAN_POINT ( 'NONE',  ( 3.063284526839891608, 8.734705317681621395, 0.4999240074894719665 ) ) ;
#2584 = EDGE_LOOP ( 'NONE', ( #10800, #23822, #7840, #28718 ) ) ;
#2585 = FACE_OUTER_BOUND ( 'NONE', #23253, .T. ) ;
#2587 = ORIENTED_EDGE ( 'NONE', *, *, #29459, .F. ) ;
#2586 = CARTESIAN_POINT ( 'NONE',  ( 18.87735372170065418, -4.548161977172891390, 3.690548956284755544 ) ) ;
#2588 = CARTESIAN_POINT ( 'NONE',  ( -56.33578448492038859, 0.003046479527604620090, -1.000000000000000000 ) ) ;
#2589 = CARTESIAN_POINT ( 'NONE',  ( 22.54151439274422941, -21.86162235810806109, -1.385141676428145452 ) ) ;
#2590 = CARTESIAN_POINT ( 'NONE',  ( 41.45135008765516460, -9.497951668093163491, 0.07017451552781736601 ) ) ;
#2591 = CARTESIAN_POINT ( 'NONE',  ( 107.8922813183675089, -16.51823989814691629, 1.728346180483987027 ) ) ;
#2592 = CARTESIAN_POINT ( 'NONE',  ( 2.274274201625327230, -7.593217523260523016, -7.958834565716851550 ) ) ;
#2593 = CARTESIAN_POINT ( 'NONE',  ( 15.98687768421490674, -15.99250810535818701, 1.500000000000000444 ) ) ;
#2594 = CARTESIAN_POINT ( 'NONE',  ( 3.499999999999999556, 0.6700234925293823141, -8.473551116235668701 ) ) ;
#2595 = CARTESIAN_POINT ( 'NONE',  ( -0.1366093623685602776, -14.96249823008941604, 1.500000000000000000 ) ) ;
#2596 = LINE ( 'NONE', #12271, #4250 ) ;
#2597 = CARTESIAN_POINT ( 'NONE',  ( 0.5988559074951336214, 7.987249520745825393, 5.028194040378882512 ) ) ;
#2598 = CARTESIAN_POINT ( 'NONE',  ( 41.19430503359171780, -3.886431767412232841, -0.02339150518254430253 ) ) ;
#2599 = FACE_OUTER_BOUND ( 'NONE', #8922, .T. ) ;
#2600 = CARTESIAN_POINT ( 'NONE',  ( -2.300050802731187449, -2.853674364686378695, -1.549418761218566809 ) ) ;
#2601 = ORIENTED_EDGE ( 'NONE', *, *, #11514, .F. ) ;
#2602 = CARTESIAN_POINT ( 'NONE',  ( -6.537550801365592967, 1.828967928396027176, -3.368539882008727115 ) ) ;
#2603 = EDGE_CURVE ( 'NONE', #30805, #23785, #9593, .T. ) ;
#2604 = CYLINDRICAL_SURFACE ( 'NONE', #11414, 8.749000000000002331 ) ;
#2605 = CARTESIAN_POINT ( 'NONE',  ( 20.08514749461435400, -21.49093168682445310, -1.640482353827673601 ) ) ;
#2606 = EDGE_LOOP ( 'NONE', ( #7983, #20682, #100 ) ) ;
#2607 = DIRECTION ( 'NONE',  ( -1.000000000000000000, 0.000000000000000000, 0.000000000000000000 ) ) ;
#2608 = CARTESIAN_POINT ( 'NONE',  ( 2.976845970491569293, 7.079702685456871869, 5.822399416825323470 ) ) ;
#2609 = EDGE_CURVE ( 'NONE', #9843, #9922, #463, .T. ) ;
#2610 = VERTEX_POINT ( 'NONE', #20831 ) ;
#2611 = CARTESIAN_POINT ( 'NONE',  ( 10.55147673363118876, -4.458382051008177527, -2.285372942705001797 ) ) ;
#2612 = APPROVAL_DATE_TIME ( #24996, #17997 ) ;
#2614 = VERTEX_POINT ( 'NONE', #3131 ) ;
#2613 = CARTESIAN_POINT ( 'NONE',  ( 111.3844470440328251, -20.20075132222358505, -1.499999999999999556 ) ) ;
#2616 = ADVANCED_FACE ( 'NONE', ( #8301 ), #18494, .F. ) ;
#2615 = VERTEX_POINT ( 'NONE', #23494 ) ;
#2617 = CARTESIAN_POINT ( 'NONE',  ( 14.60942776824126632, -20.56080517165843347, 1.750898333654289596 ) ) ;
#2618 = ORIENTED_EDGE ( 'NONE', *, *, #1411, .F. ) ;
#2619 = CARTESIAN_POINT ( 'NONE',  ( 108.0105480239282372, -18.22125103716771832, -4.637810049791077915 ) ) ;
#2621 = VERTEX_POINT ( 'NONE', #26360 ) ;
#2620 = CYLINDRICAL_SURFACE ( 'NONE', #18682, 0.5000000000000004441 ) ;
#2622 = CARTESIAN_POINT ( 'NONE',  ( 41.45135008765516460, -9.497951668093168820, 1.010822989962089746 ) ) ;
#2623 = DIRECTION ( 'NONE',  ( 0.000000000000000000, -0.9271838545667854259, -0.3746065934159166777 ) ) ;
#2624 = ADVANCED_FACE ( 'NONE', ( #5784 ), #18824, .T. ) ;
#2625 = CARTESIAN_POINT ( 'NONE',  ( 107.6641398346957033, -20.45810202417174750, 1.500000000000000000 ) ) ;
#2626 = EDGE_CURVE ( 'NONE', #22752, #26914, #12264, .T. ) ;
#2627 = CARTESIAN_POINT ( 'NONE',  ( 7.249760686538667009, 7.530955069117551304, -2.741043480754851380 ) ) ;
#2628 = VERTEX_POINT ( 'NONE', #21172 ) ;
#2629 = CARTESIAN_POINT ( 'NONE',  ( 3.063284526839890276, 4.729683950898869504, 7.360373001730925679 ) ) ;
#2630 = DIRECTION ( 'NONE',  ( -0.1908089953765452762, 0.000000000000000000, 0.9816271834476639757 ) ) ;
#2631 = CARTESIAN_POINT ( 'NONE',  ( 102.9885081044300676, -6.698322160490901567, -0.07017451552783579571 ) ) ;
#2632 = DIRECTION ( 'NONE',  ( 0.000000000000000000, 0.000000000000000000, -1.000000000000000000 ) ) ;
#2633 = EDGE_CURVE ( 'NONE', #19839, #19445, #18642, .T. ) ;
#2634 = CARTESIAN_POINT ( 'NONE',  ( -8.000050800000009232, 0.05039788597990539631, 3.202937075113939880 ) ) ;
#2635 = CARTESIAN_POINT ( 'NONE',  ( -2.143509932485916364E-17, -0.2500000000000183187, 5.003758587302147731 ) ) ;
#2636 = CARTESIAN_POINT ( 'NONE',  ( -17.45597128428593336, -25.93932300454937945, 11.00000000000000000 ) ) ;
#2637 = DIRECTION ( 'NONE',  ( 0.000000000000000000, 0.000000000000000000, -1.000000000000000000 ) ) ;
#2638 = VERTEX_POINT ( 'NONE', #5935 ) ;
#2639 = CARTESIAN_POINT ( 'NONE',  ( -5.362550801365593145, 2.228590825266444142, 2.752080473201636845 ) ) ;
#2640 = ORIENTED_EDGE ( 'NONE', *, *, #15320, .T. ) ;
#2641 = CARTESIAN_POINT ( 'NONE',  ( -8.200050800000001416, 1.887961173149511618, 2.331437884370912705 ) ) ;
#2642 = CARTESIAN_POINT ( 'NONE',  ( 3.499999999999999556, 0.000000000000000000, 0.000000000000000000 ) ) ;
#2643 = CARTESIAN_POINT ( 'NONE',  ( 1.942333353379948502, -0.8689713362383969519, 1.758041117768017747 ) ) ;
#2644 = CARTESIAN_POINT ( 'NONE',  ( 10.63777811968352971, -12.44241537618772320, 1.500000000000427658 ) ) ;
#2645 = ORIENTED_EDGE ( 'NONE', *, *, #22972, .T. ) ;
#2646 = CARTESIAN_POINT ( 'NONE',  ( 0.5664946525141408840, -9.241976615262153416, 2.300561732649529567 ) ) ;
#2647 = ORIENTED_EDGE ( 'NONE', *, *, #1785, .F. ) ;
#2648 = LINE ( 'NONE', #15985, #2242 ) ;
#2649 = APPROVAL_STATUS ( 'not_yet_approved' ) ;
#2650 = EDGE_CURVE ( 'NONE', #285, #1891, #13625, .T. ) ;
#2651 = CARTESIAN_POINT ( 'NONE',  ( 40.88348196906002130, -6.802589077584822341, 4.112224033454269900 ) ) ;
#2652 = ADVANCED_FACE ( 'NONE', ( #16303 ), #23194, .T. ) ;
#2653 = CARTESIAN_POINT ( 'NONE',  ( 7.064632940817594076, 4.973063321323974328, -7.199384779417069780 ) ) ;
#2655 = CARTESIAN_POINT ( 'NONE',  ( -1.176310634206514104E-14, 21.94000000000002260, 1.050000000000000044 ) ) ;
#2654 = DIRECTION ( 'NONE',  ( 1.000000000000000000, -0.000000000000000000, -0.000000000000000000 ) ) ;
#2656 = ORIENTED_EDGE ( 'NONE', *, *, #17503, .F. ) ;
#2657 = EDGE_CURVE ( 'NONE', #9041, #21409, #1434, .T. ) ;
#2658 = CARTESIAN_POINT ( 'NONE',  ( -3.822634483660894942E-16, -4.458382051008176639, -2.285372942705001797 ) ) ;
#2659 = FACE_OUTER_BOUND ( 'NONE', #31742, .T. ) ;
#2660 = CARTESIAN_POINT ( 'NONE',  ( 23.04750000136559862, -1.913930629741527500, 2.363507492473149618 ) ) ;
#2661 = DIRECTION ( 'NONE',  ( 1.000000000000000000, -8.574039729943018344E-17, -0.000000000000000000 ) ) ;
#2662 = VECTOR ( 'NONE', #2103, 1000.000000000000114 ) ;
#2664 = ORIENTED_EDGE ( 'NONE', *, *, #29397, .T. ) ;
#2663 = CARTESIAN_POINT ( 'NONE',  ( 13.13178786249840435, -17.31629153505178920, 4.522129901861157819 ) ) ;
#2665 = CARTESIAN_POINT ( 'NONE',  ( -6.812550801365595099, -1.828967928396026510, 3.368539882008728004 ) ) ;
#2666 = CYLINDRICAL_SURFACE ( 'NONE', #24057, 0.5000000000000000000 ) ;
#2667 = AXIS2_PLACEMENT_3D ( 'NONE', #9755, #255, #63 ) ;
#2668 = CARTESIAN_POINT ( 'NONE',  ( 25.75999999999999801, -2.208672634433321348E-15, 0.000000000000000000 ) ) ;
#2669 = LINE ( 'NONE', #17534, #13389 ) ;
#2670 = VERTEX_POINT ( 'NONE', #11460 ) ;
#2672 = VERTEX_POINT ( 'NONE', #3614 ) ;
#2671 = CARTESIAN_POINT ( 'NONE',  ( 24.43445557112933386, -17.40480440763387904, 1.396984404749296971 ) ) ;
#2673 = EDGE_CURVE ( 'NONE', #22357, #17959, #30504, .T. ) ;
#2674 = AXIS2_PLACEMENT_3D ( 'NONE', #33045, #13139, #31038 ) ;
#2675 = CC_DESIGN_DATE_AND_TIME_ASSIGNMENT ( #290, #25856, ( #6102 ) ) ;
#2676 = CARTESIAN_POINT ( 'NONE',  ( 25.75999999999999801, -2.208672634433321348E-15, 0.000000000000000000 ) ) ;
#2677 = CARTESIAN_POINT ( 'NONE',  ( 0.3045634274091702509, 5.217683548413707406, -8.853895822767748669 ) ) ;
#2678 = CARTESIAN_POINT ( 'NONE',  ( 23.04750000136559862, -1.913930629741527500, 2.363507492473149618 ) ) ;
#2679 = CARTESIAN_POINT ( 'NONE',  ( -23.54713438637982748, 3.998227953278294944, 2.146185852361370383 ) ) ;
#2680 = DIRECTION ( 'NONE',  ( -1.000000000000000000, -0.000000000000000000, 0.000000000000000000 ) ) ;
#2681 = DIRECTION ( 'NONE',  ( 1.000000000000000000, -8.574039729943018344E-17, -0.000000000000000000 ) ) ;
#2682 = CARTESIAN_POINT ( 'NONE',  ( 19.01480233880980819, -3.011762293215293429, 0.07017451552782509594 ) ) ;
#2683 = CARTESIAN_POINT ( 'NONE',  ( 107.8460215217088773, -15.85211033425178861, 1.499787059522396770 ) ) ;
#2684 = ORIENTED_EDGE ( 'NONE', *, *, #27284, .T. ) ;
#2685 = LINE ( 'NONE', #7865, #18264 ) ;
#2686 = AXIS2_PLACEMENT_3D ( 'NONE', #19176, #26879, #29214 ) ;
#2687 = CIRCLE ( 'NONE', #12280, 9.425032312242976218 ) ;
#2688 = APPROVAL_STATUS ( 'not_yet_approved' ) ;
#2689 = EDGE_CURVE ( 'NONE', #3757, #13458, #26878, .T. ) ;
#2690 = FACE_OUTER_BOUND ( 'NONE', #26329, .T. ) ;
#2691 = ORIENTED_EDGE ( 'NONE', *, *, #302, .T. ) ;
#2692 = VECTOR ( 'NONE', #17454, 1000.000000000000000 ) ;
#2693 = CARTESIAN_POINT ( 'NONE',  ( 108.0068349480237657, 18.21621961241920218, -4.398253369385427547 ) ) ;
#2694 = ORIENTED_EDGE ( 'NONE', *, *, #26513, .F. ) ;
#2695 = CARTESIAN_POINT ( 'NONE',  ( -5.250050802731188071, 2.331437884370912705, -1.887961173149511618 ) ) ;
#2697 = EDGE_LOOP ( 'NONE', ( #7451, #10386, #1742 ) ) ;
#2696 = CARTESIAN_POINT ( 'NONE',  ( 28.69334747239712513, -5.625518540330015860, -4.008637382338393174 ) ) ;
#2698 = ORIENTED_EDGE ( 'NONE', *, *, #18975, .F. ) ;
#2699 = CARTESIAN_POINT ( 'NONE',  ( 3.566513200368869096, -17.47573827932033197, 1.500000000000000000 ) ) ;
#2700 = CARTESIAN_POINT ( 'NONE',  ( -6.362550801365593145, 2.752080473201636845, -2.228590825266444142 ) ) ;
#2701 = LINE ( 'NONE', #28259, #20444 ) ;
#2702 = DIRECTION ( 'NONE',  ( 0.000000000000000000, 0.9961946980917462113, -0.08715574274765046370 ) ) ;
#2704 = VERTEX_POINT ( 'NONE', #16953 ) ;
#2703 = CARTESIAN_POINT ( 'NONE',  ( 22.23500000273118715, 2.486304738420679783, -0.2613211581691337604 ) ) ;
#2705 = CARTESIAN_POINT ( 'NONE',  ( 26.08945412691624099, 19.05746434167065928, 1.500000000000000000 ) ) ;
#2706 = DIRECTION ( 'NONE',  ( -1.000000000000000000, 0.000000000000000000, 0.000000000000000000 ) ) ;
#2707 = CARTESIAN_POINT ( 'NONE',  ( -3.817309019801226722, -10.46513237797910989, 1.499999999999999112 ) ) ;
#2708 = CARTESIAN_POINT ( 'NONE',  ( 25.73500000136559507, 1.570731468192929858, 2.892927487894329186 ) ) ;
#2709 = CIRCLE ( 'NONE', #18697, 302.1720608278466216 ) ;
#2710 = FACE_OUTER_BOUND ( 'NONE', #26412, .T. ) ;
#2712 = ORIENTED_EDGE ( 'NONE', *, *, #19321, .F. ) ;
#2711 = CARTESIAN_POINT ( 'NONE',  ( 108.0290687835694854, -18.48794536861594295, -4.329972080810385648 ) ) ;
#2713 = DIRECTION ( 'NONE',  ( 1.000000000000000000, -8.574039729943018344E-17, -0.000000000000000000 ) ) ;
#2715 = ADVANCED_FACE ( 'NONE', ( #9085 ), #16617, .T. ) ;
#2714 = CIRCLE ( 'NONE', #29398, 0.4999999999999996669 ) ;
#2716 = AXIS2_PLACEMENT_3D ( 'NONE', #26094, #3053, #368 ) ;
#2717 = DIRECTION ( 'NONE',  ( -0.000000000000000000, -0.000000000000000000, -1.000000000000000000 ) ) ;
#2718 = CARTESIAN_POINT ( 'NONE',  ( 22.73500000136559862, 1.570731468192929858, 2.892927487894329186 ) ) ;
#2719 = VECTOR ( 'NONE', #17645, 1000.000000000000227 ) ;
#2720 = DIRECTION ( 'NONE',  ( 7.770718973608970028E-17, 0.9063077870366497146, -0.4226182617406998299 ) ) ;
#2721 = DIRECTION ( 'NONE',  ( -3.469446951953478110E-15, 0.000000000000000000, 1.000000000000000000 ) ) ;
#2722 = CARTESIAN_POINT ( 'NONE',  ( -56.49561586466536056, 0.04964621674521208644, 1.500000000000000000 ) ) ;
#2723 = VECTOR ( 'NONE', #5734, 1000.000000000000000 ) ;
#2724 = ORIENTED_EDGE ( 'NONE', *, *, #28904, .F. ) ;
#2725 = CARTESIAN_POINT ( 'NONE',  ( 22.52203367452178995, -21.86037836540916146, 1.500000000000000000 ) ) ;
#2726 = CARTESIAN_POINT ( 'NONE',  ( 108.0291781248179177, -18.48951985539285658, 4.325670280512381005 ) ) ;
#2727 = CARTESIAN_POINT ( 'NONE',  ( 107.4934131274682869, -17.99000828170487765, -5.121421805061605603 ) ) ;
#2728 = ORIENTED_EDGE ( 'NONE', *, *, #12116, .T. ) ;
#2729 = EDGE_CURVE ( 'NONE', #25210, #29208, #21496, .T. ) ;
#2730 = DIRECTION ( 'NONE',  ( 0.000000000000000000, 0.000000000000000000, -1.000000000000000000 ) ) ;
#2731 = EDGE_CURVE ( 'NONE', #13458, #28727, #30102, .T. ) ;
#2732 = DIRECTION ( 'NONE',  ( 0.000000000000000000, 0.000000000000000000, 1.000000000000000000 ) ) ;
#2733 = VECTOR ( 'NONE', #6259, 1000.000000000000000 ) ;
#2734 = CARTESIAN_POINT ( 'NONE',  ( 4.187842409712536805E-16, 4.884328206559836794, 1.115095498423326559 ) ) ;
#2735 = CARTESIAN_POINT ( 'NONE',  ( 18.51491971917340607, -8.599446730134173933, 0.07017451552781736601 ) ) ;
#2736 = ORIENTED_EDGE ( 'NONE', *, *, #15816, .F. ) ;
#2737 = VECTOR ( 'NONE', #5297, 1000.000000000000000 ) ;
#2738 = CIRCLE ( 'NONE', #30518, 8.749000000000002331 ) ;
#2739 = PLANE ( 'NONE',  #22984 ) ;
#2740 = AXIS2_PLACEMENT_3D ( 'NONE', #6951, #27363, #20177 ) ;
#2741 = ORIENTED_EDGE ( 'NONE', *, *, #22289, .T. ) ;
#2742 = CARTESIAN_POINT ( 'NONE',  ( 107.5502113151021177, -18.81587173190781215, 4.846782049358179911 ) ) ;
#2744 = ORIENTED_EDGE ( 'NONE', *, *, #11590, .F. ) ;
#2743 = CARTESIAN_POINT ( 'NONE',  ( 2.143509932486214652E-17, 0.2500000000000532907, -5.003758587302145955 ) ) ;
#2745 = ORIENTED_EDGE ( 'NONE', *, *, #27846, .F. ) ;
#2746 = LINE ( 'NONE', #12920, #31591 ) ;
#2747 = ORIENTED_EDGE ( 'NONE', *, *, #28588, .F. ) ;
#2749 = CIRCLE ( 'NONE', #31025, 0.5000000000000004441 ) ;
#2748 = CYLINDRICAL_SURFACE ( 'NONE', #12972, 0.5000000000000004441 ) ;
#2751 = ORIENTED_EDGE ( 'NONE', *, *, #32175, .T. ) ;
#2750 = CARTESIAN_POINT ( 'NONE',  ( 1.278428506419904798, -2.392608122357158251, -1.500000000000000000 ) ) ;
#2752 = CARTESIAN_POINT ( 'NONE',  ( 4.749760686538667009, -8.014274990069656823, 8.669741416787380218E-17 ) ) ;
#2753 = CARTESIAN_POINT ( 'NONE',  ( 6.920196482735073928, -13.86306298490376143, -1.755640868487531758 ) ) ;
#2754 = CARTESIAN_POINT ( 'NONE',  ( -29.24402871571405882, -25.93932300454937945, 11.00000000000000000 ) ) ;
#2755 = CARTESIAN_POINT ( 'NONE',  ( -0.6528202993443400493, 0.000000000000000000, -5.396302277755718357 ) ) ;
#2756 = LINE ( 'NONE', #17345, #21356 ) ;
#2757 = CARTESIAN_POINT ( 'NONE',  ( 5.885541736258996792, 3.216848386728063947, 7.752826540560520563 ) ) ;
#2758 = VECTOR ( 'NONE', #7931, 1000.000000000000000 ) ;
#2759 = CARTESIAN_POINT ( 'NONE',  ( 107.9622325421415212, 20.81773585569407459, 1.508259000770582059 ) ) ;
#2760 = CARTESIAN_POINT ( 'NONE',  ( 0.6375389515528632201, -7.656606984113278003, 1.500000000000000444 ) ) ;
#2761 = LINE ( 'NONE', #28803, #270 ) ;
#2762 = CIRCLE ( 'NONE', #26767, 10.99999999999999822 ) ;
#2763 = AXIS2_PLACEMENT_3D ( 'NONE', #16924, #27286, #22780 ) ;
#2764 = CARTESIAN_POINT ( 'NONE',  ( 14.21659522551787624, -20.98447794503849906, 0.9788672205877712029 ) ) ;
#2765 = CYLINDRICAL_SURFACE ( 'NONE', #23991, 4.000000000000001776 ) ;
#2766 =( BOUNDED_SURFACE ( )  B_SPLINE_SURFACE ( 3, 2, ( 
 ( #23356, #464, #28374 ),
 ( #9988, #17862, #5490 ),
 ( #145, #28060, #25702 ),
 ( #17670, #5156, #15331 ),
 ( #7318, #12808, #17509 ),
 ( #10643, #25383, #12660 ),
 ( #25536, #18020, #22863 ),
 ( #318, #23023, #10331 ),
 ( #13156, #20546, #30754 ),
 ( #7827, #15488, #20704 ),
 ( #30904, #1113, #812 ),
 ( #16157, #13954, #15833 ),
 ( #3630, #31388, #10988 ),
 ( #3308, #26531, #6138 ) ),
 .UNSPECIFIED., .F., .F., .T. ) 
 B_SPLINE_SURFACE_WITH_KNOTS ( ( 4, 2, 2, 2, 2, 2, 4 ),
 ( 3, 3 ),
 ( 2.385244779468109755E-18, 0.0002022272781459603930, 0.0003033409172189393968, 0.0004044545562919184007, 0.0005055681953648974046, 0.0006066818344378764084, 0.0008089091125838344162 ),
 ( 0.000000000000000000, 1.000000000000000000 ),
 .UNSPECIFIED. ) 
 GEOMETRIC_REPRESENTATION_ITEM ( )  RATIONAL_B_SPLINE_SURFACE ( (
 ( 1.000000000000000000, 0.7097644798780626818, 1.000000000000000000),
 ( 1.000000000000000000, 0.7096080128847354063, 1.000000000000000000),
 ( 1.000000000000000000, 0.7093877859246700002, 1.000000000000000000),
 ( 1.000000000000000000, 0.7087837316534446597, 1.000000000000000000),
 ( 1.000000000000000000, 0.7085305059914599468, 1.000000000000000000),
 ( 1.000000000000000000, 0.7078957402609113991, 1.000000000000000000),
 ( 1.000000000000000000, 0.7075010273771544789, 1.000000000000000000),
 ( 1.000000000000000000, 0.7067064543823278200, 1.000000000000000000),
 ( 1.000000000000000000, 0.7063134043005300233, 1.000000000000000000),
 ( 1.000000000000000000, 0.7056801599291154803, 1.000000000000000000),
 ( 1.000000000000000000, 0.7054276077845391679, 1.000000000000000000),
 ( 1.000000000000000000, 0.7048252423529660637, 1.000000000000000000),
 ( 1.000000000000000000, 0.7046023681409566697, 1.000000000000000000),
 ( 1.000000000000000000, 0.7044453589051569153, 1.000000000000000000) ) ) 
 REPRESENTATION_ITEM ( '' )  SURFACE ( )  );
#2767 = CARTESIAN_POINT ( 'NONE',  ( 6.037141812302427191, 8.411869123983617413, 1.028012177296115492 ) ) ;
#2768 = CARTESIAN_POINT ( 'NONE',  ( -38.14293509397970183, 21.94000000000000128, -1.050000000000000044 ) ) ;
#2769 = CIRCLE ( 'NONE', #3315, 0.4499999999999990119 ) ;
#2770 = CIRCLE ( 'NONE', #19847, 5.010000000000000675 ) ;
#2771 = CARTESIAN_POINT ( 'NONE',  ( 41.43929652434213295, -5.500819839281759549, 5.695980980372492120 ) ) ;
#2772 = EDGE_CURVE ( 'NONE', #21921, #11951, #1786, .T. ) ;
#2773 = DIRECTION ( 'NONE',  ( -6.938893903907222067E-15, 0.000000000000000000, 1.000000000000000000 ) ) ;
#2774 = ORIENTED_EDGE ( 'NONE', *, *, #2188, .T. ) ;
#2775 = ADVANCED_FACE ( 'NONE', ( #9428 ), #14426, .T. ) ;
#2776 = CARTESIAN_POINT ( 'NONE',  ( -5.237550801365594033, -3.675193018007246071, 1.088641768524163167 ) ) ;
#2777 = AXIS2_PLACEMENT_3D ( 'NONE', #19085, #16554, #26764 ) ;
#2778 = AXIS2_PLACEMENT_3D ( 'NONE', #20332, #32893, #7629 ) ;
#2779 = DIRECTION ( 'NONE',  ( 0.000000000000000000, 0.000000000000000000, 1.000000000000000000 ) ) ;
#2780 = CARTESIAN_POINT ( 'NONE',  ( 18.68429645396945560, -21.55436976724162790, -1.490931396286244937 ) ) ;
#2781 = ORIENTED_EDGE ( 'NONE', *, *, #11663, .F. ) ;
#2782 = CARTESIAN_POINT ( 'NONE',  ( 6.357668022120090079, -5.080751859797305592, -6.947679035623508526 ) ) ;
#2783 = EDGE_LOOP ( 'NONE', ( #9441, #19399, #7823, #17093 ) ) ;
#2784 = CARTESIAN_POINT ( 'NONE',  ( 0.7632845268398871230, 0.000000000000000000, 0.000000000000000000 ) ) ;
#2785 = PERSON_AND_ORGANIZATION_ROLE ( 'classification_officer' ) ;
#2787 = ORIENTED_EDGE ( 'NONE', *, *, #26098, .F. ) ;
#2786 = CARTESIAN_POINT ( 'NONE',  ( 29.11693253002209403, -8.303828435806185126, 0.07017451552781736601 ) ) ;
#2788 = EDGE_LOOP ( 'NONE', ( #25595, #11177, #27135, #6110 ) ) ;
#2789 = CARTESIAN_POINT ( 'NONE',  ( -3.348806739241649399, -1.982316163823921507, 1.747785182639436830 ) ) ;
#2790 = CIRCLE ( 'NONE', #16644, 3.000000000000000444 ) ;
#2791 = VECTOR ( 'NONE', #12402, 1000.000000000000000 ) ;
#2792 = ORIENTED_EDGE ( 'NONE', *, *, #16898, .F. ) ;
#2793 = CARTESIAN_POINT ( 'NONE',  ( 10.00000000000000000, 4.681538312723516171, 0.8254815157535410064 ) ) ;
#2795 = VERTEX_POINT ( 'NONE', #6916 ) ;
#2794 = CARTESIAN_POINT ( 'NONE',  ( 19.10390797508229710, -2.015740111943975066, 0.07017451552782062729 ) ) ;
#2796 = AXIS2_PLACEMENT_3D ( 'NONE', #21405, #24245, #24058 ) ;
#2797 = CARTESIAN_POINT ( 'NONE',  ( 48.09235817783085309, -9.172289267036328297, 1.915219082070893863 ) ) ;
#2798 = CARTESIAN_POINT ( 'NONE',  ( -42.85764933975779201, 24.74387538314362800, 1.500000000000000000 ) ) ;
#2799 = CIRCLE ( 'NONE', #25741, 303.0536494382092769 ) ;
#2800 = DIRECTION ( 'NONE',  ( 1.000000000000000000, 0.000000000000000000, 0.000000000000000000 ) ) ;
#2801 = EDGE_CURVE ( 'NONE', #16210, #29752, #28283, .T. ) ;
#2802 = DIRECTION ( 'NONE',  ( -1.000000000000000000, 0.000000000000000000, 0.000000000000000000 ) ) ;
#2803 = AXIS2_PLACEMENT_3D ( 'NONE', #29453, #11561, #23781 ) ;
#2805 = AXIS2_PLACEMENT_3D ( 'NONE', #22728, #32932, #1851 ) ;
#2804 = B_SPLINE_CURVE_WITH_KNOTS ( 'NONE', 3,
 ( #16658, #31559, #1466, #29207, #11324, #13972, #6297, #16333 ),
 .UNSPECIFIED., .F., .F.,
 ( 4, 2, 2, 4 ),
 ( 2.304311362529371646E-07, 0.001261163669367344363, 0.001891630288482889968, 0.002522096907598435789 ),
 .UNSPECIFIED. ) ;
#2806 = VERTEX_POINT ( 'NONE', #14928 ) ;
#2807 = CARTESIAN_POINT ( 'NONE',  ( 21.05656763645044904, 0.8852964313267427388, -2.499999999999999112 ) ) ;
#2808 = CARTESIAN_POINT ( 'NONE',  ( -23.54713438637982748, 3.094594691910233841, 6.506829104297265687 ) ) ;
#2809 = LINE ( 'NONE', #799, #15531 ) ;
#2810 = FACE_OUTER_BOUND ( 'NONE', #20822, .T. ) ;
#2811 = EDGE_CURVE ( 'NONE', #1705, #6111, #17079, .T. ) ;
#2812 = DIRECTION ( 'NONE',  ( 0.000000000000000000, 0.4226182617406936681, 0.9063077870366527122 ) ) ;
#2813 = CIRCLE ( 'NONE', #26364, 8.749000000000002331 ) ;
#2814 = CARTESIAN_POINT ( 'NONE',  ( -50.81000000000000227, -10.96999999999998643, 0.000000000000000000 ) ) ;
#2815 = CARTESIAN_POINT ( 'NONE',  ( -56.41635936944848595, 0.01859738704150220093, -1.012721741759385230 ) ) ;
#2817 = DIRECTION ( 'NONE',  ( 0.000000000000000000, 0.4226182617406968323, 0.9063077870366511579 ) ) ;
#2816 = UNCERTAINTY_MEASURE_WITH_UNIT (LENGTH_MEASURE( 1.000000000000000082E-05 ), #25162, 'distance_accuracy_value', 'NONE');
#2818 = VERTEX_POINT ( 'NONE', #33014 ) ;
#2819 = VECTOR ( 'NONE', #7274, 1000.000000000000000 ) ;
#2820 = VECTOR ( 'NONE', #21328, 1000.000000000000227 ) ;
#2821 = CARTESIAN_POINT ( 'NONE',  ( -7.062550801365593323, 3.521866450007987037, 0.3701630799359328372 ) ) ;
#2822 = ORIENTED_EDGE ( 'NONE', *, *, #24401, .T. ) ;
#2823 = EDGE_CURVE ( 'NONE', #29918, #11672, #24820, .T. ) ;
#2824 = VECTOR ( 'NONE', #17973, 1000.000000000000227 ) ;
#2825 = VECTOR ( 'NONE', #28937, 1000.000000000000227 ) ;
#2826 = CARTESIAN_POINT ( 'NONE',  ( -3.754531657079158258, -0.9198621039125872700, -3.105402419394638791 ) ) ;
#2827 = AXIS2_PLACEMENT_3D ( 'NONE', #11334, #8826, #19180 ) ;
#2828 = VECTOR ( 'NONE', #517, 1000.000000000000000 ) ;
#2829 = EDGE_CURVE ( 'NONE', #6812, #26011, #12807, .T. ) ;
#2830 = DIRECTION ( 'NONE',  ( -1.000000000000000000, -0.000000000000000000, -0.000000000000000000 ) ) ;
#2831 = CARTESIAN_POINT ( 'NONE',  ( 6.329657586300834637, -13.60801132437365801, 1.755870824322850465 ) ) ;
#2832 = CARTESIAN_POINT ( 'NONE',  ( 19.32480846800364915, -16.28061487828867016, 1.500000000000000000 ) ) ;
#2833 = AXIS2_PLACEMENT_3D ( 'NONE', #24528, #29902, #8988 ) ;
#2834 = VERTEX_POINT ( 'NONE', #7413 ) ;
#2835 = CARTESIAN_POINT ( 'NONE',  ( 20.49290772595112742, 0.1310194482076003919, 2.499999999999998668 ) ) ;
#2836 = CIRCLE ( 'NONE', #27919, 4.000000000000002665 ) ;
#2837 = VERTEX_POINT ( 'NONE', #2257 ) ;
#2838 = CARTESIAN_POINT ( 'NONE',  ( 3.063284526839887167, 3.174628368996073924, 8.152713396088772768 ) ) ;
#2839 = DATE_AND_TIME ( #30588, #7158 ) ;
#2840 = EDGE_CURVE ( 'NONE', #2670, #31785, #21365, .T. ) ;
#2841 = CARTESIAN_POINT ( 'NONE',  ( 28.66558084216347879, -6.707193022007285954, 4.073741754960026107 ) ) ;
#2842 = AXIS2_PLACEMENT_3D ( 'NONE', #11680, #30108, #16522 ) ;
#2843 = CARTESIAN_POINT ( 'NONE',  ( 21.36097421961354925, -21.76718868951427055, 1.410897148389129052 ) ) ;
#2844 = AXIS2_PLACEMENT_3D ( 'NONE', #12873, #23095, #22 ) ;
#2846 = DIRECTION ( 'NONE',  ( -1.000000000000000000, 0.000000000000000000, 0.000000000000000000 ) ) ;
#2845 = DIRECTION ( 'NONE',  ( -1.000000000000000000, 0.000000000000000000, 0.000000000000000000 ) ) ;
#2847 = B_SPLINE_CURVE_WITH_KNOTS ( 'NONE', 3,
 ( #8104, #12957, #284, #10455 ),
 .UNSPECIFIED., .F., .F.,
 ( 4, 4 ),
 ( 0.000000000000000000, 0.003022500951957888399 ),
 .UNSPECIFIED. ) ;
#2848 = CIRCLE ( 'NONE', #16148, 7.634842307437897269 ) ;
#2849 = EDGE_LOOP ( 'NONE', ( #19340, #11154, #3448, #11215 ) ) ;
#2850 = ADVANCED_FACE ( 'NONE', ( #27814 ), #30509, .T. ) ;
#2851 = CONICAL_SURFACE ( 'NONE', #15637, 8.000000000000000000, 0.03490658503988666728 ) ;
#2852 = CARTESIAN_POINT ( 'NONE',  ( -8.000050800000003903, -2.998651111664708324, 0.1685590755062153223 ) ) ;
#2853 = CARTESIAN_POINT ( 'NONE',  ( -55.59999999999999432, -10.96966150227468972, 7.500000000000000000 ) ) ;
#2854 = CARTESIAN_POINT ( 'NONE',  ( -50.81000000000000227, -10.96999999999998643, 9.000000000000000000 ) ) ;
#2855 = AXIS2_PLACEMENT_3D ( 'NONE', #31834, #3919, #14096 ) ;
#2856 = CARTESIAN_POINT ( 'NONE',  ( 12.16192611266111712, -15.44737063921108700, -1.499999999999999778 ) ) ;
#2858 = ORIENTED_EDGE ( 'NONE', *, *, #29718, .F. ) ;
#2857 = CARTESIAN_POINT ( 'NONE',  ( 108.2963982961846199, 19.82862259121970183, -2.249089808652653399 ) ) ;
#2859 = CARTESIAN_POINT ( 'NONE',  ( -6.962550801365593678, 2.228590825266444142, 2.752080473201636845 ) ) ;
#2860 = CARTESIAN_POINT ( 'NONE',  ( -41.86373177837819526, -16.13513036599590222, 5.128141679950119602 ) ) ;
#2861 = EDGE_CURVE ( 'NONE', #15674, #4058, #6388, .T. ) ;
#2862 = TOROIDAL_SURFACE ( 'NONE', #25799, 11.18125977723849296, 0.5000000000000000000 ) ;
#2863 = DIRECTION ( 'NONE',  ( -1.000000000000000000, 0.000000000000000000, -0.000000000000000000 ) ) ;
#2864 = CARTESIAN_POINT ( 'NONE',  ( 108.6457025336241031, 16.11621187055573046, 2.334455007174216057 ) ) ;
#2865 = AXIS2_PLACEMENT_3D ( 'NONE', #14796, #7619, #2104 ) ;
#2866 = ORIENTED_EDGE ( 'NONE', *, *, #23981, .F. ) ;
#2867 = ORIENTED_EDGE ( 'NONE', *, *, #25337, .F. ) ;
#2868 = CIRCLE ( 'NONE', #29990, 0.4999999999999997780 ) ;
#2869 = DIRECTION ( 'NONE',  ( 0.000000000000000000, 0.000000000000000000, 1.000000000000000000 ) ) ;
#2870 = CARTESIAN_POINT ( 'NONE',  ( -3.688478485700421711E-13, 5.227991826304162259, -9.620177616658798669 ) ) ;
#2871 = ADVANCED_FACE ( 'NONE', ( #4600 ), #24973, .F. ) ;
#2872 = ADVANCED_FACE ( 'NONE', ( #20148 ), #25137, .F. ) ;
#2873 = DIRECTION ( 'NONE',  ( -1.000000000000000000, 0.000000000000000000, 0.000000000000000000 ) ) ;
#2874 = CARTESIAN_POINT ( 'NONE',  ( 17.39502519979085449, -21.04076415203812189, -1.751145182513948573 ) ) ;
#2875 = AXIS2_PLACEMENT_3D ( 'NONE', #28041, #30378, #4975 ) ;
#2876 = DIRECTION ( 'NONE',  ( -1.000000000000000000, 0.000000000000000000, 0.000000000000000000 ) ) ;
#2877 = PRODUCT_DEFINITION_SHAPE ( 'NONE', 'NONE',  #21105 ) ;
#2878 = AXIS2_PLACEMENT_3D ( 'NONE', #8627, #18170, #10644 ) ;
#2879 = FACE_OUTER_BOUND ( 'NONE', #1499, .T. ) ;
#2880 = CARTESIAN_POINT ( 'NONE',  ( 41.35640441664088485, -8.240600375908496034, 1.529340244835370344 ) ) ;
#2881 = ORIENTED_EDGE ( 'NONE', *, *, #8616, .F. ) ;
#2882 = DIRECTION ( 'NONE',  ( -1.000000000000000000, 0.000000000000000000, 0.000000000000000000 ) ) ;
#2883 = AXIS2_PLACEMENT_3D ( 'NONE', #4618, #14793, #22826 ) ;
#2884 = AXIS2_PLACEMENT_3D ( 'NONE', #10025, #7514, #4189 ) ;
#2885 = DIRECTION ( 'NONE',  ( 1.000000000000000000, 0.000000000000000000, 0.000000000000000000 ) ) ;
#2887 = CARTESIAN_POINT ( 'NONE',  ( 0.000000000000000000, -5.979767908488853756, 1.814490771706161132 ) ) ;
#2886 = LOCAL_TIME ( 16, 7, 10.00000000000000000, #23888 ) ;
#2888 = ORIENTED_EDGE ( 'NONE', *, *, #16398, .F. ) ;
#2889 = EDGE_CURVE ( 'NONE', #13391, #8881, #22661, .T. ) ;
#2890 = CARTESIAN_POINT ( 'NONE',  ( 0.000000000000000000, 0.000000000000000000, 0.000000000000000000 ) ) ;
#2891 = ORIENTED_EDGE ( 'NONE', *, *, #2472, .T. ) ;
#2892 = CARTESIAN_POINT ( 'NONE',  ( -17.54156717296799783, 14.33342533202398705, 1.873879510985751118 ) ) ;
#2894 = EDGE_LOOP ( 'NONE', ( #17490, #29724, #32738, #4422, #31929 ) ) ;
#2893 = CARTESIAN_POINT ( 'NONE',  ( 40.88018956639172075, -6.197502223141884592, -4.312042181581901445 ) ) ;
#2895 = ORIENTED_EDGE ( 'NONE', *, *, #7336, .T. ) ;
#2896 = DIRECTION ( 'NONE',  ( -0.000000000000000000, -1.000000000000000000, -0.000000000000000000 ) ) ;
#2897 = CARTESIAN_POINT ( 'NONE',  ( 7.249760686538667009, -1.391664247347174754, -7.892520144992448472 ) ) ;
#2898 = CARTESIAN_POINT ( 'NONE',  ( 26.17249999999999943, 1.291182301015469047, 2.378061970571981654 ) ) ;
#2899 = DIRECTION ( 'NONE',  ( 0.000000000000000000, 0.08715574274765046370, 0.9961946980917462113 ) ) ;
#2900 = EDGE_CURVE ( 'NONE', #4203, #28083, #13845, .T. ) ;
#2902 = VERTEX_POINT ( 'NONE', #9933 ) ;
#2901 = CARTESIAN_POINT ( 'NONE',  ( 7.249760686538667009, 7.953573330858264789, -3.647351267791489882 ) ) ;
#2903 = VECTOR ( 'NONE', #11574, 1000.000000000000227 ) ;
#2904 = LINE ( 'NONE', #10701, #26321 ) ;
#2905 = CARTESIAN_POINT ( 'NONE',  ( 25.25107927536528507, 18.67207037203893094, 1.499999999999350075 ) ) ;
#2906 = CARTESIAN_POINT ( 'NONE',  ( -1.112475574502160613, -13.84051535357300011, 1.744598623382826785 ) ) ;
#2907 = CARTESIAN_POINT ( 'NONE',  ( 23.04750000136559862, -3.024605502323851169, 0.3178988483021052969 ) ) ;
#2908 = VECTOR ( 'NONE', #28633, 1000.000000000000227 ) ;
#2909 = CARTESIAN_POINT ( 'NONE',  ( 10.00000000000000000, 3.993798362933308255, 3.024842911000705570 ) ) ;
#2911 = ORIENTED_EDGE ( 'NONE', *, *, #161, .F. ) ;
#2910 = DIRECTION ( 'NONE',  ( 0.000000000000000000, 0.000000000000000000, 1.000000000000000000 ) ) ;
#2912 = CARTESIAN_POINT ( 'NONE',  ( 0.6708088701982989344, 0.000000000000000000, 4.629213727441584325 ) ) ;
#2913 = VECTOR ( 'NONE', #8060, 1000.000000000000000 ) ;
#2914 = CARTESIAN_POINT ( 'NONE',  ( -23.77648227443687290, 18.46223496596753577, 1.773004750130224627 ) ) ;
#2915 = CARTESIAN_POINT ( 'NONE',  ( 25.11000000273118715, 1.573300977624590313, -1.942864903642426144 ) ) ;
#2916 = EDGE_CURVE ( 'NONE', #6454, #24800, #9340, .T. ) ;
#2917 = LOCAL_TIME ( 16, 7, 10.00000000000000000, #32767 ) ;
#2918 = EDGE_CURVE ( 'NONE', #19057, #19567, #17112, .T. ) ;
#2919 = DIRECTION ( 'NONE',  ( -1.000000000000000000, 0.000000000000000000, 0.000000000000000000 ) ) ;
#2920 = CARTESIAN_POINT ( 'NONE',  ( 6.356382399260308347, 7.150437133400997070, -4.790388219480488097 ) ) ;
#2921 = LINE ( 'NONE', #30825, #15073 ) ;
#2922 = ORIENTED_EDGE ( 'NONE', *, *, #491, .F. ) ;
#2923 = LINE ( 'NONE', #20455, #20451 ) ;
#2924 = LINE ( 'NONE', #29267, #4429 ) ;
#2925 = EDGE_LOOP ( 'NONE', ( #6215, #27122, #18110, #31968 ) ) ;
#2926 = VECTOR ( 'NONE', #12888, 1000.000000000000114 ) ;
#2927 = FACE_OUTER_BOUND ( 'NONE', #14693, .T. ) ;
#2928 = CARTESIAN_POINT ( 'NONE',  ( -2.976978444279338110, -0.1588929671266211263, -1.367460996489382685 ) ) ;
#2929 = CARTESIAN_POINT ( 'NONE',  ( 71.67787245194618606, -18.34520463695562498, -1.500000000000000444 ) ) ;
#2931 = CARTESIAN_POINT ( 'NONE',  ( 107.4498065544417500, -17.35655240063459104, 4.512182935183896682 ) ) ;
#2930 = DIRECTION ( 'NONE',  ( 0.000000000000000000, 1.776356839400250149E-14, 1.000000000000000000 ) ) ;
#2932 = ORIENTED_EDGE ( 'NONE', *, *, #5346, .T. ) ;
#2933 = EDGE_CURVE ( 'NONE', #10256, #23098, #19802, .T. ) ;
#2934 = B_SPLINE_CURVE_WITH_KNOTS ( 'NONE', 3,
 ( #5812, #31083, #10838, #16176, #28719, #6153, #13803, #18525, #15992, #26403 ),
 .UNSPECIFIED., .F., .F.,
 ( 4, 2, 2, 2, 4 ),
 ( 3.032460776720355987E-07, 0.0005479053915603968516, 0.001095507537043121683, 0.001643109682525846190, 0.002190711828008571130 ),
 .UNSPECIFIED. ) ;
#2935 = CC_DESIGN_PERSON_AND_ORGANIZATION_ASSIGNMENT ( #11798, #11985, ( #26379 ) ) ;
#2936 = LINE ( 'NONE', #28291, #9609 ) ;
#2937 = ORIENTED_EDGE ( 'NONE', *, *, #5783, .T. ) ;
#2938 = CARTESIAN_POINT ( 'NONE',  ( 2.976845687893346248, 0.5490754078163789798, -9.149921655307444723 ) ) ;
#2940 = ORIENTED_EDGE ( 'NONE', *, *, #26592, .T. ) ;
#2939 = LINE ( 'NONE', #547, #28823 ) ;
#2941 = ORIENTED_EDGE ( 'NONE', *, *, #24401, .F. ) ;
#2942 = LINE ( 'NONE', #33007, #26755 ) ;
#2943 = ORGANIZATION ( 'NAUO-ORG2', 'UNSPECIFIED', 'UNSPECIFIED' ) ;
#2944 = CARTESIAN_POINT ( 'NONE',  ( 0.7632845268398871230, 0.000000000000000000, 0.000000000000000000 ) ) ;
#2946 = ORIENTED_EDGE ( 'NONE', *, *, #6096, .F. ) ;
#2945 = CARTESIAN_POINT ( 'NONE',  ( 7.249760686538667009, 5.151476664237477188, 6.139290821770273077 ) ) ;
#2947 = ORIENTED_EDGE ( 'NONE', *, *, #31869, .T. ) ;
#2948 = CARTESIAN_POINT ( 'NONE',  ( 0.2098061928526393227, -5.473028564773644966, -1.769944308764095586 ) ) ;
#2949 = DIRECTION ( 'NONE',  ( -1.000000000000000000, 0.000000000000000000, 0.000000000000000000 ) ) ;
#2950 = CARTESIAN_POINT ( 'NONE',  ( -50.60000000000000142, -10.96966150227468972, 7.500000000000000000 ) ) ;
#2951 = CYLINDRICAL_SURFACE ( 'NONE', #22433, 302.6457063863960002 ) ;
#2952 = DIRECTION ( 'NONE',  ( -1.000000000000000000, 0.000000000000000000, 0.000000000000000000 ) ) ;
#2953 = EDGE_CURVE ( 'NONE', #20898, #8159, #202, .T. ) ;
#2954 = AXIS2_PLACEMENT_3D ( 'NONE', #15966, #309, #26187 ) ;
#2955 = FACE_OUTER_BOUND ( 'NONE', #12591, .T. ) ;
#2956 = DIRECTION ( 'NONE',  ( -1.000000000000000000, 8.574039729943017111E-17, -0.000000000000000000 ) ) ;
#2957 = CARTESIAN_POINT ( 'NONE',  ( 69.10820754288468493, -6.866680491177692858, 2.787783121302774170 ) ) ;
#2958 = CARTESIAN_POINT ( 'NONE',  ( 0.000000000000000000, 0.000000000000000000, 0.000000000000000000 ) ) ;
#2959 = CARTESIAN_POINT ( 'NONE',  ( 3.393608999705025386, -0.06500480712391917826, 1.255126411524221997 ) ) ;
#2960 = CARTESIAN_POINT ( 'NONE',  ( 5.887530252753766291, -5.676096663009846388, 6.185189124321802012 ) ) ;
#2961 = LOCAL_TIME ( 16, 7, 10.00000000000000000, #1750 ) ;
#2962 = CARTESIAN_POINT ( 'NONE',  ( 85.25075202023808174, -3.924039320687066290, 5.695980980372492120 ) ) ;
#2963 = CARTESIAN_POINT ( 'NONE',  ( 0.000000000000000000, 7.958834565716766285, 7.593217523260605617 ) ) ;
#2964 = ORIENTED_EDGE ( 'NONE', *, *, #3466, .T. ) ;
#2965 = CARTESIAN_POINT ( 'NONE',  ( -6.237550801365593145, 1.088641768524161613, 3.675193018007247403 ) ) ;
#2966 = CARTESIAN_POINT ( 'NONE',  ( -2.500050802731187627, -1.549418761218565255, 2.853674364686380471 ) ) ;
#2967 = CARTESIAN_POINT ( 'NONE',  ( 10.00000000000000178, -8.574039729943018837E-16, 0.000000000000000000 ) ) ;
#2968 = VERTEX_POINT ( 'NONE', #7265 ) ;
#2969 = DIRECTION ( 'NONE',  ( 0.1437473352845032581, 0.000000000000000000, -0.9896144216807900573 ) ) ;
#2970 = CIRCLE ( 'NONE', #17354, 3.000000000000000444 ) ;
#2971 = B_SPLINE_CURVE_WITH_KNOTS ( 'NONE', 3,
 ( #25547, #30258, #17687, #12521, #23225, #32772, #9850, #12672 ),
 .UNSPECIFIED., .F., .F.,
 ( 4, 2, 2, 4 ),
 ( 5.099451029798776812E-07, 0.001229189835658058482, 0.001843529780935597657, 0.002457869726213138782 ),
 .UNSPECIFIED. ) ;
#2972 = ORIENTED_EDGE ( 'NONE', *, *, #12144, .T. ) ;
#2973 = DIRECTION ( 'NONE',  ( -1.000000000000000000, 0.000000000000000000, 0.000000000000000000 ) ) ;
#2974 = CALENDAR_DATE ( 2026, 6, 10 ) ;
#2976 = VERTEX_POINT ( 'NONE', #3246 ) ;
#2975 = CARTESIAN_POINT ( 'NONE',  ( -2.223027892448373066, -2.927336879246196677, -4.522129901861166701 ) ) ;
#2977 = ORIENTED_EDGE ( 'NONE', *, *, #28566, .T. ) ;
#2978 = CARTESIAN_POINT ( 'NONE',  ( -50.59999999999987352, -21.43932300454937945, 1.000000000000000000 ) ) ;
#2979 = ORIENTED_EDGE ( 'NONE', *, *, #3895, .T. ) ;
#2980 = CARTESIAN_POINT ( 'NONE',  ( -1.773875666770781789, -0.3178988483021056854, 3.024605502323848949 ) ) ;
#2982 = ORIENTED_EDGE ( 'NONE', *, *, #8207, .F. ) ;
#2981 = CARTESIAN_POINT ( 'NONE',  ( -2.438362943428902252, 0.3722612527041059827, 3.133914954463516533 ) ) ;
#2983 = CARTESIAN_POINT ( 'NONE',  ( 12.16606561763909156, 4.796759898857955839, 1.050000000000000266 ) ) ;
#2984 = CARTESIAN_POINT ( 'NONE',  ( 108.1144640473778082, -19.71761592378730299, 1.808523936579597535 ) ) ;
#2985 = EDGE_CURVE ( 'NONE', #264, #2193, #25829, .T. ) ;
#2986 = CARTESIAN_POINT ( 'NONE',  ( 25.75999999999999801, -2.208672634433321348E-15, 0.000000000000000000 ) ) ;
#2987 = DIRECTION ( 'NONE',  ( 6.062761635205572056E-17, 0.7071067811865465735, -0.7071067811865484609 ) ) ;
#2988 = EDGE_CURVE ( 'NONE', #10930, #1782, #15785, .T. ) ;
#2989 = ORIENTED_EDGE ( 'NONE', *, *, #3881, .F. ) ;
#2990 = EDGE_CURVE ( 'NONE', #5275, #660, #22414, .T. ) ;
#2991 = DIRECTION ( 'NONE',  ( 0.000000000000000000, 0.5877852522924689183, 0.8090169943749504489 ) ) ;
#2992 = DIRECTION ( 'NONE',  ( 1.000000000000000000, -8.574039729943018344E-17, -0.000000000000000000 ) ) ;
#2993 = CARTESIAN_POINT ( 'NONE',  ( 102.5019105821285024, -5.123465467906981985, -2.184956770195078057 ) ) ;
#2994 = DIRECTION ( 'NONE',  ( 0.000000000000000000, -0.8191520442889951292, 0.5735764363510413855 ) ) ;
#2995 = CARTESIAN_POINT ( 'NONE',  ( 23.22564588060106772, -21.93932300456763329, 1.010482627728501948 ) ) ;
#2996 = PLANE ( 'NONE',  #31604 ) ;
#2997 = CARTESIAN_POINT ( 'NONE',  ( 23.92250000000000298, 2.378061970571979433, -1.291182301015470602 ) ) ;
#2998 = CARTESIAN_POINT ( 'NONE',  ( 3.249999999999999556, 0.4999240074895661690, -8.734705317681621395 ) ) ;
#2999 = ORIENTED_EDGE ( 'NONE', *, *, #26390, .T. ) ;
#3000 = CARTESIAN_POINT ( 'NONE',  ( -4.312550801365593323, -3.675193018007246071, 1.088641768524163167 ) ) ;
#3001 = ORIENTED_EDGE ( 'NONE', *, *, #30795, .T. ) ;
#3002 = CARTESIAN_POINT ( 'NONE',  ( -8.300050799999999285, 2.983565686104819648, 0.3135853898029609677 ) ) ;
#3003 = CARTESIAN_POINT ( 'NONE',  ( 110.2875796713736634, 19.60135708372762409, -5.471072653611070535 ) ) ;
#3004 = DIRECTION ( 'NONE',  ( -1.000000000000000000, -0.000000000000000000, -0.000000000000000000 ) ) ;
#3005 = CARTESIAN_POINT ( 'NONE',  ( 13.85437446117657068, -14.51384729146047547, 1.500000000000000000 ) ) ;
#3006 = EDGE_LOOP ( 'NONE', ( #2724, #5127, #7346, #7588, #3939 ) ) ;
#3007 = CARTESIAN_POINT ( 'NONE',  ( 102.2915521900156079, -2.105775436100236764, -2.787782622536843835 ) ) ;
#3008 =( BOUNDED_CURVE ( )  B_SPLINE_CURVE ( 3, ( #22851, #25523, #7646, #30232 ),
 .UNSPECIFIED., .F., .F. ) 
 B_SPLINE_CURVE_WITH_KNOTS ( ( 4, 4 ),
 ( 4.712388980384689674, 6.457718232379018097 ),
 .UNSPECIFIED. ) 
 CURVE ( )  GEOMETRIC_REPRESENTATION_ITEM ( )  RATIONAL_B_SPLINE_CURVE ( ( 1.000000000000000000, 0.7618584064576930936, 0.7618584064576930936, 1.000000000000000000 ) ) 
 REPRESENTATION_ITEM ( '' )  );
#3009 = ORIENTED_EDGE ( 'NONE', *, *, #8201, .T. ) ;
#3010 = CARTESIAN_POINT ( 'NONE',  ( 0.6728001046013577513, 8.512517952453869441, 3.357496170308674976 ) ) ;
#3011 = DATE_AND_TIME ( #13164, #3962 ) ;
#3012 = CARTESIAN_POINT ( 'NONE',  ( 54.97666862915123431, -6.486485553567831630, 4.023790190276410605 ) ) ;
#3013 = EDGE_CURVE ( 'NONE', #29829, #20134, #17612, .T. ) ;
#3014 = DIRECTION ( 'NONE',  ( 1.000000000000000000, 7.164576672270377148E-15, 0.000000000000000000 ) ) ;
#3015 = CARTESIAN_POINT ( 'NONE',  ( 25.75999999999999801, -2.208672634433321348E-15, 0.000000000000000000 ) ) ;
#3016 = VERTEX_POINT ( 'NONE', #12932 ) ;
#3017 = CARTESIAN_POINT ( 'NONE',  ( 3.499999999999999556, 0.005878491403456947983, 7.047692205288324629 ) ) ;
#3018 = CARTESIAN_POINT ( 'NONE',  ( -18.30155664144426453, 0.000000000000000000, 0.000000000000000000 ) ) ;
#3019 = CARTESIAN_POINT ( 'NONE',  ( 9.350000000000001421, 0.000000000000000000, 1.000000000000000000 ) ) ;
#3021 = ORIENTED_EDGE ( 'NONE', *, *, #24403, .F. ) ;
#3020 = CARTESIAN_POINT ( 'NONE',  ( 9.282537329959909655, 0.2172754300399158400, -1.041239158277187160 ) ) ;
#3022 = CARTESIAN_POINT ( 'NONE',  ( -5.062550801365593323, -3.521866450007987037, -0.3701630799359323931 ) ) ;
#3023 = CARTESIAN_POINT ( 'NONE',  ( -53.95513674679793326, 5.522463357794191730, 1.050000000000049116 ) ) ;
#3024 = CARTESIAN_POINT ( 'NONE',  ( 35.27967220683370186, -7.797546999713141247, -2.184956776474153095 ) ) ;
#3025 = VERTEX_POINT ( 'NONE', #23154 ) ;
#3026 = ORIENTED_EDGE ( 'NONE', *, *, #25928, .T. ) ;
#3027 = CARTESIAN_POINT ( 'NONE',  ( 108.6181628067467386, 15.96285980464529786, -2.043459231428901735 ) ) ;
#3028 = CARTESIAN_POINT ( 'NONE',  ( 3.063284526839889832, 3.174628368996186278, -8.152713396088721254 ) ) ;
#3029 = CARTESIAN_POINT ( 'NONE',  ( 20.98500000136559862, -0.9349337715887247047, 3.156283516753367824 ) ) ;
#3030 = CARTESIAN_POINT ( 'NONE',  ( 3.499999999999999556, 7.008469740302802897, 0.7425307242148009301 ) ) ;
#3031 = CARTESIAN_POINT ( 'NONE',  ( -0.2059365608663963898, 0.000000000000000000, 1.000000000000000000 ) ) ;
#3032 = DIRECTION ( 'NONE',  ( 1.000000000000000000, 0.000000000000000000, 0.000000000000000000 ) ) ;
#3033 = CARTESIAN_POINT ( 'NONE',  ( 47.95865874067742141, -8.381244160377555374, 0.8105615599371254199 ) ) ;
#3034 = VERTEX_POINT ( 'NONE', #20967 ) ;
#3035 = CARTESIAN_POINT ( 'NONE',  ( 10.00000000000000178, 0.2500000000000544564, -5.003758587302146843 ) ) ;
#3036 = EDGE_CURVE ( 'NONE', #2248, #18257, #22962, .T. ) ;
#3037 = ADVANCED_FACE ( 'NONE', ( #8267 ), #31792, .T. ) ;
#3038 = MECHANICAL_CONTEXT ( 'NONE', #16282, 'mechanical' ) ;
#3039 = CARTESIAN_POINT ( 'NONE',  ( 68.71221462755966058, -6.131929330191479899, -3.993435576825361100 ) ) ;
#3040 = ORIENTED_EDGE ( 'NONE', *, *, #19183, .F. ) ;
#3041 = DIRECTION ( 'NONE',  ( -0.000000000000000000, 0.000000000000000000, 1.000000000000000000 ) ) ;
#3042 = ORIENTED_EDGE ( 'NONE', *, *, #13464, .F. ) ;
#3043 = CARTESIAN_POINT ( 'NONE',  ( -17.72558274912641352, 7.737767392030566072, 2.044195425586785575 ) ) ;
#3045 = EDGE_LOOP ( 'NONE', ( #10017, #26499, #8500, #2922 ) ) ;
#3044 = CARTESIAN_POINT ( 'NONE',  ( 54.96134875814583154, -5.932951279955770651, -4.312042181584450518 ) ) ;
#3046 = VERTEX_POINT ( 'NONE', #28500 ) ;
#3047 = EDGE_CURVE ( 'NONE', #4554, #11141, #15487, .T. ) ;
#3048 = EDGE_CURVE ( 'NONE', #21704, #31255, #23452, .T. ) ;
#3049 = CARTESIAN_POINT ( 'NONE',  ( 41.56220206658399263, -20.97620094567151838, -4.522129901861164925 ) ) ;
#3050 = CARTESIAN_POINT ( 'NONE',  ( 0.6728002192067955578, 5.823680980834268439, -7.058361986476028527 ) ) ;
#3051 = LINE ( 'NONE', #18717, #26840 ) ;
#3052 = CARTESIAN_POINT ( 'NONE',  ( 48.09670199522224721, -9.430894477034977186, -0.07017451552783579571 ) ) ;
#3054 = ORIENTED_EDGE ( 'NONE', *, *, #1620, .T. ) ;
#3053 = DIRECTION ( 'NONE',  ( 0.1908089953765454150, 4.257129299459132156E-16, -0.9816271834476638647 ) ) ;
#3055 = CARTESIAN_POINT ( 'NONE',  ( 10.43095328441111924, 21.14375246189590030, 1.508259000770582059 ) ) ;
#3056 = DIRECTION ( 'NONE',  ( -1.000000000000000000, 0.000000000000000000, 0.000000000000000000 ) ) ;
#3057 = CARTESIAN_POINT ( 'NONE',  ( 2.087651665455726224, -16.81471312933366136, 1.500000000000000444 ) ) ;
#3058 = LINE ( 'NONE', #13853, #1728 ) ;
#3059 = CARTESIAN_POINT ( 'NONE',  ( 3.093679806470314819, -0.1913619822784919933, 1.398088436977038107 ) ) ;
#3062 = EDGE_CURVE ( 'NONE', #16944, #30215, #25692, .T. ) ;
#3061 = ORIENTED_EDGE ( 'NONE', *, *, #5068, .F. ) ;
#3060 = CARTESIAN_POINT ( 'NONE',  ( 7.249760686538667009, -4.973063321323927255, 7.199384779417104419 ) ) ;
#3063 = FACE_OUTER_BOUND ( 'NONE', #13917, .T. ) ;
#3064 = B_SPLINE_CURVE_WITH_KNOTS ( 'NONE', 3,
 ( #6470, #26888, #29885, #1826, #12008, #6968, #32567, #19534, #14315, #1481, #1983, #24512 ),
 .UNSPECIFIED., .F., .F.,
 ( 4, 2, 2, 2, 2, 4 ),
 ( 8.673617379884035472E-19, 7.411273891762962317E-05, 0.0001482254778352583790, 0.0002964509556705158906, 0.0005929019113410210476, 0.001185803822682031470 ),
 .UNSPECIFIED. ) ;
#3065 = CARTESIAN_POINT ( 'NONE',  ( -27.17337974022411373, 17.29073355517597221, 1.801206419975863504 ) ) ;
#3066 = CARTESIAN_POINT ( 'NONE',  ( 22.29750000136559507, -0.3178988483021076838, -3.024605502323848949 ) ) ;
#3067 = CARTESIAN_POINT ( 'NONE',  ( 0.000000000000000000, -2.652816298622381996, -5.657964889053610058 ) ) ;
#3068 = ADVANCED_FACE ( 'NONE', ( #26138 ), #5532, .T. ) ;
#3069 = CARTESIAN_POINT ( 'NONE',  ( 18.65791233782715963, -7.001076235476726417, -2.184956778830003277 ) ) ;
#3070 = CARTESIAN_POINT ( 'NONE',  ( 28.60502136297058229, -6.760022240753575495, 3.993434336043301336 ) ) ;
#3071 = VERTEX_POINT ( 'NONE', #25282 ) ;
#3072 = DIRECTION ( 'NONE',  ( 0.4809547266710044178, 0.000000000000000000, 0.8767454310646958238 ) ) ;
#3073 = B_SPLINE_SURFACE_WITH_KNOTS ( 'NONE', 1, 3, ( 
 ( #5552, #12560, #25434, #30453, #17740, #20428, #12712, #25588, #1761, #2543, #17916, #11956, #28107, #30806, #27759, #5205 ),
 ( #27947, #19639, #10390, #23262, #7874, #15381, #2699, #5054, #22152, #25271, #10040, #6911, #17107, #12870, #20750, #22764 ) ),
 .UNSPECIFIED., .F., .F., .F.,
 ( 2, 2 ),
 ( 4, 2, 2, 2, 2, 2, 2, 4 ),
 ( 0.000000000000000000, 1.000000000000000000 ),
 ( 0.000000000000000000, 0.5000000000000000000, 0.6250000000000000000, 0.7500000000000000000, 0.8125000000000000000, 0.8750000000000000000, 0.9375000000000000000, 1.000000000000000000 ),
 .UNSPECIFIED. ) ;
#3074 = CARTESIAN_POINT ( 'NONE',  ( 0.000000000000000000, 2.871924938129881699, 6.435996203144517480 ) ) ;
#3075 = ORIENTED_EDGE ( 'NONE', *, *, #26835, .F. ) ;
#3076 = DIRECTION ( 'NONE',  ( 1.000000000000000000, 0.000000000000000000, 0.000000000000000000 ) ) ;
#3077 = CARTESIAN_POINT ( 'NONE',  ( 5.612718622971679672, -7.786491723834097378, -2.621884781721345092 ) ) ;
#3078 = CARTESIAN_POINT ( 'NONE',  ( 0.4474568012433098874, -7.410208993127078259, -0.9788672205888330202 ) ) ;
#3080 = CARTESIAN_POINT ( 'NONE',  ( 107.9510094122608734, -17.36390984048267327, 4.614126556756068531 ) ) ;
#3079 = CARTESIAN_POINT ( 'NONE',  ( 25.43628654896178176, -17.54453578616395149, 1.000000000000000000 ) ) ;
#3081 = EDGE_LOOP ( 'NONE', ( #17559, #1353, #25116, #19800 ) ) ;
#3082 = CARTESIAN_POINT ( 'NONE',  ( -4.900050799999999818, -0.3135853898029607456, 2.983565686104819648 ) ) ;
#3083 = ORIENTED_EDGE ( 'NONE', *, *, #25966, .T. ) ;
#3084 = CARTESIAN_POINT ( 'NONE',  ( 2.589202797589366334, 1.003524335601164497, -10.26630467377257538 ) ) ;
#3086 = VERTEX_POINT ( 'NONE', #4566 ) ;
#3085 = DIRECTION ( 'NONE',  ( 1.000000000000000000, 0.000000000000000000, 0.000000000000000000 ) ) ;
#3087 = EDGE_LOOP ( 'NONE', ( #31399, #11921, #26994, #23042, #9489, #893, #6213, #18000, #28377 ) ) ;
#3088 = LINE ( 'NONE', #13245, #19881 ) ;
#3089 = EDGE_CURVE ( 'NONE', #11534, #4598, #24939, .T. ) ;
#3090 = EDGE_CURVE ( 'NONE', #20203, #3086, #3220, .T. ) ;
#3091 = DIRECTION ( 'NONE',  ( 0.000000000000000000, 0.4226182617407045483, -0.9063077870366476052 ) ) ;
#3093 = ORIENTED_EDGE ( 'NONE', *, *, #7486, .F. ) ;
#3092 = CARTESIAN_POINT ( 'NONE',  ( -2.506063600758156262, 0.4999999999999998890, -1.500000000000000000 ) ) ;
#3094 = ORIENTED_EDGE ( 'NONE', *, *, #7936, .F. ) ;
#3095 = CARTESIAN_POINT ( 'NONE',  ( -5.700050800000000528, -0.3135853898029607456, 2.983565686104819648 ) ) ;
#3096 = DIRECTION ( 'NONE',  ( -1.000000000000000000, 0.000000000000000000, -0.000000000000000000 ) ) ;
#3097 = CARTESIAN_POINT ( 'NONE',  ( -30.19127229040104865, 4.968489494181039134, 5.500000000000000000 ) ) ;
#3098 = LINE ( 'NONE', #8083, #20841 ) ;
#3099 = LINE ( 'NONE', #15929, #23164 ) ;
#3100 = DIRECTION ( 'NONE',  ( -3.623545766764251600E-17, -0.4226182617407038267, 0.9063077870366479383 ) ) ;
#3101 = CARTESIAN_POINT ( 'NONE',  ( 0.6161739807942353542, -5.543681800203635213, 1.499999999999999778 ) ) ;
#3102 = CARTESIAN_POINT ( 'NONE',  ( 23.66826818115504238, -7.072331084924259770, 2.787782631216866758 ) ) ;
#3103 = EDGE_CURVE ( 'NONE', #22148, #1082, #26678, .T. ) ;
#3104 = CARTESIAN_POINT ( 'NONE',  ( 2.274274201625327230, 0.000000000000000000, 0.000000000000000000 ) ) ;
#3105 = CARTESIAN_POINT ( 'NONE',  ( 2.632061376486628301, -0.4999999999999992784, 1.500000000000000444 ) ) ;
#3106 = CC_DESIGN_PERSON_AND_ORGANIZATION_ASSIGNMENT ( #17098, #26988, ( #25875 ) ) ;
#3107 = EDGE_LOOP ( 'NONE', ( #12674, #26991, #18510, #12080 ) ) ;
#3108 = CARTESIAN_POINT ( 'NONE',  ( 0.000000000000000000, -7.009698679648292519, 3.730838147389666126 ) ) ;
#3109 = CARTESIAN_POINT ( 'NONE',  ( 18.93617721851659041, -3.890633339435721982, 4.522129901861162260 ) ) ;
#3110 = LINE ( 'NONE', #13265, #4434 ) ;
#3111 = ORIENTED_EDGE ( 'NONE', *, *, #3176, .T. ) ;
#3112 = CARTESIAN_POINT ( 'NONE',  ( 23.61000000136559507, 2.892927487894327410, -1.570731468192931635 ) ) ;
#3113 = CARTESIAN_POINT ( 'NONE',  ( -2.350050802731187272, -2.983565686104819648, -0.3135853898029605791 ) ) ;
#3114 = CARTESIAN_POINT ( 'NONE',  ( 19.72213158284597867, -21.49998897973801704, -1.523512165874404189 ) ) ;
#3115 = ORIENTED_EDGE ( 'NONE', *, *, #13688, .F. ) ;
#3116 = CARTESIAN_POINT ( 'NONE',  ( 26.20274081918675435, 20.47280333234591154, 4.999054092451758358 ) ) ;
#3117 = ADVANCED_FACE ( 'NONE', ( #2051 ), #19759, .T. ) ;
#3118 = EDGE_LOOP ( 'NONE', ( #21825, #14725, #14773, #24968 ) ) ;
#3119 = DIRECTION ( 'NONE',  ( 1.000000000000000000, 0.000000000000000000, 0.000000000000000000 ) ) ;
#3120 = SECURITY_CLASSIFICATION_LEVEL ( 'unclassified' ) ;
#3122 = ORIENTED_EDGE ( 'NONE', *, *, #22115, .F. ) ;
#3121 = DIRECTION ( 'NONE',  ( 1.000000000000000000, -8.574039729943018344E-17, -0.000000000000000000 ) ) ;
#3123 = ORIENTED_EDGE ( 'NONE', *, *, #1288, .T. ) ;
#3124 = DIRECTION ( 'NONE',  ( 0.000000000000000000, 0.000000000000000000, 1.000000000000000000 ) ) ;
#3125 = EDGE_LOOP ( 'NONE', ( #11539, #1171, #30153, #4557, #22792, #21877, #19127, #29576, #2386, #23598, #20895, #1473, #5775, #31632, #16603, #31539, #9229, #31468, #24458, #29399, #13134, #1272, #8593, #21645, #676, #23607, #26554, #12686, #15520, #23753, #20477, #4167, #13745, #31599, #23372, #26961, #5485, #11854, #26760, #2932, #627, #13449, #18862, #24194, #33073, #17565 ) ) ;
#3126 = CARTESIAN_POINT ( 'NONE',  ( 10.00000000000000000, 3.641590349731970822, -3.055657119358763829 ) ) ;
#3128 = EDGE_LOOP ( 'NONE', ( #4427, #19266, #16434, #22226 ) ) ;
#3127 = CARTESIAN_POINT ( 'NONE',  ( 29.33867311917065379, -3.750126786195063122, -0.8105614676216158498 ) ) ;
#3129 = CARTESIAN_POINT ( 'NONE',  ( 13.78505948480717436, 7.589837197045443240, 1.050000000000000044 ) ) ;
#3130 = LINE ( 'NONE', #20526, #23978 ) ;
#3131 = CARTESIAN_POINT ( 'NONE',  ( 110.2875796713736918, 19.60135708372767382, 5.471072653610979941 ) ) ;
#3132 = CARTESIAN_POINT ( 'NONE',  ( 4.749760686538667009, 7.530955069117551304, -2.741043480754851380 ) ) ;
#3133 = ORIENTED_EDGE ( 'NONE', *, *, #22371, .F. ) ;
#3134 = CARTESIAN_POINT ( 'NONE',  ( 56.97280603064898941, -277.2763395528616002, 5.471072653610988823 ) ) ;
#3135 = DIRECTION ( 'NONE',  ( -0.000000000000000000, -0.000000000000000000, -1.000000000000000000 ) ) ;
#3136 = PLANE ( 'NONE',  #19811 ) ;
#3137 = PLANE ( 'NONE',  #23723 ) ;
#3138 = CARTESIAN_POINT ( 'NONE',  ( -15.57671159194236488, -25.43932300454937590, 1.499999999999999556 ) ) ;
#3139 = FACE_OUTER_BOUND ( 'NONE', #32296, .T. ) ;
#3140 = CARTESIAN_POINT ( 'NONE',  ( 23.00111451137534502, -1.283275288181523244E-15, -2.499999999999998668 ) ) ;
#3141 = DIRECTION ( 'NONE',  ( 0.000000000000000000, 0.000000000000000000, -1.000000000000000000 ) ) ;
#3142 = CARTESIAN_POINT ( 'NONE',  ( -7.600050802731187716, 3.113457007523260156, -0.9222479816126439855 ) ) ;
#3143 = EDGE_LOOP ( 'NONE', ( #17560, #16753, #924 ) ) ;
#3144 = CARTESIAN_POINT ( 'NONE',  ( -3.254531657079157370, -1.545410377633946286, 2.846291840500174697 ) ) ;
#3145 = DIRECTION ( 'NONE',  ( 2.473959037481232675E-13, 1.000000000000000000, 0.000000000000000000 ) ) ;
#3146 = CARTESIAN_POINT ( 'NONE',  ( -5.050050800000001061, 2.853674364686379583, 1.549418761218565921 ) ) ;
#3147 = CARTESIAN_POINT ( 'NONE',  ( 12.29359088965425784, -13.32350402072020934, 1.000000000000000000 ) ) ;
#3148 = ORIENTED_EDGE ( 'NONE', *, *, #12741, .T. ) ;
#3149 = EDGE_CURVE ( 'NONE', #24117, #11175, #5342, .T. ) ;
#3150 = CARTESIAN_POINT ( 'NONE',  ( 34.92557263839314885, 0.5000000000000000000, -2.487612133692604921 ) ) ;
#3151 = EDGE_CURVE ( 'NONE', #9751, #14334, #16077, .T. ) ;
#3152 = ORIENTED_EDGE ( 'NONE', *, *, #16195, .T. ) ;
#3153 = CARTESIAN_POINT ( 'NONE',  ( 0.000000000000000000, 9.884132761439062165, 4.709950686174647849 ) ) ;
#3154 = EDGE_CURVE ( 'NONE', #28488, #25776, #7467, .T. ) ;
#3155 = DATE_AND_TIME ( #471, #24229 ) ;
#3156 = CARTESIAN_POINT ( 'NONE',  ( 40.88367704618155329, -6.838565261165500786, 4.073741263077431896 ) ) ;
#3157 = CARTESIAN_POINT ( 'NONE',  ( 10.56183597391177464, 4.753758587302147731, 0.000000000000000000 ) ) ;
#3158 = CARTESIAN_POINT ( 'NONE',  ( 3.249999999999999556, 0.000000000000000000, 3.499999999999999556 ) ) ;
#3159 = VERTEX_POINT ( 'NONE', #14890 ) ;
#3160 = CARTESIAN_POINT ( 'NONE',  ( 18.86054332783663767, -4.736068442360261699, 3.993434336035624366 ) ) ;
#3161 = CARTESIAN_POINT ( 'NONE',  ( 25.69812813987159217, 19.01643737707301085, -1.364233426705607322 ) ) ;
#3162 = CARTESIAN_POINT ( 'NONE',  ( 8.694260012178471442, -0.3977034846782490640, 1.500000000000001554 ) ) ;
#3164 = EDGE_LOOP ( 'NONE', ( #16853, #8105, #31208, #7752, #8675 ) ) ;
#3163 = CARTESIAN_POINT ( 'NONE',  ( 108.3358876115613896, 20.04851468097726652, -1.779919050530493152 ) ) ;
#3165 = CARTESIAN_POINT ( 'NONE',  ( -4.212550801365593678, -3.368539882008727115, -1.828967928396028064 ) ) ;
#3166 = CARTESIAN_POINT ( 'NONE',  ( 0.000000000000000000, 0.000000000000000000, 0.000000000000000000 ) ) ;
#3167 = CARTESIAN_POINT ( 'NONE',  ( 41.35325844292879793, -7.141637217093566470, -3.390608916445196908 ) ) ;
#3168 = VERTEX_POINT ( 'NONE', #9900 ) ;
#3169 = ORIENTED_EDGE ( 'NONE', *, *, #27366, .T. ) ;
#3170 = CYLINDRICAL_SURFACE ( 'NONE', #25709, 5.010000000000000675 ) ;
#3171 = DIRECTION ( 'NONE',  ( -0.9896144216807906124, -6.234046928178286825E-16, -0.1437473352845001773 ) ) ;
#3172 = DIRECTION ( 'NONE',  ( 0.000000000000000000, 0.000000000000000000, 1.000000000000000000 ) ) ;
#3173 = DIRECTION ( 'NONE',  ( 0.000000000000000000, 0.000000000000000000, -1.000000000000000000 ) ) ;
#3174 = CARTESIAN_POINT ( 'NONE',  ( 7.249760686538667009, 0.000000000000000000, 0.000000000000000000 ) ) ;
#3175 =( BOUNDED_SURFACE ( )  B_SPLINE_SURFACE ( 3, 3, ( 
 ( #26185, #23979, #11122, #18830, #23345, #6123, #28843, #26659, #21500, #31713, #15823, #451, #10631, #20836, #31050, #13292 ),
 ( #8305, #18498, #15964, #4257, #14273, #3952, #24468, #32374, #27328, #6767, #3769, #31865, #27153, #14624, #8934, #19314 ),
 ( #30016, #19140, #12117, #9587, #16957, #24159, #1588, #14430, #9087, #21658, #4447, #24824, #1770, #11773, #21978, #22312 ),
 ( #16624, #17310, #1283, #14126, #32523, #16806, #13939, #19806, #11464, #1942, #11965, #1437, #32204, #24641, #7107, #29331 ) ),
 .UNSPECIFIED., .F., .F., .F. ) 
 B_SPLINE_SURFACE_WITH_KNOTS ( ( 4, 4 ),
 ( 4, 2, 2, 2, 2, 2, 2, 4 ),
 ( 0.000000000000000000, 1.000000000000000000 ),
 ( 0.000000000000000000, 0.5000000000000000000, 0.6250000000000000000, 0.7500000000000000000, 0.8125000000000000000, 0.8750000000000000000, 0.9375000000000000000, 1.000000000000000000 ),
 .UNSPECIFIED. ) 
 GEOMETRIC_REPRESENTATION_ITEM ( )  RATIONAL_B_SPLINE_SURFACE ( (
 ( 1.000000000000000000, 1.000000000000000000, 1.000000000000000000, 1.000000000000000000, 1.000000000000000000, 1.000000000000000000, 1.000000000000000000, 1.000000000000000000, 1.000000000000000000, 1.000000000000000000, 1.000000000000000000, 1.000000000000000000, 1.000000000000000000, 1.000000000000000000, 1.000000000000000000, 1.000000000000000000),
 ( 0.5895302151065233698, 0.5895302151065233698, 0.5895302151065233698, 0.5895302151065233698, 0.5895302151065233698, 0.5895302151065233698, 0.5895302151065233698, 0.5895302151065233698, 0.5895302151065233698, 0.5895302151065233698, 0.5895302151065233698, 0.5895302151065233698, 0.5895302151065233698, 0.5895302151065233698, 0.5895302151065233698, 0.5895302151065233698),
 ( 0.5895302151065233698, 0.5895302151065233698, 0.5895302151065233698, 0.5895302151065233698, 0.5895302151065233698, 0.5895302151065233698, 0.5895302151065233698, 0.5895302151065233698, 0.5895302151065233698, 0.5895302151065233698, 0.5895302151065233698, 0.5895302151065233698, 0.5895302151065233698, 0.5895302151065233698, 0.5895302151065233698, 0.5895302151065233698),
 ( 1.000000000000000000, 1.000000000000000000, 1.000000000000000000, 1.000000000000000000, 1.000000000000000000, 1.000000000000000000, 1.000000000000000000, 1.000000000000000000, 1.000000000000000000, 1.000000000000000000, 1.000000000000000000, 1.000000000000000000, 1.000000000000000000, 1.000000000000000000, 1.000000000000000000, 1.000000000000000000) ) ) 
 REPRESENTATION_ITEM ( '' )  SURFACE ( )  );
#3176 = EDGE_CURVE ( 'NONE', #11755, #3662, #20113, .T. ) ;
#3177 = CARTESIAN_POINT ( 'NONE',  ( 26.39808386558502917, 18.58254979424145503, -0.4463807625373593657 ) ) ;
#3178 = CARTESIAN_POINT ( 'NONE',  ( 23.61221640758335738, -8.051464822112826880, 0.4367666033528453395 ) ) ;
#3179 = ORIENTED_EDGE ( 'NONE', *, *, #4664, .T. ) ;
#3180 = ADVANCED_FACE ( 'NONE', ( #23103 ), #30446, .T. ) ;
#3181 = CARTESIAN_POINT ( 'NONE',  ( -57.12917293608614955, -2.964366234459024696, 5.871858320049880398 ) ) ;
#3182 = ADVANCED_FACE ( 'NONE', ( #10549 ), #20303, .T. ) ;
#3183 = ORIENTED_EDGE ( 'NONE', *, *, #17906, .F. ) ;
#3184 = DATE_AND_TIME ( #15870, #2886 ) ;
#3185 = CARTESIAN_POINT ( 'NONE',  ( 0.000000000000000000, 4.137773741518377513, 5.705158055754806945 ) ) ;
#3186 = VERTEX_POINT ( 'NONE', #28763 ) ;
#3187 = DIRECTION ( 'NONE',  ( 1.000000000000000000, 0.000000000000000000, 0.000000000000000000 ) ) ;
#3188 = CIRCLE ( 'NONE', #19208, 2.999999999999999556 ) ;
#3189 = ORIENTED_EDGE ( 'NONE', *, *, #12286, .F. ) ;
#3190 = CARTESIAN_POINT ( 'NONE',  ( 0.7632845268398876781, -8.734705317681624948, 0.4999240074894106822 ) ) ;
#3192 = ORIENTED_EDGE ( 'NONE', *, *, #25250, .F. ) ;
#3191 = CARTESIAN_POINT ( 'NONE',  ( 69.01696383923302847, -5.045148589264282890, -4.093304263523003250 ) ) ;
#3193 = ORIENTED_EDGE ( 'NONE', *, *, #2545, .F. ) ;
#3194 = CARTESIAN_POINT ( 'NONE',  ( 0.1517578099452217555, -1.375880305419572514, -4.522129901861164925 ) ) ;
#3195 = CARTESIAN_POINT ( 'NONE',  ( -3.862550801365593145, 3.521866450007987037, 0.3701630799359328372 ) ) ;
#3196 = CARTESIAN_POINT ( 'NONE',  ( 25.92249999999999943, 2.378061970571979433, -1.291182301015470824 ) ) ;
#3197 = CARTESIAN_POINT ( 'NONE',  ( 29.19831543700436427, -9.049787287704358363, -1.915219082070897638 ) ) ;
#3198 = CIRCLE ( 'NONE', #22998, 6.000000000000000888 ) ;
#3200 = VERTEX_POINT ( 'NONE', #20922 ) ;
#3199 = CARTESIAN_POINT ( 'NONE',  ( 5.377543748152550762, 7.530955069117551304, -2.741043480754851380 ) ) ;
#3201 = LINE ( 'NONE', #2705, #2289 ) ;
#3202 = CARTESIAN_POINT ( 'NONE',  ( 19.03564543755645033, 14.58476759517576404, 1.050000000000000044 ) ) ;
#3203 = CARTESIAN_POINT ( 'NONE',  ( 10.32244514579517691, -19.71146457077206193, 1.499999999999365841 ) ) ;
#3204 = DIRECTION ( 'NONE',  ( 0.1027947991993881510, -0.9947025833170222153, -3.252606517456439149E-15 ) ) ;
#3205 = CARTESIAN_POINT ( 'NONE',  ( 3.744708216408842549, 0.000000000000000000, 1.000000000000000000 ) ) ;
#3207 = EDGE_LOOP ( 'NONE', ( #17401, #1431, #1390, #30988 ) ) ;
#3206 = CARTESIAN_POINT ( 'NONE',  ( 25.75999999999999801, 0.8512451026088739825, 2.902758476911987628 ) ) ;
#3208 = PLANE ( 'NONE',  #20521 ) ;
#3209 = EDGE_CURVE ( 'NONE', #21075, #12143, #28617, .T. ) ;
#3210 = CARTESIAN_POINT ( 'NONE',  ( -24.45920507959942469, 18.39788475725609374, 1.774545360836604191 ) ) ;
#3211 = CARTESIAN_POINT ( 'NONE',  ( 21.79750000136559507, 0.3178988483021036315, 3.024605502323848949 ) ) ;
#3212 = CARTESIAN_POINT ( 'NONE',  ( 10.57125986779756843, -4.884328206559843899, 1.115095498423292142 ) ) ;
#3213 = AXIS2_PLACEMENT_3D ( 'NONE', #20669, #7943, #430 ) ;
#3214 = CARTESIAN_POINT ( 'NONE',  ( 15.55254023221931448, 20.42149909151575216, 5.412820279296878923 ) ) ;
#3215 = CARTESIAN_POINT ( 'NONE',  ( 15.28872660057389155, 20.76088595412472415, 4.629213727441584325 ) ) ;
#3216 = ADVANCED_FACE ( 'NONE', ( #18427 ), #18572, .F. ) ;
#3217 = DIRECTION ( 'NONE',  ( 0.000000000000000000, 1.000000000000000000, 0.000000000000000000 ) ) ;
#3218 = AXIS2_PLACEMENT_3D ( 'NONE', #31470, #1040, #28643 ) ;
#3219 = ORIENTED_EDGE ( 'NONE', *, *, #25311, .F. ) ;
#3220 = CIRCLE ( 'NONE', #9055, 5.009999999999999787 ) ;
#3221 = CARTESIAN_POINT ( 'NONE',  ( -10.00000000000000000, 0.000000000000000000, 0.000000000000000000 ) ) ;
#3222 = CARTESIAN_POINT ( 'NONE',  ( -2.994413461838833612, -0.08301688964435380291, -1.285747183615637113 ) ) ;
#3223 = EDGE_CURVE ( 'NONE', #22549, #12204, #18529, .T. ) ;
#3224 = CARTESIAN_POINT ( 'NONE',  ( 6.880159790065804692, 8.451885315426457268, -2.190520500543400306 ) ) ;
#3226 = CARTESIAN_POINT ( 'NONE',  ( 108.0017901292596747, -18.09513953262979058, 4.637902566605376364 ) ) ;
#3225 = LINE ( 'NONE', #10913, #22517 ) ;
#3227 = ORIENTED_EDGE ( 'NONE', *, *, #7500, .T. ) ;
#3228 = CARTESIAN_POINT ( 'NONE',  ( -4.750050800000000351, -3.113457007523259268, 0.9222479816126455399 ) ) ;
#3229 = EDGE_LOOP ( 'NONE', ( #24727, #26646, #9576, #31466, #15506 ) ) ;
#3230 = DIRECTION ( 'NONE',  ( 0.000000000000000000, 0.000000000000000000, 1.000000000000000000 ) ) ;
#3232 = VERTEX_POINT ( 'NONE', #5854 ) ;
#3231 = CARTESIAN_POINT ( 'NONE',  ( 10.00000000000000178, -8.574039729943018837E-16, 0.000000000000000000 ) ) ;
#3233 = ADVANCED_FACE ( 'NONE', ( #2710 ), #23580, .T. ) ;
#3234 = VERTEX_POINT ( 'NONE', #8228 ) ;
#3235 = CARTESIAN_POINT ( 'NONE',  ( 56.97280603064898941, -277.2763395528616002, -5.471072653611049219 ) ) ;
#3236 = AXIS2_PLACEMENT_3D ( 'NONE', #27896, #12821, #5013 ) ;
#3237 = AXIS2_PLACEMENT_3D ( 'NONE', #21058, #31260, #18530 ) ;
#3238 = CARTESIAN_POINT ( 'NONE',  ( 5.175170698068133568, 0.5000000000000000000, 5.403836275575642389 ) ) ;
#3240 = ORIENTED_EDGE ( 'NONE', *, *, #4835, .T. ) ;
#3239 = CARTESIAN_POINT ( 'NONE',  ( 107.9166483397147687, 17.71402499141862208, 3.339827141515659292 ) ) ;
#3241 = ORIENTED_EDGE ( 'NONE', *, *, #27316, .F. ) ;
#3242 = AXIS2_PLACEMENT_3D ( 'NONE', #8034, #16031, #28757 ) ;
#3243 = CARTESIAN_POINT ( 'NONE',  ( -3.262261974584276913, -10.74317314725658434, -1.743566385593488199 ) ) ;
#3244 = B_SPLINE_CURVE_WITH_KNOTS ( 'NONE', 3,
 ( #29955, #7044, #4386, #12071, #14571, #17255, #1896, #14227 ),
 .UNSPECIFIED., .F., .F.,
 ( 4, 2, 2, 4 ),
 ( 2.304311362623472242E-07, 0.001064743401393353391, 0.001596999886521901450, 0.002129256371650449509 ),
 .UNSPECIFIED. ) ;
#3245 = DIRECTION ( 'NONE',  ( 1.000000000000000000, -0.000000000000000000, -0.000000000000000000 ) ) ;
#3246 = CARTESIAN_POINT ( 'NONE',  ( 10.00000000000000178, 3.407865132560231380, -3.672404558090005100 ) ) ;
#3247 = DIRECTION ( 'NONE',  ( 0.000000000000000000, 0.000000000000000000, 1.000000000000000000 ) ) ;
#3248 = CARTESIAN_POINT ( 'NONE',  ( 3.020080181661098706, 3.262125172874016155, 8.342499971033864981 ) ) ;
#3249 = AXIS2_PLACEMENT_3D ( 'NONE', #3134, #609, #15662 ) ;
#3250 = ADVANCED_FACE ( 'NONE', ( #7884 ), #12885, .T. ) ;
#3251 = CARTESIAN_POINT ( 'NONE',  ( -6.557304906975410574, 1.062355717592095683, 2.999999999999999112 ) ) ;
#3252 = FACE_OUTER_BOUND ( 'NONE', #14155, .T. ) ;
#3253 = CARTESIAN_POINT ( 'NONE',  ( 5.489343958331425632, 7.664144799260948382, 2.678936089601470005 ) ) ;
#3254 = CARTESIAN_POINT ( 'NONE',  ( 2.949938889207334825, 0.4708014538555421735, 1.389575531037028799 ) ) ;
#3255 = ORIENTED_EDGE ( 'NONE', *, *, #6907, .F. ) ;
#3256 = LINE ( 'NONE', #18616, #4436 ) ;
#3257 = EDGE_CURVE ( 'NONE', #18014, #22155, #21100, .T. ) ;
#3258 = CIRCLE ( 'NONE', #18727, 10.99999999999999822 ) ;
#3259 = DIRECTION ( 'NONE',  ( 0.000000000000000000, 0.2588190451025241812, -0.9659258262890673130 ) ) ;
#3260 = EDGE_CURVE ( 'NONE', #13354, #24212, #17632, .T. ) ;
#3261 = DIRECTION ( 'NONE',  ( 0.000000000000000000, -0.9659258262890710878, 0.2588190451025100258 ) ) ;
#3262 = VERTEX_POINT ( 'NONE', #2909 ) ;
#3263 = CARTESIAN_POINT ( 'NONE',  ( 24.54750000136559507, 1.913930629741522838, -2.363507492473150062 ) ) ;
#3264 = AXIS2_PLACEMENT_3D ( 'NONE', #2109, #9800, #9298 ) ;
#3265 = CIRCLE ( 'NONE', #5913, 4.000000000000001776 ) ;
#3266 = CARTESIAN_POINT ( 'NONE',  ( 20.05745782660422094, -21.55152848446452296, -1.510982242221070804 ) ) ;
#3267 = EDGE_LOOP ( 'NONE', ( #8390, #29992, #6022, #11558 ) ) ;
#3268 = CARTESIAN_POINT ( 'NONE',  ( 1.135243775848452819, -9.027721268913223795, -1.499999999999999112 ) ) ;
#3269 = EDGE_CURVE ( 'NONE', #3747, #19054, #16038, .T. ) ;
#3270 = AXIS2_PLACEMENT_3D ( 'NONE', #9376, #27938, #4551 ) ;
#3271 = ORIENTED_EDGE ( 'NONE', *, *, #25920, .F. ) ;
#3272 = CARTESIAN_POINT ( 'NONE',  ( 29.40513214805973874, -2.959508727827649732, -1.915219082070890755 ) ) ;
#3273 = PERSON_AND_ORGANIZATION ( #18331, #32302 ) ;
#3275 = VERTEX_POINT ( 'NONE', #23272 ) ;
#3274 = LINE ( 'NONE', #18630, #19740 ) ;
#3276 = ORIENTED_EDGE ( 'NONE', *, *, #31346, .F. ) ;
#3277 = CARTESIAN_POINT ( 'NONE',  ( 24.42250000136559507, 1.913930629741522838, -2.363507492473150062 ) ) ;
#3278 = EDGE_CURVE ( 'NONE', #29313, #7400, #16923, .T. ) ;
#3279 = ORIENTED_EDGE ( 'NONE', *, *, #26530, .F. ) ;
#3280 = DIRECTION ( 'NONE',  ( -0.1327696077594705815, 0.9911469271785068313, 0.000000000000000000 ) ) ;
#3282 = ORIENTED_EDGE ( 'NONE', *, *, #10989, .F. ) ;
#3281 = CARTESIAN_POINT ( 'NONE',  ( 68.92628806523653395, -3.240579989648024295, -0.4367667217259110779 ) ) ;
#3283 = CARTESIAN_POINT ( 'NONE',  ( 14.90130905634548952, 9.429294031743246762, 1.050000000000000044 ) ) ;
#3284 = CARTESIAN_POINT ( 'NONE',  ( 7.064632816082965228, -0.7071067811865714425, 8.721381771256201176 ) ) ;
#3285 = VECTOR ( 'NONE', #13356, 1000.000000000000114 ) ;
#3286 = CARTESIAN_POINT ( 'NONE',  ( 25.75999999999999801, -2.208672634433321348E-15, 0.000000000000000000 ) ) ;
#3287 = LINE ( 'NONE', #2627, #15095 ) ;
#3288 = VECTOR ( 'NONE', #5424, 1000.000000000000000 ) ;
#3289 = AXIS2_PLACEMENT_3D ( 'NONE', #15519, #25239, #2358 ) ;
#3290 = ORIENTED_EDGE ( 'NONE', *, *, #17803, .T. ) ;
#3291 = CIRCLE ( 'NONE', #22510, 5.500000000000001776 ) ;
#3292 = DIRECTION ( 'NONE',  ( 0.000000000000000000, 0.5735764363510439390, 0.8191520442889933529 ) ) ;
#3293 = CARTESIAN_POINT ( 'NONE',  ( -2.617344628312510135, 0.000000000000000000, -1.468739241856748867 ) ) ;
#3294 = CARTESIAN_POINT ( 'NONE',  ( 18.65791233782715963, -7.001076235476726417, -2.184956778830003277 ) ) ;
#3295 = CARTESIAN_POINT ( 'NONE',  ( -6.700050802731188249, 2.853674364686379583, 1.549418761218565921 ) ) ;
#3296 = ADVANCED_FACE ( 'NONE', ( #23415 ), #22923, .F. ) ;
#3297 = VECTOR ( 'NONE', #16441, 1000.000000000000000 ) ;
#3298 = DIRECTION ( 'NONE',  ( 1.000000000000000000, 0.000000000000000000, -0.000000000000000000 ) ) ;
#3299 = CARTESIAN_POINT ( 'NONE',  ( 23.19969958429632229, -21.93395823966979563, 1.123858831411095105 ) ) ;
#3300 = CARTESIAN_POINT ( 'NONE',  ( -2.512942406915326110, -5.022711880624455567E-15, 2.999999999999999556 ) ) ;
#3301 = FACE_OUTER_BOUND ( 'NONE', #9678, .T. ) ;
#3302 = EDGE_CURVE ( 'NONE', #8298, #27019, #32598, .T. ) ;
#3303 = LINE ( 'NONE', #189, #30538 ) ;
#3304 = CARTESIAN_POINT ( 'NONE',  ( -2.462550801365593678, 0.3701630799359330593, -3.521866450007987037 ) ) ;
#3305 = EDGE_LOOP ( 'NONE', ( #5391, #25984, #31749 ) ) ;
#3306 = CARTESIAN_POINT ( 'NONE',  ( -2.654531657079157281, 2.846291840500173365, 1.545410377633946952 ) ) ;
#3307 = VECTOR ( 'NONE', #1874, 1000.000000000000000 ) ;
#3308 = CARTESIAN_POINT ( 'NONE',  ( 108.1156589233281267, 18.82219444680281484, 4.414476567109669958 ) ) ;
#3309 = DIRECTION ( 'NONE',  ( 0.000000000000000000, 0.000000000000000000, 1.000000000000000000 ) ) ;
#3310 = CARTESIAN_POINT ( 'NONE',  ( 24.24156412054449206, -17.70199322286843113, 1.500000000000000000 ) ) ;
#3311 = VERTEX_POINT ( 'NONE', #29373 ) ;
#3312 = CARTESIAN_POINT ( 'NONE',  ( 20.50111451137534857, -3.256483526998273983E-15, 2.499999999999998668 ) ) ;
#3313 = VECTOR ( 'NONE', #7778, 999.9999999999998863 ) ;
#3314 = EDGE_CURVE ( 'NONE', #9752, #6678, #9631, .T. ) ;
#3315 = AXIS2_PLACEMENT_3D ( 'NONE', #19026, #16177, #21055 ) ;
#3316 = ORIENTED_EDGE ( 'NONE', *, *, #8723, .F. ) ;
#3317 = CARTESIAN_POINT ( 'NONE',  ( 2.274274201625327230, -1.464956435139465496, -10.90201369670500142 ) ) ;
#3318 = CALENDAR_DATE ( 2026, 6, 10 ) ;
#3319 = CARTESIAN_POINT ( 'NONE',  ( 54.94687251578933740, -5.409905656046521294, 4.074610066671965569 ) ) ;
#3320 = AXIS2_PLACEMENT_3D ( 'NONE', #2044, #30151, #7046 ) ;
#3321 = AXIS2_PLACEMENT_3D ( 'NONE', #32670, #14601, #1743 ) ;
#3322 = EDGE_CURVE ( 'NONE', #13354, #25477, #1819, .T. ) ;
#3323 = AXIS2_PLACEMENT_3D ( 'NONE', #6371, #7485, #12522 ) ;
#3324 = APPROVAL ( #2688, 'UNSPECIFIED' ) ;
#3325 = CARTESIAN_POINT ( 'NONE',  ( 8.917260909444884476, 0.3029815364085644558, 1.471149382586864895 ) ) ;
#3326 = PLANE ( 'NONE',  #7047 ) ;
#3327 = ORIENTED_EDGE ( 'NONE', *, *, #3278, .F. ) ;
#3328 = CARTESIAN_POINT ( 'NONE',  ( 0.1574692421720930435, 7.165523657698311233, 7.841623826006798303 ) ) ;
#3329 = FACE_OUTER_BOUND ( 'NONE', #23209, .T. ) ;
#3330 = CARTESIAN_POINT ( 'NONE',  ( 109.3993806922052698, 20.31298924473501444, 2.334455007174201402 ) ) ;
#3332 = ORIENTED_EDGE ( 'NONE', *, *, #25584, .T. ) ;
#3331 = CARTESIAN_POINT ( 'NONE',  ( 0.000000000000000000, 0.000000000000000000, -3.000000000000000444 ) ) ;
#3333 = VECTOR ( 'NONE', #17046, 1000.000000000000000 ) ;
#3334 = DIRECTION ( 'NONE',  ( 0.000000000000000000, 0.000000000000000000, 1.000000000000000000 ) ) ;
#3335 = AXIS2_PLACEMENT_3D ( 'NONE', #1445, #32027, #9098 ) ;
#3336 = CARTESIAN_POINT ( 'NONE',  ( 108.1288400433390393, -19.92462668933126579, -1.384270303710054328 ) ) ;
#3337 = DIRECTION ( 'NONE',  ( 0.4030398059120877119, 0.9151824489413827868, -3.863824945872021474E-15 ) ) ;
#3338 = AXIS2_PLACEMENT_3D ( 'NONE', #8701, #18240, #29108 ) ;
#3339 = ORIENTED_EDGE ( 'NONE', *, *, #9034, .T. ) ;
#3340 = ORIENTED_EDGE ( 'NONE', *, *, #13637, .T. ) ;
#3341 = ADVANCED_FACE ( 'NONE', ( #27039 ), #24136, .T. ) ;
#3342 = AXIS2_PLACEMENT_3D ( 'NONE', #19941, #27610, #9715 ) ;
#3344 = VECTOR ( 'NONE', #13030, 1000.000000000000114 ) ;
#3343 = DIRECTION ( 'NONE',  ( 0.000000000000000000, 0.000000000000000000, 1.000000000000000000 ) ) ;
#3345 = LINE ( 'NONE', #23543, #29036 ) ;
#3346 = CARTESIAN_POINT ( 'NONE',  ( -1.293118168543983204, -1.473601950426632889, 5.485967528433935314 ) ) ;
#3347 = ORIENTED_EDGE ( 'NONE', *, *, #27986, .F. ) ;
#3348 = EDGE_CURVE ( 'NONE', #5364, #12775, #22030, .T. ) ;
#3349 = AXIS2_PLACEMENT_3D ( 'NONE', #6670, #14008, #1995 ) ;
#3350 = CARTESIAN_POINT ( 'NONE',  ( -32.99878091140236336, 0.000000000000000000, 1.268467860057148622 ) ) ;
#3351 = VECTOR ( 'NONE', #25468, 1000.000000000000227 ) ;
#3352 = CARTESIAN_POINT ( 'NONE',  ( 2.357329994281668117, 2.053141773251463853, 10.64078702437730151 ) ) ;
#3353 = CARTESIAN_POINT ( 'NONE',  ( -59.04079763661544433, -4.690551911666260843, 5.310642798857019287 ) ) ;
#3354 = CARTESIAN_POINT ( 'NONE',  ( -4.087550801365593678, 2.752080473201636845, -2.228590825266444142 ) ) ;
#3355 = CARTESIAN_POINT ( 'NONE',  ( -47.25352234179201361, 16.22999999999998266, -1.050000000000000044 ) ) ;
#3356 = LINE ( 'NONE', #30791, #1260 ) ;
#3357 = VERTEX_POINT ( 'NONE', #9314 ) ;
#3358 = CARTESIAN_POINT ( 'NONE',  ( 18.96091535642496240, -3.614110606601101949, 2.184956778829998836 ) ) ;
#3359 = AXIS2_PLACEMENT_3D ( 'NONE', #12499, #1982, #22707 ) ;
#3360 = ORIENTED_EDGE ( 'NONE', *, *, #31151, .F. ) ;
#3362 = CIRCLE ( 'NONE', #6564, 2.999999999999999556 ) ;
#3361 = CALENDAR_DATE ( 2026, 6, 10 ) ;
#3363 = DIRECTION ( 'NONE',  ( 0.06927878976713817971, -0.9975973382524637723, 0.000000000000000000 ) ) ;
#3364 = CIRCLE ( 'NONE', #2281, 0.5000000000000004441 ) ;
#3365 = AXIS2_PLACEMENT_3D ( 'NONE', #29577, #11512, #18694 ) ;
#3366 = VECTOR ( 'NONE', #30673, 1000.000000000000000 ) ;
#3367 = CARTESIAN_POINT ( 'NONE',  ( 12.02900455932878820, -13.20152970908862500, -1.000000000000000000 ) ) ;
#3368 = VERTEX_POINT ( 'NONE', #32408 ) ;
#3369 = CARTESIAN_POINT ( 'NONE',  ( 10.52034268205830259, 3.055657119358849094, -3.641590349731898879 ) ) ;
#3370 = ORIENTED_EDGE ( 'NONE', *, *, #5111, .F. ) ;
#3371 = ORIENTED_EDGE ( 'NONE', *, *, #15819, .F. ) ;
#3372 = CARTESIAN_POINT ( 'NONE',  ( -23.54713438637982748, 8.275374457817616047, 8.599999999999999645 ) ) ;
#3373 = CARTESIAN_POINT ( 'NONE',  ( -4.862550801365594033, 0.3701630799359330593, -3.521866450007987037 ) ) ;
#3374 = CARTESIAN_POINT ( 'NONE',  ( 7.868768533615232208, -10.68327055928662617, 1.500000000000000000 ) ) ;
#3375 = VECTOR ( 'NONE', #24383, 999.9999999999998863 ) ;
#3376 = CARTESIAN_POINT ( 'NONE',  ( 1.743661372318740632, -1.493834480585329194, -1.500000000000000222 ) ) ;
#3378 = ORIENTED_EDGE ( 'NONE', *, *, #12056, .F. ) ;
#3377 = CARTESIAN_POINT ( 'NONE',  ( 16.02030197382709176, 11.87192001622980264, -1.500000000000000222 ) ) ;
#3379 = CARTESIAN_POINT ( 'NONE',  ( -7.387550801365593500, 0.3701630799359330593, -3.521866450007987037 ) ) ;
#3380 = CARTESIAN_POINT ( 'NONE',  ( 13.48007872897105841, 7.959851041527245208, 1.500000000000000000 ) ) ;
#3381 = DIRECTION ( 'NONE',  ( -4.339452166954056922E-15, 0.000000000000000000, -1.000000000000000000 ) ) ;
#3382 = CARTESIAN_POINT ( 'NONE',  ( 20.86000000136559507, -0.9349337715887248157, 3.156283516753367824 ) ) ;
#3383 = EDGE_CURVE ( 'NONE', #11370, #11079, #9469, .T. ) ;
#3385 = ORIENTED_EDGE ( 'NONE', *, *, #25958, .T. ) ;
#3384 = CARTESIAN_POINT ( 'NONE',  ( -3.529825581556913254E-16, -4.116875700062066379, -2.376879293651108060 ) ) ;
#3386 = ADVANCED_FACE ( 'NONE', ( #29566 ), #18168, .F. ) ;
#3387 = CIRCLE ( 'NONE', #7113, 0.4499999999999990119 ) ;
#3388 = CIRCLE ( 'NONE', #12984, 0.4500000000000025646 ) ;
#3389 = DIRECTION ( 'NONE',  ( 0.000000000000000000, -0.7071067811865380248, -0.7071067811865570096 ) ) ;
#3390 = CARTESIAN_POINT ( 'NONE',  ( 21.36000000273118715, 1.942864903642424146, 1.573300977624592534 ) ) ;
#3391 = AXIS2_PLACEMENT_3D ( 'NONE', #8493, #28893, #8667 ) ;
#3392 = AXIS2_PLACEMENT_3D ( 'NONE', #12466, #32881, #9949 ) ;
#3393 = CARTESIAN_POINT ( 'NONE',  ( -17.31779044994511807, 7.339147416616279784, 1.500000000000000000 ) ) ;
#3394 = DIRECTION ( 'NONE',  ( 0.000000000000000000, 0.000000000000000000, -1.000000000000000000 ) ) ;
#3395 = CARTESIAN_POINT ( 'NONE',  ( -3.018833153846783635, -0.05660549560294792643, -1.240144350321688238 ) ) ;
#3396 = PLANE ( 'NONE',  #6018 ) ;
#3397 = AXIS2_PLACEMENT_3D ( 'NONE', #32560, #24358, #27038 ) ;
#3398 = LOCAL_TIME ( 16, 7, 10.00000000000000000, #17370 ) ;
#3399 = CARTESIAN_POINT ( 'NONE',  ( 9.300899703876350344, 0.2440751071713773424, 1.049978936837301369 ) ) ;
#3400 = VERTEX_POINT ( 'NONE', #16669 ) ;
#3401 = CARTESIAN_POINT ( 'NONE',  ( 18.00753636102977850, -21.49658694929768998, 1.499999999999999112 ) ) ;
#3402 = CARTESIAN_POINT ( 'NONE',  ( -3.086632255569896177, -0.4418731834524158852, -1.500000000000000444 ) ) ;
#3403 = CARTESIAN_POINT ( 'NONE',  ( 5.489343806296449024, 7.976812024616046770, -1.512045527216122176 ) ) ;
#3405 = CARTESIAN_POINT ( 'NONE',  ( 107.4526705878834179, -17.39807245566085570, 4.614338180291445823 ) ) ;
#3404 = CARTESIAN_POINT ( 'NONE',  ( 108.1156589233279135, 18.82219444680288234, -4.397958565568440115 ) ) ;
#3406 = VERTEX_POINT ( 'NONE', #26882 ) ;
#3407 = AXIS2_PLACEMENT_3D ( 'NONE', #10087, #22473, #14428 ) ;
#3408 = CARTESIAN_POINT ( 'NONE',  ( -4.906376978575949011, -0.1572233378491262878, 2.999999999999999556 ) ) ;
#3409 = ORIENTED_EDGE ( 'NONE', *, *, #6084, .F. ) ;
#3410 = CARTESIAN_POINT ( 'NONE',  ( -32.42885140446504977, -0.0003384977252881313063, 1.500000000000000000 ) ) ;
#3411 = CIRCLE ( 'NONE', #13434, 6.000000000000000888 ) ;
#3413 = VERTEX_POINT ( 'NONE', #9132 ) ;
#3412 = CARTESIAN_POINT ( 'NONE',  ( 108.0946594595236689, 20.79497418261435016, -1.491968323836175836 ) ) ;
#3414 = EDGE_LOOP ( 'NONE', ( #27993, #12919, #18919, #26401 ) ) ;
#3415 = CARTESIAN_POINT ( 'NONE',  ( 18.58227844715246135, -7.846511338401735536, -2.713652344655543391 ) ) ;
#3416 = CIRCLE ( 'NONE', #1286, 8.749000000000002331 ) ;
#3417 = VECTOR ( 'NONE', #31959, 1000.000000000000000 ) ;
#3418 = CIRCLE ( 'NONE', #23596, 0.5000000000000004441 ) ;
#3419 = CARTESIAN_POINT ( 'NONE',  ( -6.050050802731187893, 2.331437884370912705, -1.887961173149511618 ) ) ;
#3420 = EDGE_CURVE ( 'NONE', #14502, #6959, #18993, .T. ) ;
#3422 = EDGE_LOOP ( 'NONE', ( #1336, #9888, #30047, #31410, #29574, #25023 ) ) ;
#3421 = LINE ( 'NONE', #900, #10714 ) ;
#3423 = CARTESIAN_POINT ( 'NONE',  ( 9.924500721901809541, 1.154815372706009535, -1.050000000000000044 ) ) ;
#3424 = CARTESIAN_POINT ( 'NONE',  ( -4.148668979644773103, -6.185511544332382705, -1.745226750906151425 ) ) ;
#3425 = DIRECTION ( 'NONE',  ( -1.000000000000000000, 0.000000000000000000, 0.000000000000000000 ) ) ;
#3426 = LOCAL_TIME ( 16, 7, 10.00000000000000000, #24532 ) ;
#3427 = CARTESIAN_POINT ( 'NONE',  ( 20.69346795568988995, -16.15118080712828430, -1.000000000000000444 ) ) ;
#3428 = CARTESIAN_POINT ( 'NONE',  ( 107.4498027076793960, -17.35649700946218132, -4.512031564368074399 ) ) ;
#3429 = CARTESIAN_POINT ( 'NONE',  ( 6.880159540721329847, 3.624895993596869648, 7.943102264535267132 ) ) ;
#3430 = CARTESIAN_POINT ( 'NONE',  ( 107.5617944031221640, -18.98359742639815551, -4.522129901861166701 ) ) ;
#3431 = CARTESIAN_POINT ( 'NONE',  ( 107.6235316907398243, 18.91057310341846787, -4.397958565568440115 ) ) ;
#3432 = DIRECTION ( 'NONE',  ( -1.000000000000000000, 0.000000000000000000, 0.000000000000000000 ) ) ;
#3433 = DIRECTION ( 'NONE',  ( 0.000000000000000000, 0.000000000000000000, 1.000000000000000000 ) ) ;
#3434 = CARTESIAN_POINT ( 'NONE',  ( 2.363212477606361439, -0.1552069907123549142, 1.757289734063312014 ) ) ;
#3435 = ORIENTED_EDGE ( 'NONE', *, *, #30694, .T. ) ;
#3436 = CARTESIAN_POINT ( 'NONE',  ( 29.27523314209291527, -3.695744416153337042, 0.07017451552713392660 ) ) ;
#3437 = EDGE_CURVE ( 'NONE', #17869, #26510, #14664, .T. ) ;
#3438 = VECTOR ( 'NONE', #20465, 1000.000000000000000 ) ;
#3439 = CARTESIAN_POINT ( 'NONE',  ( 107.3476768466458253, -15.88628154573095586, -1.500000000000000000 ) ) ;
#3440 = DIRECTION ( 'NONE',  ( 1.000000000000000000, -0.000000000000000000, -0.000000000000000000 ) ) ;
#3441 = VERTEX_POINT ( 'NONE', #16842 ) ;
#3442 = CARTESIAN_POINT ( 'NONE',  ( 23.73500000136559152, 3.156283516753366047, 0.9349337715887203748 ) ) ;
#3443 = B_SPLINE_CURVE_WITH_KNOTS ( 'NONE', 3,
 ( #20128, #24175, #31880, #26852, #1451, #19155 ),
 .UNSPECIFIED., .F., .F.,
 ( 4, 2, 4 ),
 ( 0.009536920346932386411, 0.5047684601734662158, 1.000000000000000000 ),
 .UNSPECIFIED. ) ;
#3444 = DIRECTION ( 'NONE',  ( 0.000000000000000000, 1.000000000000000000, 0.000000000000000000 ) ) ;
#3445 = ADVANCED_FACE ( 'NONE', ( #24861 ), #10688, .T. ) ;
#3446 = CARTESIAN_POINT ( 'NONE',  ( 110.2274383572228942, 17.36892446252421962, -4.612695725900422872 ) ) ;
#3447 = PRODUCT_DEFINITION_FORMATION_WITH_SPECIFIED_SOURCE ( 'ANY', '', #32741, .NOT_KNOWN. ) ;
#3448 = ORIENTED_EDGE ( 'NONE', *, *, #11508, .T. ) ;
#3449 = CARTESIAN_POINT ( 'NONE',  ( 0.5441516179539818143, -6.195371308637259489, -1.500000000000000000 ) ) ;
#3450 = ORIENTED_EDGE ( 'NONE', *, *, #130, .T. ) ;
#3451 = ORIENTED_EDGE ( 'NONE', *, *, #11320, .F. ) ;
#3452 = DIRECTION ( 'NONE',  ( -1.000000000000000000, 8.574039729943017111E-17, -0.000000000000000000 ) ) ;
#3453 = ADVANCED_FACE ( 'NONE', ( #6804 ), #22349, .F. ) ;
#3454 = CALENDAR_DATE ( 2026, 6, 10 ) ;
#3456 = ORIENTED_EDGE ( 'NONE', *, *, #30110, .T. ) ;
#3455 = CARTESIAN_POINT ( 'NONE',  ( 23.23500000000000298, 0.2613211581691317065, 2.486304738420681559 ) ) ;
#3457 = EDGE_LOOP ( 'NONE', ( #30596, #21004, #18198, #23573, #22052 ) ) ;
#3458 = CARTESIAN_POINT ( 'NONE',  ( 26.39808386558502562, 18.58254979424150832, 0.4463807625373201193 ) ) ;
#3459 = ORIENTED_EDGE ( 'NONE', *, *, #10593, .T. ) ;
#3460 = SHAPE_REPRESENTATION ( 'Part6_handleknob', ( #2865 ), #7102 ) ;
#3461 = PLANE ( 'NONE',  #15528 ) ;
#3463 = VERTEX_POINT ( 'NONE', #30066 ) ;
#3462 = CARTESIAN_POINT ( 'NONE',  ( 10.00000000000000000, -4.116875700062067267, -2.376879293651108060 ) ) ;
#3464 = FACE_OUTER_BOUND ( 'NONE', #961, .T. ) ;
#3465 = CARTESIAN_POINT ( 'NONE',  ( 3.249999999999999556, 0.000000000000000000, 0.000000000000000000 ) ) ;
#3466 = EDGE_CURVE ( 'NONE', #7281, #2902, #29233, .T. ) ;
#3467 = DIRECTION ( 'NONE',  ( 0.9896144216807900573, 0.000000000000000000, 0.1437473352845041463 ) ) ;
#3468 = EDGE_CURVE ( 'NONE', #9954, #22307, #16021, .T. ) ;
#3469 = DIRECTION ( 'NONE',  ( -1.000000000000000000, 0.000000000000000000, 0.000000000000000000 ) ) ;
#3470 = CARTESIAN_POINT ( 'NONE',  ( 108.0617485914592208, -18.95852647251686562, 4.497382052644061545 ) ) ;
#3471 = CARTESIAN_POINT ( 'NONE',  ( -4.000050800000000351, -2.331437884370912705, 1.887961173149512062 ) ) ;
#3472 = LINE ( 'NONE', #23678, #8581 ) ;
#3473 = CARTESIAN_POINT ( 'NONE',  ( 23.62103335626769152, -7.897478826044957323, -1.169950778993630758 ) ) ;
#3474 = CARTESIAN_POINT ( 'NONE',  ( 1.750000000000000222, -5.522688772756442432, 6.461416928141223259 ) ) ;
#3475 = LOCAL_TIME ( 16, 7, 10.00000000000000000, #16291 ) ;
#3476 = EDGE_CURVE ( 'NONE', #4283, #18871, #4830, .T. ) ;
#3477 = CARTESIAN_POINT ( 'NONE',  ( 1.750000000000000222, -7.851777359433977921, -3.255701506262514311 ) ) ;
#3478 = DIRECTION ( 'NONE',  ( -0.08343273266574553759, -0.4645863764670123963, 0.8815886103626666692 ) ) ;
#3479 = DIRECTION ( 'NONE',  ( 0.000000000000000000, 0.000000000000000000, 1.000000000000000000 ) ) ;
#3480 = CARTESIAN_POINT ( 'NONE',  ( 10.00000000000000000, 2.285372942705016897, -4.458382051008168645 ) ) ;
#3481 = LINE ( 'NONE', #31874, #32687 ) ;
#3482 = CARTESIAN_POINT ( 'NONE',  ( -3.862550801365593145, 3.521866450007987037, 0.3701630799359328372 ) ) ;
#3483 = VERTEX_POINT ( 'NONE', #125 ) ;
#3484 = EDGE_CURVE ( 'NONE', #7787, #17721, #27690, .T. ) ;
#3485 = CARTESIAN_POINT ( 'NONE',  ( -5.500050800000000351, -2.983565686104819648, -0.3135853898029605791 ) ) ;
#3486 = TOROIDAL_SURFACE ( 'NONE', #30188, 7.482234843104714983, 0.5000000000000000000 ) ;
#3487 = CARTESIAN_POINT ( 'NONE',  ( 15.55254023221933046, 20.42149909151570597, -5.396302277755718357 ) ) ;
#3488 = CARTESIAN_POINT ( 'NONE',  ( 25.75999999999999801, -2.208672634433321348E-15, 0.000000000000000000 ) ) ;
#3489 = CARTESIAN_POINT ( 'NONE',  ( 8.396671913538202858, -0.7629006742129739171, 1.500000000000000000 ) ) ;
#3490 = EDGE_LOOP ( 'NONE', ( #467, #13667, #10919, #26507 ) ) ;
#3491 = CARTESIAN_POINT ( 'NONE',  ( 69.01291188535118692, -4.970031385437840399, -3.993434827419594324 ) ) ;
#3492 = ORIENTED_EDGE ( 'NONE', *, *, #26925, .F. ) ;
#3493 = CARTESIAN_POINT ( 'NONE',  ( 1.562973067601286070, -10.39368793503460431, 1.763952067544157343 ) ) ;
#3494 = DATE_AND_TIME ( #3318, #32278 ) ;
#3495 = CARTESIAN_POINT ( 'NONE',  ( 69.01321520912082974, -4.970018244546921871, 3.993434826753180289 ) ) ;
#3496 = EDGE_CURVE ( 'NONE', #1139, #23130, #4978, .T. ) ;
#3497 = EDGE_CURVE ( 'NONE', #13341, #7400, #12985, .T. ) ;
#3498 = CARTESIAN_POINT ( 'NONE',  ( 3.499999999999999556, 7.008469740302810891, 2.257469275785292329 ) ) ;
#3499 = CARTESIAN_POINT ( 'NONE',  ( 0.000000000000000000, -8.497168642645966941, 0.2193742428684632428 ) ) ;
#3500 = DIRECTION ( 'NONE',  ( -0.000000000000000000, -0.9993908270190956511, -0.03489949670250104552 ) ) ;
#3501 = EDGE_LOOP ( 'NONE', ( #27745, #25053, #22650, #10923, #25083, #32399 ) ) ;
#3502 = EDGE_CURVE ( 'NONE', #20265, #26968, #20184, .T. ) ;
#3503 = CARTESIAN_POINT ( 'NONE',  ( 0.3749740905863469531, 6.632019415960888509, 7.612528756000761732 ) ) ;
#3504 = EDGE_CURVE ( 'NONE', #7400, #6370, #15513, .T. ) ;
#3505 = CARTESIAN_POINT ( 'NONE',  ( 24.97738509828242925, 18.93945643846228677, -1.491740999229418829 ) ) ;
#3506 = DIRECTION ( 'NONE',  ( 1.000000000000000000, 0.000000000000000000, 0.000000000000000000 ) ) ;
#3508 = ORIENTED_EDGE ( 'NONE', *, *, #24722, .F. ) ;
#3507 = LINE ( 'NONE', #13662, #26692 ) ;
#3509 = CARTESIAN_POINT ( 'NONE',  ( -2.312550801365593767, 3.675193018007247403, -1.088641768524161391 ) ) ;
#3510 = CARTESIAN_POINT ( 'NONE',  ( 108.3190031596522260, 19.95449539046050447, 1.997040456489197036 ) ) ;
#3511 = CARTESIAN_POINT ( 'NONE',  ( 0.000000000000000000, 0.000000000000000000, 0.000000000000000000 ) ) ;
#3512 = ORIENTED_EDGE ( 'NONE', *, *, #14084, .F. ) ;
#3513 = ORIENTED_EDGE ( 'NONE', *, *, #32952, .F. ) ;
#3514 = CARTESIAN_POINT ( 'NONE',  ( 107.5617944031221640, -18.98359742639815551, 4.522129901861158707 ) ) ;
#3515 = DIRECTION ( 'NONE',  ( 0.000000000000000000, 0.000000000000000000, 1.000000000000000000 ) ) ;
#3516 = FACE_OUTER_BOUND ( 'NONE', #18801, .T. ) ;
#3517 = CARTESIAN_POINT ( 'NONE',  ( -0.9232102171129876744, 0.000000000000000000, 4.522129901861159595 ) ) ;
#3518 = CARTESIAN_POINT ( 'NONE',  ( 25.11445742118086599, -17.48309506032569516, 1.186364133453378322 ) ) ;
#3519 = EDGE_CURVE ( 'NONE', #18044, #23643, #28235, .T. ) ;
#3520 = LINE ( 'NONE', #3826, #10841 ) ;
#3521 = CC_DESIGN_DATE_AND_TIME_ASSIGNMENT ( #18027, #25543, ( #28213 ) ) ;
#3522 = CARTESIAN_POINT ( 'NONE',  ( -58.35079223774033608, -4.003636301679985188, 5.522895031407148103 ) ) ;
#3523 = CARTESIAN_POINT ( 'NONE',  ( -3.487550801365593589, -2.228590825266444586, -2.752080473201636401 ) ) ;
#3524 = DIRECTION ( 'NONE',  ( -1.000000000000000000, -0.000000000000000000, 0.000000000000000000 ) ) ;
#3525 = CARTESIAN_POINT ( 'NONE',  ( 29.18336473368349715, -8.306880066003914820, 0.4367664981562905946 ) ) ;
#3526 = ORIENTED_EDGE ( 'NONE', *, *, #25048, .T. ) ;
#3527 = CARTESIAN_POINT ( 'NONE',  ( -2.330754651808268490E-16, -2.718385644597144157, -4.208382051008221048 ) ) ;
#3528 = ORIENTED_EDGE ( 'NONE', *, *, #1897, .T. ) ;
#3529 = PERSON_AND_ORGANIZATION ( #6766, #25292 ) ;
#3530 = CARTESIAN_POINT ( 'NONE',  ( 85.03579748202663779, -5.204477564423076963, 3.993433529915562108 ) ) ;
#3531 = ADVANCED_FACE ( 'NONE', ( #30381, #23006 ), #12306, .F. ) ;
#3532 = CYLINDRICAL_SURFACE ( 'NONE', #15744, 3.000000000000000444 ) ;
#3533 = ORIENTED_EDGE ( 'NONE', *, *, #27058, .T. ) ;
#3534 = CARTESIAN_POINT ( 'NONE',  ( 0.000000000000000000, 0.000000000000000000, 0.000000000000000000 ) ) ;
#3535 = ORIENTED_EDGE ( 'NONE', *, *, #11689, .F. ) ;
#3536 = ORIENTED_EDGE ( 'NONE', *, *, #10798, .F. ) ;
#3537 = CARTESIAN_POINT ( 'NONE',  ( 1.394036994807608625E-16, 1.625881193364697719, 4.467071865485476856 ) ) ;
#3538 = CARTESIAN_POINT ( 'NONE',  ( -3.512550801365593944, -3.675193018007245627, 1.088641768524163389 ) ) ;
#3539 = CARTESIAN_POINT ( 'NONE',  ( 8.970430173841169363, -11.86789775953564785, 1.499999999999999778 ) ) ;
#3540 = DIRECTION ( 'NONE',  ( 1.000000000000000000, 0.000000000000000000, 0.000000000000000000 ) ) ;
#3542 = VERTEX_POINT ( 'NONE', #2629 ) ;
#3541 = CARTESIAN_POINT ( 'NONE',  ( 11.68041589746584208, 4.858256445636988552, -1.499999999999999778 ) ) ;
#3543 = CARTESIAN_POINT ( 'NONE',  ( -5.687550801365593323, 2.752080473201636845, -2.228590825266444142 ) ) ;
#3544 = CARTESIAN_POINT ( 'NONE',  ( 21.51801198777054935, 16.55905037250783352, 1.050000000000117284 ) ) ;
#3545 = CARTESIAN_POINT ( 'NONE',  ( 17.39502519978892892, -21.04076415203781636, 1.751145182513948129 ) ) ;
#3546 = CARTESIAN_POINT ( 'NONE',  ( 22.42250000136559507, 1.913930629741522838, -2.363507492473150062 ) ) ;
#3548 = VERTEX_POINT ( 'NONE', #2125 ) ;
#3547 = DIRECTION ( 'NONE',  ( 0.7222222222222220989, 0.000000000000000000, -0.6916610887771519334 ) ) ;
#3549 = CARTESIAN_POINT ( 'NONE',  ( 10.55147673363119232, 2.376879293651063652, 4.116875700062091248 ) ) ;
#3550 = CARTESIAN_POINT ( 'NONE',  ( 21.86000000273118715, -1.942864903642428587, -1.573300977624592756 ) ) ;
#3551 = ADVANCED_FACE ( 'NONE', ( #22523, #7452, #17654 ), #15473, .T. ) ;
#3552 = CARTESIAN_POINT ( 'NONE',  ( -18.25325501504504189, 6.775292334730776744, 2.070007460140761868 ) ) ;
#3553 = CARTESIAN_POINT ( 'NONE',  ( 101.8667766209797634, -4.980100140098701722, -2.484925282884729913 ) ) ;
#3554 = DIRECTION ( 'NONE',  ( -0.000000000000000000, -0.000000000000000000, 1.000000000000000000 ) ) ;
#3555 = DIRECTION ( 'NONE',  ( -1.000000000000000000, -0.000000000000000000, -0.000000000000000000 ) ) ;
#3556 = DIRECTION ( 'NONE',  ( 0.1027947991993877208, -0.9947025833170222153, 0.000000000000000000 ) ) ;
#3557 = CARTESIAN_POINT ( 'NONE',  ( -7.037550801365593856, 1.088641768524161613, 3.675193018007247403 ) ) ;
#3558 = VERTEX_POINT ( 'NONE', #17845 ) ;
#3559 = CARTESIAN_POINT ( 'NONE',  ( 6.524595126109737464, 8.397268106035244983, -2.112519041817527032 ) ) ;
#3561 = DIRECTION ( 'NONE',  ( -1.000000000000000000, 0.000000000000000000, -0.000000000000000000 ) ) ;
#3560 = CARTESIAN_POINT ( 'NONE',  ( 10.52034268205830614, 3.407865132560178978, 3.672404558090050397 ) ) ;
#3562 = EDGE_CURVE ( 'NONE', #29777, #15458, #20850, .T. ) ;
#3563 = ORIENTED_EDGE ( 'NONE', *, *, #22450, .T. ) ;
#3564 = ADVANCED_FACE ( 'NONE', ( #18006 ), #28193, .F. ) ;
#3565 = CYLINDRICAL_SURFACE ( 'NONE', #15539, 2.999999999999999112 ) ;
#3566 = ORIENTED_EDGE ( 'NONE', *, *, #346, .F. ) ;
#3567 = DIRECTION ( 'NONE',  ( 0.000000000000000000, 0.000000000000000000, 1.000000000000000000 ) ) ;
#3568 = ADVANCED_FACE ( 'NONE', ( #28842 ), #8132, .T. ) ;
#3570 = ORIENTED_EDGE ( 'NONE', *, *, #1166, .T. ) ;
#3569 = CARTESIAN_POINT ( 'NONE',  ( -2.600000000000000089, 0.000000000000000000, 1.000000000000000000 ) ) ;
#3571 = ORIENTED_EDGE ( 'NONE', *, *, #8596, .T. ) ;
#3572 = DIRECTION ( 'NONE',  ( -4.917867153433088392E-17, -0.5735764363510558184, 0.8191520442889849152 ) ) ;
#3573 = DIRECTION ( 'NONE',  ( -1.000000000000000000, 0.000000000000000000, 0.000000000000000000 ) ) ;
#3575 = ORIENTED_EDGE ( 'NONE', *, *, #9562, .T. ) ;
#3574 = CARTESIAN_POINT ( 'NONE',  ( 107.9617357165269595, 17.96508929613819916, 3.877315172376031960 ) ) ;
#3576 = CARTESIAN_POINT ( 'NONE',  ( 15.22955465171501999, 10.73977884020718854, -1.500000000000000000 ) ) ;
#3577 = CARTESIAN_POINT ( 'NONE',  ( -2.767073886773233848, -0.6621507858625382825, -1.748408842879326075 ) ) ;
#3578 = CARTESIAN_POINT ( 'NONE',  ( 3.499999999999999556, -6.700937042937042065, -2.183447440113257976 ) ) ;
#3579 = CARTESIAN_POINT ( 'NONE',  ( 7.502484982175676720, -10.19046547981761996, -1.500000000000000000 ) ) ;
#3580 = CARTESIAN_POINT ( 'NONE',  ( -50.81000000000000227, -10.96999999999998643, 8.628141679950115162 ) ) ;
#3581 = LINE ( 'NONE', #8897, #219 ) ;
#3582 = DIRECTION ( 'NONE',  ( -0.000000000000000000, -0.3746065934159164001, 0.9271838545667856479 ) ) ;
#3583 = CARTESIAN_POINT ( 'NONE',  ( 3.063284526839887167, 0.000000000000000000, 0.000000000000000000 ) ) ;
#3584 = CARTESIAN_POINT ( 'NONE',  ( 2.386646147131364248, -0.3554301312245136679, 1.500000000000000000 ) ) ;
#3585 = ORIENTED_EDGE ( 'NONE', *, *, #2301, .T. ) ;
#3586 = CARTESIAN_POINT ( 'NONE',  ( 0.000000000000000000, 8.264486777890107660, 4.472189673936814991 ) ) ;
#3587 = DIRECTION ( 'NONE',  ( 0.000000000000000000, 0.000000000000000000, 1.000000000000000000 ) ) ;
#3588 = FACE_OUTER_BOUND ( 'NONE', #26645, .T. ) ;
#3589 = ORIENTED_EDGE ( 'NONE', *, *, #25118, .F. ) ;
#3590 = ADVANCED_FACE ( 'NONE', ( #5943 ), #10801, .F. ) ;
#3591 = B_SPLINE_CURVE_WITH_KNOTS ( 'NONE', 3,
 ( #23285, #28773, #15402, #25611, #2725, #23121 ),
 .UNSPECIFIED., .F., .F.,
 ( 4, 2, 4 ),
 ( 0.01682075285868001036, 0.5000000000000000000, 0.5131349204668873565 ),
 .UNSPECIFIED. ) ;
#3592 = CARTESIAN_POINT ( 'NONE',  ( 25.53801055518932017, -0.6886950482053056932, -2.722715053693994136 ) ) ;
#3593 = CARTESIAN_POINT ( 'NONE',  ( 20.06012370291101732, -21.48645126995936039, 1.642756992391390947 ) ) ;
#3594 = ORIENTED_EDGE ( 'NONE', *, *, #244, .F. ) ;
#3595 = DIRECTION ( 'NONE',  ( -0.000000000000000000, -0.000000000000000000, -1.000000000000000000 ) ) ;
#3596 = DIRECTION ( 'NONE',  ( 1.000000000000000000, 0.000000000000000000, 0.000000000000000000 ) ) ;
#3597 = ADVANCED_FACE ( 'NONE', ( #23677 ), #31227, .T. ) ;
#3598 = ORIENTED_EDGE ( 'NONE', *, *, #17572, .T. ) ;
#3599 = EDGE_CURVE ( 'NONE', #442, #21233, #21387, .T. ) ;
#3600 = ORIENTED_EDGE ( 'NONE', *, *, #17718, .F. ) ;
#3601 = CARTESIAN_POINT ( 'NONE',  ( 25.34157222223566919, -17.52646456585300072, -1.103933258152206776 ) ) ;
#3602 = B_SPLINE_SURFACE_WITH_KNOTS ( 'NONE', 1, 3, ( 
 ( #12924, #7916, #2254, #25634, #10258, #25823, #12443, #30849, #17793, #22657, #13103, #20296, #17451, #23304, #27649, #15110 ),
 ( #406, #5249, #15424, #28303, #2433, #17605, #14924, #22955, #15273, #25476, #32861, #20484, #12602, #2750, #10082, #22805 ) ),
 .UNSPECIFIED., .F., .F., .F.,
 ( 2, 2 ),
 ( 4, 2, 2, 2, 2, 2, 2, 4 ),
 ( 0.000000000000000000, 1.000000000000000000 ),
 ( 0.000000000000000000, 0.5000000000000000000, 0.6250000000000000000, 0.7500000000000000000, 0.8125000000000000000, 0.8750000000000000000, 0.9375000000000000000, 1.000000000000000000 ),
 .UNSPECIFIED. ) ;
#3604 = EDGE_LOOP ( 'NONE', ( #12021, #24451, #5651, #251 ) ) ;
#3603 = CARTESIAN_POINT ( 'NONE',  ( 0.6708088701982988233, 0.000000000000000000, 4.629213727441584325 ) ) ;
#3605 = VERTEX_POINT ( 'NONE', #10630 ) ;
#3606 = CARTESIAN_POINT ( 'NONE',  ( 0.000000000000000000, 0.000000000000000000, 0.000000000000000000 ) ) ;
#3607 = ORIENTED_EDGE ( 'NONE', *, *, #32615, .T. ) ;
#3608 = CARTESIAN_POINT ( 'NONE',  ( 109.3993806922052840, 20.31298924473512457, -2.334455007174283558 ) ) ;
#3609 = DIRECTION ( 'NONE',  ( 1.000000000000000000, -8.574039729943018344E-17, -0.000000000000000000 ) ) ;
#3611 = VERTEX_POINT ( 'NONE', #16138 ) ;
#3610 = CARTESIAN_POINT ( 'NONE',  ( 54.90427307175370686, -3.885678510653091777, -1.529339875078414179 ) ) ;
#3612 = DIRECTION ( 'NONE',  ( 1.000000000000000000, 0.000000000000000000, -0.000000000000000000 ) ) ;
#3613 = CARTESIAN_POINT ( 'NONE',  ( 10.00000000000000000, 3.024842911000744650, -3.993798362933278057 ) ) ;
#3614 = CARTESIAN_POINT ( 'NONE',  ( 9.350000000000001421, 0.000000000000000000, -1.000000000000000000 ) ) ;
#3615 = CARTESIAN_POINT ( 'NONE',  ( -3.449949199999996274, 0.000000000000000000, -6.000000000000000888 ) ) ;
#3616 = CARTESIAN_POINT ( 'NONE',  ( 108.0606459309291267, -18.94264843518903163, 4.540289307709638678 ) ) ;
#3617 = CARTESIAN_POINT ( 'NONE',  ( 10.00000000000000000, -4.116875700062067267, -2.376879293651108060 ) ) ;
#3618 = CARTESIAN_POINT ( 'NONE',  ( 47.95865874067742851, -8.381244160376988717, -0.8105615599411728489 ) ) ;
#3619 = FACE_OUTER_BOUND ( 'NONE', #22284, .T. ) ;
#3620 = CARTESIAN_POINT ( 'NONE',  ( -1.394036994807583480E-16, -1.625881193364668409, -4.467071865485488402 ) ) ;
#3621 = CARTESIAN_POINT ( 'NONE',  ( 7.249760686538667009, 2.741043480754926875, 7.530955069117522882 ) ) ;
#3622 = CARTESIAN_POINT ( 'NONE',  ( -1.361091220733346370E-15, -7.944914065997057406, -7.533794289458144000 ) ) ;
#3623 = FACE_OUTER_BOUND ( 'NONE', #23258, .T. ) ;
#3624 = ADVANCED_FACE ( 'NONE', ( #23344 ), #943, .F. ) ;
#3625 = CARTESIAN_POINT ( 'NONE',  ( 108.1156589233279419, 18.82219444680297116, 4.414476567109417715 ) ) ;
#3626 = CARTESIAN_POINT ( 'NONE',  ( -2.912550801365593411, 1.088641768524161613, 3.675193018007247403 ) ) ;
#3627 = ORIENTED_EDGE ( 'NONE', *, *, #20596, .F. ) ;
#3628 = CARTESIAN_POINT ( 'NONE',  ( -6.500050800000000351, -0.3135853898029607456, 2.983565686104819648 ) ) ;
#3629 = EDGE_CURVE ( 'NONE', #31255, #25309, #796, .T. ) ;
#3630 = CARTESIAN_POINT ( 'NONE',  ( 108.1105447920915594, 18.79371694613778843, 4.475313644716053751 ) ) ;
#3631 = EDGE_CURVE ( 'NONE', #112, #31964, #6366, .T. ) ;
#3632 = CARTESIAN_POINT ( 'NONE',  ( 3.499999999999999556, 7.008469740302802897, 0.7425307242148009301 ) ) ;
#3633 = CARTESIAN_POINT ( 'NONE',  ( 6.976285486575339867, -4.435383624114959566, 1.500000000000000000 ) ) ;
#3634 = ORIENTED_EDGE ( 'NONE', *, *, #24801, .F. ) ;
#3635 = CARTESIAN_POINT ( 'NONE',  ( 6.963573770753527903, -4.510305581628758276, -1.500000000000000222 ) ) ;
#3636 = EDGE_CURVE ( 'NONE', #7325, #6067, #8021, .T. ) ;
#3637 =( BOUNDED_SURFACE ( )  B_SPLINE_SURFACE ( 3, 2, ( 
 ( #12855, #2184, #30436 ),
 ( #15368, #12371, #22591 ),
 ( #10188, #20410, #19924 ),
 ( #30628, #2683, #19735 ) ),
 .UNSPECIFIED., .F., .F., .F. ) 
 B_SPLINE_SURFACE_WITH_KNOTS ( ( 4, 4 ),
 ( 3, 3 ),
 ( 0.003849315137956214883, 0.007259385487753089797 ),
 ( 0.000000000000000000, 1.000000000000000000 ),
 .UNSPECIFIED. ) 
 GEOMETRIC_REPRESENTATION_ITEM ( )  RATIONAL_B_SPLINE_SURFACE ( (
 ( 1.000000000000000000, 0.7074525376973934687, 1.000000000000000000),
 ( 1.000000000000000000, 0.7074519917813385517, 1.000000000000000000),
 ( 1.000000000000000000, 0.7074511013186139952, 1.000000000000000000),
 ( 1.000000000000000000, 0.7074498840443294023, 1.000000000000000000) ) ) 
 REPRESENTATION_ITEM ( '' )  SURFACE ( )  );
#3638 = ORIENTED_EDGE ( 'NONE', *, *, #32426, .T. ) ;
#3639 = CARTESIAN_POINT ( 'NONE',  ( 5.543469847163194686, -12.78081252332906637, 1.500000000000000000 ) ) ;
#3640 = DATE_AND_TIME ( #28565, #15699 ) ;
#3641 = EDGE_CURVE ( 'NONE', #22465, #17163, #32066, .T. ) ;
#3642 = CARTESIAN_POINT ( 'NONE',  ( 18.84046687333678705, -4.960482910705372284, 4.215290389460252918 ) ) ;
#3643 = CARTESIAN_POINT ( 'NONE',  ( 10.55147673363119232, -4.458382051008210389, 2.285372942704937849 ) ) ;
#3644 = CARTESIAN_POINT ( 'NONE',  ( 25.75999999999999801, -2.208672634433321348E-15, 0.000000000000000000 ) ) ;
#3645 = CARTESIAN_POINT ( 'NONE',  ( 10.00000000000000178, -1.946309384392625796, 4.616489984850526085 ) ) ;
#3646 = ORIENTED_EDGE ( 'NONE', *, *, #19376, .T. ) ;
#3647 = CARTESIAN_POINT ( 'NONE',  ( 0.08034255810681192878, 7.347818361010405752, 7.899847910286047714 ) ) ;
#3648 = CARTESIAN_POINT ( 'NONE',  ( 10.52034268205830259, -3.641590349731909537, -3.055657119358837992 ) ) ;
#3649 = CARTESIAN_POINT ( 'NONE',  ( 2.976845824368060445, -4.933977349953521774, -7.725179967474431919 ) ) ;
#3650 = ADVANCED_FACE ( 'NONE', ( #13459 ), #8610, .F. ) ;
#3652 = VERTEX_POINT ( 'NONE', #13628 ) ;
#3651 = CARTESIAN_POINT ( 'NONE',  ( 4.749760686538667009, 6.940565734314597002, 4.007137495034836405 ) ) ;
#3653 = DIRECTION ( 'NONE',  ( 8.574039729943018344E-17, 1.000000000000000000, 0.000000000000000000 ) ) ;
#3654 = CARTESIAN_POINT ( 'NONE',  ( 18.60865963056891559, -7.551622653696671073, 0.8125824237645643544 ) ) ;
#3655 = CARTESIAN_POINT ( 'NONE',  ( 0.7632845268398871230, 0.000000000000000000, 0.000000000000000000 ) ) ;
#3656 = VERTEX_POINT ( 'NONE', #10073 ) ;
#3657 = CARTESIAN_POINT ( 'NONE',  ( 3.499999999999999556, -7.009698679648292519, 0.7308381473896670144 ) ) ;
#3658 = CARTESIAN_POINT ( 'NONE',  ( -56.71071518287084245, 0.7496615022747109558, -1.050000000000000044 ) ) ;
#3659 = CARTESIAN_POINT ( 'NONE',  ( -2.386718424894570312, -9.330009425478156260, 4.522129901861159595 ) ) ;
#3660 = EDGE_LOOP ( 'NONE', ( #1413, #2946, #17487, #27296 ) ) ;
#3661 = DIRECTION ( 'NONE',  ( 0.000000000000000000, 0.000000000000000000, 1.000000000000000000 ) ) ;
#3662 = VERTEX_POINT ( 'NONE', #22646 ) ;
#3663 = FACE_OUTER_BOUND ( 'NONE', #9917, .T. ) ;
#3664 = CARTESIAN_POINT ( 'NONE',  ( -2.102220961135812693, 1.255248584792989064, 3.273767578062598105 ) ) ;
#3665 = CARTESIAN_POINT ( 'NONE',  ( -4.337550801365594566, -3.368539882008727115, -1.828967928396027842 ) ) ;
#3666 = EDGE_CURVE ( 'NONE', #29657, #4019, #252, .T. ) ;
#3667 = DIRECTION ( 'NONE',  ( 0.8660254037844409281, -0.4999999999999960587, 0.000000000000000000 ) ) ;
#3668 = CARTESIAN_POINT ( 'NONE',  ( 0.7632845268398871230, 7.360373001730917686, 4.729683950898899703 ) ) ;
#3669 = ORIENTED_EDGE ( 'NONE', *, *, #15669, .F. ) ;
#3670 = DIRECTION ( 'NONE',  ( 0.000000000000000000, 0.000000000000000000, 1.000000000000000000 ) ) ;
#3671 = ADVANCED_FACE ( 'NONE', ( #30984 ), #2739, .F. ) ;
#3672 = ORIENTED_EDGE ( 'NONE', *, *, #30420, .F. ) ;
#3673 = DATE_AND_TIME ( #3361, #21546 ) ;
#3674 = CARTESIAN_POINT ( 'NONE',  ( 28.66410178491977945, -6.765307663810779637, 3.993434336021463693 ) ) ;
#3675 = ADVANCED_FACE ( 'NONE', ( #10249 ), #17924, .F. ) ;
#3676 = CARTESIAN_POINT ( 'NONE',  ( -23.35000000000000142, -10.96966150227469505, -1.500000000000000000 ) ) ;
#3677 = ORIENTED_EDGE ( 'NONE', *, *, #31861, .T. ) ;
#3678 = FACE_OUTER_BOUND ( 'NONE', #399, .T. ) ;
#3679 = ORIENTED_EDGE ( 'NONE', *, *, #7930, .F. ) ;
#3680 = VERTEX_POINT ( 'NONE', #12742 ) ;
#3681 = CARTESIAN_POINT ( 'NONE',  ( -8.000050800000000351, 0.000000000000000000, -3.000000000000000444 ) ) ;
#3682 = CARTESIAN_POINT ( 'NONE',  ( -5.112550801365594033, -3.675193018007245627, 1.088641768524163389 ) ) ;
#3683 = CARTESIAN_POINT ( 'NONE',  ( 22.61000000000000298, -1.942864903642428587, -1.573300977624592756 ) ) ;
#3684 = EDGE_CURVE ( 'NONE', #21342, #8558, #2936, .T. ) ;
#3685 = B_SPLINE_CURVE_WITH_KNOTS ( 'NONE', 3,
 ( #21048, #23224, #15694, #25900 ),
 .UNSPECIFIED., .F., .F.,
 ( 4, 4 ),
 ( -5.999999996298584598E-08, 0.0003583794985564089713 ),
 .UNSPECIFIED. ) ;
#3686 = CARTESIAN_POINT ( 'NONE',  ( 1.205419605580912767, -3.374343154704484427, -1.499999999999999556 ) ) ;
#3687 = CC_DESIGN_PERSON_AND_ORGANIZATION_ASSIGNMENT ( #27524, #15144, ( #8747 ) ) ;
#3689 = ORIENTED_EDGE ( 'NONE', *, *, #31553, .F. ) ;
#3688 = DIRECTION ( 'NONE',  ( -1.000000000000000000, 0.000000000000000000, -0.000000000000000000 ) ) ;
#3690 = CARTESIAN_POINT ( 'NONE',  ( -6.137550801365595277, -1.828967928396026510, 3.368539882008728004 ) ) ;
#3691 = CARTESIAN_POINT ( 'NONE',  ( 11.28219953675240994, 4.179024087153581313, 1.500000000000000000 ) ) ;
#3692 = DIRECTION ( 'NONE',  ( -1.000000000000000000, 0.000000000000000000, -0.000000000000000000 ) ) ;
#3693 = CARTESIAN_POINT ( 'NONE',  ( 0.7632845268398888994, -6.772677083992417302, 5.538577986808867593 ) ) ;
#3695 = ORIENTED_EDGE ( 'NONE', *, *, #24874, .T. ) ;
#3694 = CARTESIAN_POINT ( 'NONE',  ( 2.661997781067675817, -3.981025027156562590, 9.315861390595092217 ) ) ;
#3696 = CARTESIAN_POINT ( 'NONE',  ( -41.30970132048468457, -16.45499999999997343, 1.500000000000000000 ) ) ;
#3697 = CARTESIAN_POINT ( 'NONE',  ( 25.29647048078943783, -17.54044502839390773, 1.294083243069050093 ) ) ;
#3698 = CARTESIAN_POINT ( 'NONE',  ( 101.8797206818349821, -5.166491396337139719, -2.184956718990371805 ) ) ;
#3699 = CARTESIAN_POINT ( 'NONE',  ( -4.272733292961548912, -6.150071936795129091, -1.499999999999920064 ) ) ;
#3700 = CARTESIAN_POINT ( 'NONE',  ( 0.08034255810714203971, -7.347818361009576194, -7.899847910285872743 ) ) ;
#3701 = B_SPLINE_CURVE_WITH_KNOTS ( 'NONE', 3,
 ( #25976, #31169, #8069, #7580, #28293, #25626, #15265, #12916 ),
 .UNSPECIFIED., .F., .F.,
 ( 4, 2, 2, 4 ),
 ( 0.000000000000000000, 0.5000000000000000000, 0.7500000000000000000, 1.000000000000000000 ),
 .UNSPECIFIED. ) ;
#3702 = EDGE_CURVE ( 'NONE', #30241, #17653, #25895, .T. ) ;
#3703 = CARTESIAN_POINT ( 'NONE',  ( 9.284416849710916964, 0.2200169608700019708, 1.043104428712757326 ) ) ;
#3704 = CARTESIAN_POINT ( 'NONE',  ( 107.8806307222008627, -16.35047421165092985, 1.384330804614037236 ) ) ;
#3705 = ORIENTED_EDGE ( 'NONE', *, *, #5410, .F. ) ;
#3706 = B_SPLINE_CURVE_WITH_KNOTS ( 'NONE', 3,
 ( #11653, #22201, #16994, #29728, #11822, #6806, #16844, #14481, #26884, #14311, #1633, #12003 ),
 .UNSPECIFIED., .F., .F.,
 ( 4, 2, 2, 2, 2, 4 ),
 ( 3.496446946337351263E-18, 0.0007549536553621100056, 0.001132430483043158232, 0.001321168896883682942, 0.001415538103803949633, 0.001509907310724215891 ),
 .UNSPECIFIED. ) ;
#3707 = DIRECTION ( 'NONE',  ( 0.000000000000000000, 0.000000000000000000, -1.000000000000000000 ) ) ;
#3708 = CARTESIAN_POINT ( 'NONE',  ( -17.85000000000000142, -10.96966150227469505, 4.500000000000000888 ) ) ;
#3710 = CARTESIAN_POINT ( 'NONE',  ( 107.9801083150606900, -17.78292680192075892, 4.320020057268043168 ) ) ;
#3709 = CARTESIAN_POINT ( 'NONE',  ( -40.61087657765956038, -10.96999999999998643, 5.871858320049875957 ) ) ;
#3711 = ORIENTED_EDGE ( 'NONE', *, *, #7202, .T. ) ;
#3712 = VECTOR ( 'NONE', #5463, 1000.000000000000114 ) ;
#3713 = FACE_OUTER_BOUND ( 'NONE', #1256, .T. ) ;
#3714 = ORIENTED_EDGE ( 'NONE', *, *, #23741, .F. ) ;
#3715 = CARTESIAN_POINT ( 'NONE',  ( 21.36097421961356702, -21.76718868951428121, -1.410897148389125277 ) ) ;
#3717 = ORIENTED_EDGE ( 'NONE', *, *, #32659, .F. ) ;
#3716 = CARTESIAN_POINT ( 'NONE',  ( 69.01329431673670456, -4.971603792614007311, -3.995971199217486447 ) ) ;
#3718 = VERTEX_POINT ( 'NONE', #32850 ) ;
#3719 = DIRECTION ( 'NONE',  ( 8.574039729943018344E-17, 1.000000000000000000, 0.000000000000000000 ) ) ;
#3720 = EDGE_CURVE ( 'NONE', #2084, #25735, #5358, .T. ) ;
#3721 = FACE_OUTER_BOUND ( 'NONE', #31944, .T. ) ;
#3722 = EDGE_LOOP ( 'NONE', ( #6797, #26155, #30190, #21610 ) ) ;
#3723 = CARTESIAN_POINT ( 'NONE',  ( 14.33714415250651797, 9.363647757017387718, -1.500000000000000000 ) ) ;
#3724 = CARTESIAN_POINT ( 'NONE',  ( 0.6621927554280921946, -15.34504050551903021, -1.745995324132502136 ) ) ;
#3725 = DIRECTION ( 'NONE',  ( 7.023442172597838372E-17, 0.8191520442889889120, 0.5735764363510502672 ) ) ;
#3726 = B_SPLINE_CURVE_WITH_KNOTS ( 'NONE', 3,
 ( #3153, #18175, #28383, #30762, #23364, #3010, #13311, #7833 ),
 .UNSPECIFIED., .F., .F.,
 ( 4, 2, 2, 4 ),
 ( 5.099451029799059509E-07, 0.001229189756374614957, 0.001843529662010432151, 0.002457869567646249562 ),
 .UNSPECIFIED. ) ;
#3727 = CARTESIAN_POINT ( 'NONE',  ( 15.81086013942911350, -14.68957281887592892, -0.9999999999999995559 ) ) ;
#3728 = CARTESIAN_POINT ( 'NONE',  ( 107.9802527803231129, -17.78500706576168611, -4.325704939595124365 ) ) ;
#3729 = CARTESIAN_POINT ( 'NONE',  ( 35.00000000000000000, 0.000000000000000000, -2.999999999999995559 ) ) ;
#3730 = CIRCLE ( 'NONE', #20815, 8.749000000000002331 ) ;
#3731 = VECTOR ( 'NONE', #13612, 1000.000000000000000 ) ;
#3732 = CARTESIAN_POINT ( 'NONE',  ( 2.976845773540292228, 3.349682859779612443, -8.532418605434688885 ) ) ;
#3733 = DIRECTION ( 'NONE',  ( 0.000000000000000000, -0.9271838545667856479, -0.3746065934159162891 ) ) ;
#3734 = EDGE_CURVE ( 'NONE', #3159, #27553, #30330, .T. ) ;
#3735 = CARTESIAN_POINT ( 'NONE',  ( 0.9232102171129938917, 0.000000000000000000, -4.522129901861164925 ) ) ;
#3736 = CARTESIAN_POINT ( 'NONE',  ( -8.000050800000000351, 0.000000000000000000, 0.000000000000000000 ) ) ;
#3737 = VECTOR ( 'NONE', #17304, 999.9999999999998863 ) ;
#3738 = ORIENTED_EDGE ( 'NONE', *, *, #4844, .F. ) ;
#3739 = DIRECTION ( 'NONE',  ( -7.023442172597853164E-17, -0.8191520442889907994, -0.5735764363510474917 ) ) ;
#3740 = ADVANCED_FACE ( 'NONE', ( #2422 ), #4914, .F. ) ;
#3741 = CARTESIAN_POINT ( 'NONE',  ( 8.901867736793462882, 0.07845480144340738482, -1.317219896051736505 ) ) ;
#3742 = ORIENTED_EDGE ( 'NONE', *, *, #16546, .F. ) ;
#3743 = DIRECTION ( 'NONE',  ( 1.000000000000000000, 0.000000000000000000, 0.000000000000000000 ) ) ;
#3744 = FACE_OUTER_BOUND ( 'NONE', #13307, .T. ) ;
#3745 = EDGE_LOOP ( 'NONE', ( #15810, #6831, #9396, #4234, #28439 ) ) ;
#3746 = DIRECTION ( 'NONE',  ( 0.8660254037844399289, -0.4999999999999977796, 0.000000000000000000 ) ) ;
#3747 = VERTEX_POINT ( 'NONE', #5088 ) ;
#3748 = AXIS2_PLACEMENT_3D ( 'NONE', #30855, #7300, #5256 ) ;
#3749 = VECTOR ( 'NONE', #8442, 1000.000000000000000 ) ;
#3750 = ORIENTED_EDGE ( 'NONE', *, *, #4512, .T. ) ;
#3751 = CARTESIAN_POINT ( 'NONE',  ( 23.90742340928847653, -3.204431202321702088, -2.713652344655540727 ) ) ;
#3752 = ITEM_DEFINED_TRANSFORMATION ( 'NONE', 'NONE', #15113,  #2865 ) ;
#3754 = ORIENTED_EDGE ( 'NONE', *, *, #21592, .F. ) ;
#3753 = DIRECTION ( 'NONE',  ( -1.000000000000000000, 8.574039729943019576E-17, -0.000000000000000000 ) ) ;
#3755 = ORIENTED_EDGE ( 'NONE', *, *, #17169, .T. ) ;
#3756 = CARTESIAN_POINT ( 'NONE',  ( 25.36000000136559507, 0.9349337715887185984, -3.156283516753368268 ) ) ;
#3757 = VERTEX_POINT ( 'NONE', #17951 ) ;
#3759 = AXIS2_PLACEMENT_3D ( 'NONE', #27541, #22850, #20037 ) ;
#3758 = FACE_OUTER_BOUND ( 'NONE', #8118, .T. ) ;
#3760 = CARTESIAN_POINT ( 'NONE',  ( 6.530491627857222703, -7.903708701126667791, -3.540416224243748466 ) ) ;
#3762 = ORIENTED_EDGE ( 'NONE', *, *, #8415, .T. ) ;
#3761 = CARTESIAN_POINT ( 'NONE',  ( 47.88260332741770497, -3.822977517009024329, -0.4367665431853247071 ) ) ;
#3763 = CARTESIAN_POINT ( 'NONE',  ( 21.61000000273118715, -1.573300977624594976, 1.942864903642425700 ) ) ;
#3764 = CARTESIAN_POINT ( 'NONE',  ( 2.274274201625327230, 4.762163868918412923, -9.915734732513168836 ) ) ;
#3765 = CARTESIAN_POINT ( 'NONE',  ( 7.249760686538667009, 0.8180878109961843281, 8.711672189281429723 ) ) ;
#3766 = DIRECTION ( 'NONE',  ( -8.649074885250573632E-15, 0.03489949670250105246, 0.9993908270190957621 ) ) ;
#3767 = FACE_OUTER_BOUND ( 'NONE', #26766, .T. ) ;
#3768 = B_SPLINE_CURVE_WITH_KNOTS ( 'NONE', 3,
 ( #3330, #11151, #7995, #18190 ),
 .UNSPECIFIED., .F., .F.,
 ( 4, 4 ),
 ( 0.000000000000000000, 0.003022500881216731543 ),
 .UNSPECIFIED. ) ;
#3769 = CARTESIAN_POINT ( 'NONE',  ( -1.327193056402532045, -8.327227690482029487, -5.485967528433937979 ) ) ;
#3770 = CARTESIAN_POINT ( 'NONE',  ( 69.15727116336866231, -7.845927800133502217, -0.4367667211789117987 ) ) ;
#3771 = CARTESIAN_POINT ( 'NONE',  ( 14.23800746264082839, 22.11259878822725966, -1.491740999229417941 ) ) ;
#3772 = EDGE_CURVE ( 'NONE', #31510, #10995, #29942, .T. ) ;
#3773 = EDGE_CURVE ( 'NONE', #15394, #6161, #18593, .T. ) ;
#3774 = CONICAL_SURFACE ( 'NONE', #21380, 2.524999999999999911, 0.7853981633974627119 ) ;
#3775 = CARTESIAN_POINT ( 'NONE',  ( 5.489321606599601111, 7.593050043411109229, 2.874206582856435599 ) ) ;
#3776 = DIRECTION ( 'NONE',  ( 0.000000000000000000, 0.000000000000000000, -1.000000000000000000 ) ) ;
#3777 = CYLINDRICAL_SURFACE ( 'NONE', #26315, 0.4999999999999995559 ) ;
#3778 = DIRECTION ( 'NONE',  ( 3.623545766764243588E-17, 0.4226182617407029385, -0.9063077870366482713 ) ) ;
#3779 = CIRCLE ( 'NONE', #12305, 4.000000000000001776 ) ;
#3780 = CARTESIAN_POINT ( 'NONE',  ( 108.0375372059708212, 18.38718189920101764, 4.618926104085890216 ) ) ;
#3781 = CARTESIAN_POINT ( 'NONE',  ( -7.400050802731187538, 0.9222479816126443186, 3.113457007523260156 ) ) ;
#3782 = VERTEX_POINT ( 'NONE', #11068 ) ;
#3783 = CARTESIAN_POINT ( 'NONE',  ( -5.150050800000000706, 3.113457007523260156, -0.9222479816126439855 ) ) ;
#3784 = CIRCLE ( 'NONE', #9102, 2.999999999999999112 ) ;
#3785 = DIRECTION ( 'NONE',  ( -1.000000000000000000, 0.000000000000000000, 0.000000000000000000 ) ) ;
#3786 = PLANE ( 'NONE',  #19329 ) ;
#3787 = CARTESIAN_POINT ( 'NONE',  ( -41.71978369837230360, -15.85293847936788580, 5.221339267391799766 ) ) ;
#3788 = EDGE_LOOP ( 'NONE', ( #25671, #5889, #8770, #4793 ) ) ;
#3789 = CARTESIAN_POINT ( 'NONE',  ( -7.050050800000001061, -2.853674364686378695, -1.549418761218566809 ) ) ;
#3790 = VERTEX_POINT ( 'NONE', #730 ) ;
#3791 = CARTESIAN_POINT ( 'NONE',  ( 0.6081216625945999876, -7.499966554744998071, 1.500000000000000444 ) ) ;
#3792 = PERSON_AND_ORGANIZATION_ROLE ( 'design_owner' ) ;
#3793 = AXIS2_PLACEMENT_3D ( 'NONE', #26516, #14124, #6266 ) ;
#3794 = ORIENTED_EDGE ( 'NONE', *, *, #28410, .F. ) ;
#3795 = VECTOR ( 'NONE', #13925, 1000.000000000000000 ) ;
#3796 = CARTESIAN_POINT ( 'NONE',  ( 28.68519643166255761, -5.941144522469937961, 4.275175838854671007 ) ) ;
#3797 = AXIS2_PLACEMENT_3D ( 'NONE', #30382, #17655, #4979 ) ;
#3798 = AXIS2_PLACEMENT_3D ( 'NONE', #32907, #33053, #17847 ) ;
#3799 = CARTESIAN_POINT ( 'NONE',  ( 19.03654924710325602, -2.768675503676416572, 2.713652344655542503 ) ) ;
#3800 = CARTESIAN_POINT ( 'NONE',  ( 102.3664313161150972, -3.178976151073279244, -4.275175836085992387 ) ) ;
#3801 = VECTOR ( 'NONE', #9121, 1000.000000000000000 ) ;
#3802 = CARTESIAN_POINT ( 'NONE',  ( 21.64180102898196978, -16.89820628832873339, -1.499999999999857447 ) ) ;
#3803 = CARTESIAN_POINT ( 'NONE',  ( 9.578960313758919654, 17.92714876365089793, 5.412820279296879811 ) ) ;
#3804 = ORIENTED_EDGE ( 'NONE', *, *, #8813, .F. ) ;
#3805 = CARTESIAN_POINT ( 'NONE',  ( -3.103431213610433836, -2.413098734550712128E-13, 1.052805373823281210 ) ) ;
#3806 = DIRECTION ( 'NONE',  ( 0.000000000000000000, 0.000000000000000000, 1.000000000000000000 ) ) ;
#3807 = LINE ( 'NONE', #14158, #11914 ) ;
#3808 = CIRCLE ( 'NONE', #27832, 0.5000000000000004441 ) ;
#3809 = EDGE_CURVE ( 'NONE', #28731, #689, #8568, .T. ) ;
#3811 = VERTEX_POINT ( 'NONE', #16400 ) ;
#3810 = CARTESIAN_POINT ( 'NONE',  ( 25.72720924917965846, 2.995293602030530078, 0.1965175717148812951 ) ) ;
#3812 = CARTESIAN_POINT ( 'NONE',  ( -2.862550801365593145, -0.3701630799359326152, 3.521866450007987037 ) ) ;
#3813 = FACE_OUTER_BOUND ( 'NONE', #19385, .T. ) ;
#3814 = DIRECTION ( 'NONE',  ( 0.000000000000000000, 1.000000000000000000, 0.000000000000000000 ) ) ;
#3815 = CYLINDRICAL_SURFACE ( 'NONE', #25303, 0.5000000000000004441 ) ;
#3816 = FACE_OUTER_BOUND ( 'NONE', #19515, .T. ) ;
#3817 = DIRECTION ( 'NONE',  ( 1.000000000000000000, -0.000000000000000000, -0.000000000000000000 ) ) ;
#3818 = CARTESIAN_POINT ( 'NONE',  ( 34.98193025661426248, 0.5174497483512505713, -2.552009564962228527 ) ) ;
#3819 = CARTESIAN_POINT ( 'NONE',  ( -1.023266466338824454, -9.291661594691762005, 5.485967528433933538 ) ) ;
#3820 = ORIENTED_EDGE ( 'NONE', *, *, #24763, .T. ) ;
#3821 = VECTOR ( 'NONE', #3298, 1000.000000000000000 ) ;
#3822 = EDGE_CURVE ( 'NONE', #4740, #436, #28312, .T. ) ;
#3823 = DIRECTION ( 'NONE',  ( 1.000000000000000000, 0.000000000000000000, 0.000000000000000000 ) ) ;
#3824 = ORIENTED_EDGE ( 'NONE', *, *, #10565, .F. ) ;
#3825 = TOROIDAL_SURFACE ( 'NONE', #17676, 7.482234843104714983, 0.5000000000000000000 ) ;
#3826 = CARTESIAN_POINT ( 'NONE',  ( -2.093800801365593323, -0.3135853898029608011, 2.983565686104819648 ) ) ;
#3827 =( BOUNDED_CURVE ( )  B_SPLINE_CURVE ( 2, ( #17173, #12009, #4498 ),
 .UNSPECIFIED., .F., .F. ) 
 B_SPLINE_CURVE_WITH_KNOTS ( ( 3, 3 ),
 ( 0.9353822619934377691, 0.9375000000000000000 ),
 .UNSPECIFIED. ) 
 CURVE ( )  GEOMETRIC_REPRESENTATION_ITEM ( )  RATIONAL_B_SPLINE_CURVE ( ( 0.9821626249036861100, 0.9896829947469995004, 1.000000000000000000 ) ) 
 REPRESENTATION_ITEM ( '' )  );
#3828 = CARTESIAN_POINT ( 'NONE',  ( -2.010643812441442968, 0.9556990460818173272, 3.226324136115746644 ) ) ;
#3829 = AXIS2_PLACEMENT_3D ( 'NONE', #5813, #8174, #31085 ) ;
#3830 = EDGE_CURVE ( 'NONE', #18408, #9983, #18756, .T. ) ;
#3831 = CARTESIAN_POINT ( 'NONE',  ( -2.637550801365593056, -1.088641768524163611, -3.675193018007245627 ) ) ;
#3832 = DIRECTION ( 'NONE',  ( 0.000000000000000000, -0.9271838545667856479, -0.3746065934159165667 ) ) ;
#3833 = CARTESIAN_POINT ( 'NONE',  ( -60.07995281065674931, -10.96999999999998465, 9.000000000000000000 ) ) ;
#3834 = CIRCLE ( 'NONE', #23036, 10.96966150227469328 ) ;
#3835 = VERTEX_POINT ( 'NONE', #10735 ) ;
#3836 = CARTESIAN_POINT ( 'NONE',  ( -59.75626822162180218, -5.804869634004078627, 5.128141679950119602 ) ) ;
#3837 = AXIS2_PLACEMENT_3D ( 'NONE', #29860, #14798, #7285 ) ;
#3838 = VECTOR ( 'NONE', #19351, 1000.000000000000000 ) ;
#3839 = EDGE_LOOP ( 'NONE', ( #5518, #25266, #5761 ) ) ;
#3840 = PERSON_AND_ORGANIZATION_ROLE ( 'creator' ) ;
#3841 = EDGE_CURVE ( 'NONE', #17909, #24949, #31321, .T. ) ;
#3842 = CARTESIAN_POINT ( 'NONE',  ( 12.44989959798868817, 19.50000000000000000, 13.00000000000004441 ) ) ;
#3843 = CYLINDRICAL_SURFACE ( 'NONE', #20861, 8.500000000000000000 ) ;
#3844 = ORIENTED_EDGE ( 'NONE', *, *, #10178, .F. ) ;
#3845 = CARTESIAN_POINT ( 'NONE',  ( 10.00000000000000178, -8.574039729943018837E-16, 0.000000000000000000 ) ) ;
#3846 = ADVANCED_FACE ( 'NONE', ( #544 ), #16116, .T. ) ;
#3847 = ORIENTED_EDGE ( 'NONE', *, *, #6395, .T. ) ;
#3848 = CIRCLE ( 'NONE', #106, 10.52000000000000135 ) ;
#3849 = ORIENTED_EDGE ( 'NONE', *, *, #8074, .F. ) ;
#3850 = CARTESIAN_POINT ( 'NONE',  ( 5.612974441954676763, 6.163896661468974969, 5.432722698947179296 ) ) ;
#3851 = CARTESIAN_POINT ( 'NONE',  ( -5.162550801365593856, -2.752080473201636845, 2.228590825266444586 ) ) ;
#3852 = AXIS2_PLACEMENT_3D ( 'NONE', #13296, #5950, #31532 ) ;
#3853 = CARTESIAN_POINT ( 'NONE',  ( 24.17249999999999943, 1.291182301015469047, 2.378061970571981654 ) ) ;
#3854 = CARTESIAN_POINT ( 'NONE',  ( 1.448939188974345038, -2.783086940837860457, -1.500000000000000000 ) ) ;
#3856 = ORIENTED_EDGE ( 'NONE', *, *, #6396, .T. ) ;
#3855 = CARTESIAN_POINT ( 'NONE',  ( 6.037141869538511507, 3.843044125430171931, -7.552970526864650758 ) ) ;
#3857 = CARTESIAN_POINT ( 'NONE',  ( -5.837550801365594566, -1.088641768524163389, -3.675193018007246071 ) ) ;
#3858 = AXIS2_PLACEMENT_3D ( 'NONE', #12684, #2863, #23236 ) ;
#3859 = PLANE ( 'NONE',  #10177 ) ;
#3860 = CARTESIAN_POINT ( 'NONE',  ( 8.151896291536630201, -19.35435381133223842, 1.499999999999999112 ) ) ;
#3861 = ADVANCED_FACE ( 'NONE', ( #13877 ), #15912, .F. ) ;
#3862 = ORIENTED_EDGE ( 'NONE', *, *, #10983, .F. ) ;
#3864 = ORIENTED_EDGE ( 'NONE', *, *, #22474, .F. ) ;
#3863 = CARTESIAN_POINT ( 'NONE',  ( 12.44989959798868817, 19.50000000000000000, -1.818740222761504599 ) ) ;
#3865 = EDGE_CURVE ( 'NONE', #10650, #7898, #26029, .T. ) ;
#3866 = VECTOR ( 'NONE', #3452, 1000.000000000000000 ) ;
#3867 = DIRECTION ( 'NONE',  ( 0.1503837331804358246, -0.08682408883346498518, -0.9848077530122080203 ) ) ;
#3868 = DIRECTION ( 'NONE',  ( -6.062761635205572056E-17, -0.7071067811865465735, -0.7071067811865484609 ) ) ;
#3869 = CARTESIAN_POINT ( 'NONE',  ( -6.562942409646512765, -8.831141768130910875E-16, 2.999999999999999556 ) ) ;
#3870 = CARTESIAN_POINT ( 'NONE',  ( -4.250504261574428178, -7.586801008987120731, -1.500000000000318190 ) ) ;
#3871 = AXIS2_PLACEMENT_3D ( 'NONE', #18068, #24632, #17742 ) ;
#3872 = LINE ( 'NONE', #21901, #18869 ) ;
#3873 = VECTOR ( 'NONE', #29531, 1000.000000000000000 ) ;
#3874 = CIRCLE ( 'NONE', #23081, 8.750000000000000000 ) ;
#3875 = DIRECTION ( 'NONE',  ( -0.000000000000000000, 0.000000000000000000, 1.000000000000000000 ) ) ;
#3876 = CARTESIAN_POINT ( 'NONE',  ( -3.587550801365593678, -3.521866450007987037, -0.3701630799359323931 ) ) ;
#3877 = CARTESIAN_POINT ( 'NONE',  ( 0.000000000000000000, 19.50000000000000000, 0.000000000000000000 ) ) ;
#3878 = EDGE_LOOP ( 'NONE', ( #31123, #20396, #8363 ) ) ;
#3879 = CONICAL_SURFACE ( 'NONE', #15615, 302.1720608278466216, 0.4915790642873723582 ) ;
#3881 = EDGE_CURVE ( 'NONE', #21586, #9413, #13239, .T. ) ;
#3880 = VECTOR ( 'NONE', #30973, 1000.000000000000000 ) ;
#3882 = CARTESIAN_POINT ( 'NONE',  ( 21.05407077897152845, -21.72523992960347883, 1.419373079978943464 ) ) ;
#3883 = CARTESIAN_POINT ( 'NONE',  ( 7.249760686538667009, 8.466096581343512284, -2.210816291636124475 ) ) ;
#3886 = CARTESIAN_POINT ( 'NONE',  ( 7.249760686538667009, -7.906491560603691404, 3.748318449932265484 ) ) ;
#3885 = FACE_OUTER_BOUND ( 'NONE', #29669, .T. ) ;
#3884 = CIRCLE ( 'NONE', #20975, 8.749000000000002331 ) ;
#3887 = EDGE_LOOP ( 'NONE', ( #8734, #7038, #5437, #23306, #4 ) ) ;
#3888 = VECTOR ( 'NONE', #26251, 1000.000000000000114 ) ;
#3889 = CARTESIAN_POINT ( 'NONE',  ( 21.32535692059155963, -21.82495604402122069, 1.318256435726650633 ) ) ;
#3890 = ORIENTED_EDGE ( 'NONE', *, *, #18641, .T. ) ;
#3891 = CARTESIAN_POINT ( 'NONE',  ( 0.000000000000000000, 9.884132761439062165, 4.709950686174647849 ) ) ;
#3893 = ORIENTED_EDGE ( 'NONE', *, *, #5307, .F. ) ;
#3892 = CARTESIAN_POINT ( 'NONE',  ( 84.96582260358789540, -4.062957753267931515, -3.999772873837519338 ) ) ;
#3894 = ORIENTED_EDGE ( 'NONE', *, *, #9492, .F. ) ;
#3895 = EDGE_CURVE ( 'NONE', #15207, #30146, #28332, .T. ) ;
#3896 = DIRECTION ( 'NONE',  ( -2.219124775575015083E-17, -0.2588190451025310090, 0.9659258262890655367 ) ) ;
#3898 = ORIENTED_EDGE ( 'NONE', *, *, #15879, .T. ) ;
#3897 = CARTESIAN_POINT ( 'NONE',  ( 3.499999999999999556, -2.417132211460119251, 8.149077976821791580 ) ) ;
#3899 = CIRCLE ( 'NONE', #17777, 4.000000000000001776 ) ;
#3900 = CARTESIAN_POINT ( 'NONE',  ( 19.01933586171005786, 14.56926017569804443, -1.050000000000000044 ) ) ;
#3901 = CARTESIAN_POINT ( 'NONE',  ( 10.00000000000000000, 3.641590349731929077, 3.055657119358814011 ) ) ;
#3902 = VECTOR ( 'NONE', #2374, 1000.000000000000000 ) ;
#3903 = CARTESIAN_POINT ( 'NONE',  ( 101.8016823592329274, -4.042758964359259188, -3.993434276136486716 ) ) ;
#3904 = EDGE_CURVE ( 'NONE', #27107, #5903, #18192, .T. ) ;
#3905 = VECTOR ( 'NONE', #10022, 1000.000000000000000 ) ;
#3906 = CARTESIAN_POINT ( 'NONE',  ( 14.03158388662403411, -14.04624128054154042, -0.9999999999999995559 ) ) ;
#3908 = VERTEX_POINT ( 'NONE', #31467 ) ;
#3907 = CARTESIAN_POINT ( 'NONE',  ( 107.4505246733081094, -17.36694227132590029, -4.540110608227355904 ) ) ;
#3909 = ADVANCED_FACE ( 'NONE', ( #8546 ), #3565, .T. ) ;
#3910 = CARTESIAN_POINT ( 'NONE',  ( -4.950050802731188249, -0.3135853898029607456, 2.983565686104819648 ) ) ;
#3911 = AXIS2_PLACEMENT_3D ( 'NONE', #17762, #22931, #30167 ) ;
#3912 = VECTOR ( 'NONE', #23072, 1000.000000000000000 ) ;
#3913 = DIRECTION ( 'NONE',  ( 0.000000000000000000, 0.000000000000000000, -1.000000000000000000 ) ) ;
#3914 = CARTESIAN_POINT ( 'NONE',  ( 3.249999999999999556, -7.360373001730951437, 4.729683950898845524 ) ) ;
#3915 = UNCERTAINTY_MEASURE_WITH_UNIT (LENGTH_MEASURE( 1.000000000000000082E-05 ), #27348, 'distance_accuracy_value', 'NONE');
#3916 = CARTESIAN_POINT ( 'NONE',  ( 0.000000000000000000, 9.314797388894893615, 1.239665997526919972 ) ) ;
#3917 = CARTESIAN_POINT ( 'NONE',  ( 0.7632845268398871230, -5.538577986808947529, 6.772677083992368452 ) ) ;
#3918 = ORIENTED_EDGE ( 'NONE', *, *, #18926, .T. ) ;
#3919 = DIRECTION ( 'NONE',  ( -1.000000000000000000, -0.000000000000000000, -0.000000000000000000 ) ) ;
#3920 = CARTESIAN_POINT ( 'NONE',  ( -23.35000000000000142, -10.96966150227469505, 1.500000000000000000 ) ) ;
#3921 = CARTESIAN_POINT ( 'NONE',  ( 33.81874022276149816, 19.50000000000000000, 1.818740222761735525 ) ) ;
#3922 = ORIENTED_EDGE ( 'NONE', *, *, #26113, .F. ) ;
#3923 = ADVANCED_FACE ( 'NONE', ( #3713 ), #11408, .T. ) ;
#3924 = PRODUCT_RELATED_PRODUCT_CATEGORY ( 'detail', '', ( #32741 ) ) ;
#3925 = AXIS2_PLACEMENT_3D ( 'NONE', #9934, #20149, #30012 ) ;
#3926 = AXIS2_PLACEMENT_3D ( 'NONE', #14174, #9650, #27396 ) ;
#3927 = CARTESIAN_POINT ( 'NONE',  ( 0.000000000000000000, -7.009698679648292519, 0.7308381473896670144 ) ) ;
#3928 = CARTESIAN_POINT ( 'NONE',  ( 78.59573142019985426, 24.17918843217023550, -5.396302277755718357 ) ) ;
#3929 = EDGE_LOOP ( 'NONE', ( #19829, #19666, #1317, #11345 ) ) ;
#3930 = CARTESIAN_POINT ( 'NONE',  ( 19.80242846375582388, -16.61789548659649896, -1.500000000000000222 ) ) ;
#3931 = VERTEX_POINT ( 'NONE', #22260 ) ;
#3932 = AXIS2_PLACEMENT_3D ( 'NONE', #20891, #31109, #16204 ) ;
#3933 = AXIS2_PLACEMENT_3D ( 'NONE', #22236, #16879, #29420 ) ;
#3934 = ORIENTED_EDGE ( 'NONE', *, *, #13642, .T. ) ;
#3935 = DIRECTION ( 'NONE',  ( -7.472768010111378190E-18, -0.08715574274766135776, 0.9961946980917453232 ) ) ;
#3936 = APPROVAL_STATUS ( 'not_yet_approved' ) ;
#3938 = ORIENTED_EDGE ( 'NONE', *, *, #922, .F. ) ;
#3937 = CYLINDRICAL_SURFACE ( 'NONE', #19187, 0.4500000000000025646 ) ;
#3939 = ORIENTED_EDGE ( 'NONE', *, *, #9360, .F. ) ;
#3940 = CARTESIAN_POINT ( 'NONE',  ( 25.17250000136559507, -2.363507492473152283, -1.913930629741525280 ) ) ;
#3941 = EDGE_CURVE ( 'NONE', #10995, #16442, #14220, .T. ) ;
#3942 = ORIENTED_EDGE ( 'NONE', *, *, #19288, .F. ) ;
#3943 = CARTESIAN_POINT ( 'NONE',  ( 17.41559371906258136, 18.02474698348859050, 1.508259000770581615 ) ) ;
#3944 = CARTESIAN_POINT ( 'NONE',  ( 0.5704035945089810378, 2.319683995708331725, -9.255216539914508544 ) ) ;
#3946 = ORIENTED_EDGE ( 'NONE', *, *, #21394, .T. ) ;
#3945 = DIRECTION ( 'NONE',  ( 0.000000000000000000, 0.000000000000000000, 1.000000000000000000 ) ) ;
#3947 = CARTESIAN_POINT ( 'NONE',  ( 15.02212703843154529, 19.50000000000000000, -4.708247362410203252 ) ) ;
#3948 = DIRECTION ( 'NONE',  ( 0.000000000000000000, 0.000000000000000000, -1.000000000000000000 ) ) ;
#3949 = CARTESIAN_POINT ( 'NONE',  ( 101.8933637717135667, -5.362948496614666993, 1.868788700022515181 ) ) ;
#3950 = DIRECTION ( 'NONE',  ( 0.000000000000000000, -0.9993908270190956511, 0.03489949670250104552 ) ) ;
#3951 = VECTOR ( 'NONE', #6880, 1000.000000000000000 ) ;
#3952 = CARTESIAN_POINT ( 'NONE',  ( 6.270432871730932334, -15.60322400927264397, -5.485967528433937979 ) ) ;
#3953 = CARTESIAN_POINT ( 'NONE',  ( 47.95950916398560082, -8.432626694227655761, -0.07017451552783438018 ) ) ;
#3954 = CARTESIAN_POINT ( 'NONE',  ( 10.00000000000000178, -8.574039729943018837E-16, 0.000000000000000000 ) ) ;
#3955 =( REPRESENTATION_RELATIONSHIP ('NONE','NONE', #1085, #13478 ) REPRESENTATION_RELATIONSHIP_WITH_TRANSFORMATION ( #28676 )SHAPE_REPRESENTATION_RELATIONSHIP( ) );
#3956 = AXIS2_PLACEMENT_3D ( 'NONE', #3927, #6397, #1414 ) ;
#3957 = AXIS2_PLACEMENT_3D ( 'NONE', #11100, #8910, #16283 ) ;
#3958 = DIRECTION ( 'NONE',  ( 1.000000000000000000, -0.000000000000000000, -0.000000000000000000 ) ) ;
#3959 = CARTESIAN_POINT ( 'NONE',  ( -3.671580638170519912E-13, 9.620177616658855513, 5.227991826304058343 ) ) ;
#3960 = DIRECTION ( 'NONE',  ( 0.06927878976713691683, -0.9975973382524638833, 0.000000000000000000 ) ) ;
#3961 = VECTOR ( 'NONE', #18221, 1000.000000000000000 ) ;
#3962 = LOCAL_TIME ( 16, 7, 10.00000000000000000, #31736 ) ;
#3963 = CARTESIAN_POINT ( 'NONE',  ( 108.0120074800398982, 18.24502231166869493, 4.476406828366910950 ) ) ;
#3964 = EDGE_CURVE ( 'NONE', #19481, #8502, #21937, .T. ) ;
#3965 = CARTESIAN_POINT ( 'NONE',  ( -5.850050802731187716, 1.887961173149511618, 2.331437884370912705 ) ) ;
#3966 = EDGE_LOOP ( 'NONE', ( #28334, #20833, #28132 ) ) ;
#3967 = CARTESIAN_POINT ( 'NONE',  ( -7.600050800000000883, 2.331437884370912705, -1.887961173149511618 ) ) ;
#3968 = CYLINDRICAL_SURFACE ( 'NONE', #15666, 0.4499999999999999001 ) ;
#3969 = DIRECTION ( 'NONE',  ( -0.1027947991993878318, 0.9947025833170222153, 0.000000000000000000 ) ) ;
#3970 = CARTESIAN_POINT ( 'NONE',  ( 7.230698034991899448, -5.790874021893926304, 1.500000000000000222 ) ) ;
#3971 = ORIENTED_EDGE ( 'NONE', *, *, #26513, .T. ) ;
#3972 = CARTESIAN_POINT ( 'NONE',  ( 0.7632845268398882332, -4.729683950898921019, 7.360373001730893705 ) ) ;
#3973 = AXIS2_PLACEMENT_3D ( 'NONE', #20040, #27866, #25016 ) ;
#3974 = ORIENTED_EDGE ( 'NONE', *, *, #15179, .F. ) ;
#3975 = CARTESIAN_POINT ( 'NONE',  ( 3.091298606786377245, -11.74967118460379467, 1.759199775826757017 ) ) ;
#3976 = DATE_AND_TIME ( #6789, #8237 ) ;
#3977 = CARTESIAN_POINT ( 'NONE',  ( 6.524595623740805372, 6.028129343649612615, 6.215987993068464945 ) ) ;
#3978 = VERTEX_POINT ( 'NONE', #29278 ) ;
#3979 = CARTESIAN_POINT ( 'NONE',  ( 40.88018956635887946, -6.197502223173953162, 4.312042181588143563 ) ) ;
#3980 = EDGE_CURVE ( 'NONE', #1891, #4614, #1703, .T. ) ;
#3981 = EDGE_CURVE ( 'NONE', #19878, #30724, #3784, .T. ) ;
#3982 = CARTESIAN_POINT ( 'NONE',  ( -5.950050800000000528, 3.113457007523260156, -0.9222479816126439855 ) ) ;
#3983 = CARTESIAN_POINT ( 'NONE',  ( 102.3530718240336057, -2.986125964273158129, -4.150065902008639895 ) ) ;
#3984 = CARTESIAN_POINT ( 'NONE',  ( 23.03407491560847475, -17.39674082715732339, -1.686926596850272908 ) ) ;
#3985 = CARTESIAN_POINT ( 'NONE',  ( 13.41780342409107973, 19.07609913100965571, 4.629213727441584325 ) ) ;
#3986 = EDGE_CURVE ( 'NONE', #21393, #24740, #26220, .T. ) ;
#3987 = VERTEX_POINT ( 'NONE', #1384 ) ;
#3988 = APPROVAL_PERSON_ORGANIZATION ( #26013, #8983, #28826 ) ;
#3989 = CARTESIAN_POINT ( 'NONE',  ( 34.31843563627104032, 19.51744974835125035, 2.301584610165278377 ) ) ;
#3990 = FACE_OUTER_BOUND ( 'NONE', #3229, .T. ) ;
#3991 = CARTESIAN_POINT ( 'NONE',  ( 5.885541736258998569, -7.752826540560528557, 3.216848386728037745 ) ) ;
#3993 = EDGE_LOOP ( 'NONE', ( #29139, #16692, #29408, #32639 ) ) ;
#3992 = DIRECTION ( 'NONE',  ( 1.000000000000000000, 0.000000000000000000, -0.000000000000000000 ) ) ;
#3994 = CARTESIAN_POINT ( 'NONE',  ( 5.489321289187128805, -8.118169347437836691, -0.1038943573681802152 ) ) ;
#3995 = CARTESIAN_POINT ( 'NONE',  ( 19.10390797508231131, -2.015740111943978619, 0.07017451552781951707 ) ) ;
#3996 = CARTESIAN_POINT ( 'NONE',  ( 10.00000000000000000, -4.116875700062100130, 2.376879293651050329 ) ) ;
#3997 = CARTESIAN_POINT ( 'NONE',  ( 5.377543748152549874, -2.741043480754977946, 7.530955069117504230 ) ) ;
#3998 = CARTESIAN_POINT ( 'NONE',  ( 0.7212197595562506169, 8.936767016196059288, 0.5238431420062442667 ) ) ;
#3999 = LINE ( 'NONE', #16676, #11290 ) ;
#4000 = CARTESIAN_POINT ( 'NONE',  ( 0.000000000000000000, 0.6700234925292696264, 8.473551116235677583 ) ) ;
#4001 = EDGE_LOOP ( 'NONE', ( #7404, #31991, #7042, #20900 ) ) ;
#4002 = DIRECTION ( 'NONE',  ( 0.000000000000000000, 0.000000000000000000, 1.000000000000000000 ) ) ;
#4003 = ORIENTED_EDGE ( 'NONE', *, *, #11041, .T. ) ;
#4004 = CARTESIAN_POINT ( 'NONE',  ( 25.09406982928240737, -17.52096209994179787, -1.402054309285089673 ) ) ;
#4005 = CARTESIAN_POINT ( 'NONE',  ( -59.01620623031298152, -4.767884042047559667, 5.493143919433970623 ) ) ;
#4006 = CARTESIAN_POINT ( 'NONE',  ( 48.02957825751260401, -5.434743900603434597, -5.695980980372493008 ) ) ;
#4007 = FACE_OUTER_BOUND ( 'NONE', #21164, .T. ) ;
#4008 = CARTESIAN_POINT ( 'NONE',  ( 0.5032040568799869273, -5.109302080992267570, -8.283195248923467702 ) ) ;
#4009 = VERTEX_POINT ( 'NONE', #11559 ) ;
#4010 = CARTESIAN_POINT ( 'NONE',  ( 107.9195515681658435, 17.73019131299352935, -3.358191939550565497 ) ) ;
#4011 = EDGE_CURVE ( 'NONE', #19054, #32515, #12331, .T. ) ;
#4012 = B_SPLINE_CURVE_WITH_KNOTS ( 'NONE', 3,
 ( #14682, #1840, #2331, #24882 ),
 .UNSPECIFIED., .F., .F.,
 ( 4, 4 ),
 ( 0.000000000000000000, 0.0003584394985563508270 ),
 .UNSPECIFIED. ) ;
#4013 = ORIENTED_EDGE ( 'NONE', *, *, #11774, .T. ) ;
#4014 = APPROVAL_DATE_TIME ( #8991, #12272 ) ;
#4015 = DIRECTION ( 'NONE',  ( 0.000000000000000000, 1.000000000000000000, 0.000000000000000000 ) ) ;
#4016 = CARTESIAN_POINT ( 'NONE',  ( 7.161332922825494940, -6.537789733078093413, -0.9999999999999997780 ) ) ;
#4017 = ORIENTED_EDGE ( 'NONE', *, *, #22195, .F. ) ;
#4018 = DIRECTION ( 'NONE',  ( -0.03487826274237468965, -0.9987827659587182882, -0.03487826274237469659 ) ) ;
#4019 = VERTEX_POINT ( 'NONE', #32469 ) ;
#4020 = ORIENTED_EDGE ( 'NONE', *, *, #6524, .F. ) ;
#4021 = CARTESIAN_POINT ( 'NONE',  ( 10.55147673363119054, 4.116875700062082366, 2.376879293651078751 ) ) ;
#4022 = FACE_OUTER_BOUND ( 'NONE', #21715, .T. ) ;
#4023 = CARTESIAN_POINT ( 'NONE',  ( 23.67250000000000298, -1.291182301015472378, -2.378061970571982098 ) ) ;
#4024 = CARTESIAN_POINT ( 'NONE',  ( 5.543719668239277532, -12.78094047433792468, -1.499999999999999112 ) ) ;
#4026 = VERTEX_POINT ( 'NONE', #22106 ) ;
#4025 = DIRECTION ( 'NONE',  ( 4.917867153433032309E-17, 0.5735764363510496011, -0.8191520442889893561 ) ) ;
#4027 = CARTESIAN_POINT ( 'NONE',  ( -6.637550801365594388, -1.088641768524163389, -3.675193018007246071 ) ) ;
#4028 = DIRECTION ( 'NONE',  ( 6.062761635205589313E-17, 0.7071067811865484609, 0.7071067811865465735 ) ) ;
#4029 = CARTESIAN_POINT ( 'NONE',  ( 2.274274201625309910, -10.90201369670500853, -1.464956435139685098 ) ) ;
#4030 = FACE_OUTER_BOUND ( 'NONE', #7408, .T. ) ;
#4031 = ORIENTED_EDGE ( 'NONE', *, *, #13751, .F. ) ;
#4033 = VERTEX_POINT ( 'NONE', #6364 ) ;
#4032 = CARTESIAN_POINT ( 'NONE',  ( 13.17780055412413454, 21.79273496866543169, 1.386556541278284094 ) ) ;
#4034 = DIRECTION ( 'NONE',  ( 0.000000000000000000, -0.9659258262890701996, 0.2588190451025139671 ) ) ;
#4035 = DIRECTION ( 'NONE',  ( -1.000000000000000000, -0.000000000000000000, -0.000000000000000000 ) ) ;
#4036 = EDGE_CURVE ( 'NONE', #6686, #27584, #15493, .T. ) ;
#4037 = CARTESIAN_POINT ( 'NONE',  ( -17.64511778006428599, 14.89308641508515585, 1.500000000000212719 ) ) ;
#4038 = LINE ( 'NONE', #9692, #23565 ) ;
#4039 = CARTESIAN_POINT ( 'NONE',  ( 10.00000000000000000, 4.884328206559851004, -1.115095498423258391 ) ) ;
#4040 = FACE_OUTER_BOUND ( 'NONE', #954, .T. ) ;
#4041 = EDGE_CURVE ( 'NONE', #32002, #4375, #5389, .T. ) ;
#4042 = CARTESIAN_POINT ( 'NONE',  ( 18.99190826319515324, -3.267672110760487136, 1.529339877371808987 ) ) ;
#4043 = CARTESIAN_POINT ( 'NONE',  ( 107.4811544939906867, -15.87715700148073239, 1.499966567242846383 ) ) ;
#4044 = EDGE_LOOP ( 'NONE', ( #4344, #779, #17512, #15466 ) ) ;
#4045 = CARTESIAN_POINT ( 'NONE',  ( -34.48223484310472031, 0.5000000000000000000, 3.000000000000004441 ) ) ;
#4046 = EDGE_LOOP ( 'NONE', ( #19969, #22333, #3598, #30642 ) ) ;
#4047 = LINE ( 'NONE', #18934, #11332 ) ;
#4048 = ADVANCED_FACE ( 'NONE', ( #4553 ), #29449, .F. ) ;
#4049 = DIRECTION ( 'NONE',  ( -0.6916610887771488247, 0.000000000000000000, -0.7222222222222250965 ) ) ;
#4051 = LINE ( 'NONE', #11710, #24078 ) ;
#4050 = CARTESIAN_POINT ( 'NONE',  ( 5.885541615502094537, -1.821712961073290726, -8.193643496140870397 ) ) ;
#4052 = EDGE_LOOP ( 'NONE', ( #15808, #6055, #10166, #4353, #14565, #15838 ) ) ;
#4053 = DIRECTION ( 'NONE',  ( 1.000000000000000000, -0.000000000000000000, -0.000000000000000000 ) ) ;
#4054 = EDGE_LOOP ( 'NONE', ( #29370, #26954, #19470, #20740 ) ) ;
#4055 =( BOUNDED_SURFACE ( )  B_SPLINE_SURFACE ( 3, 2, ( 
 ( #1410, #6580, #13421 ),
 ( #23641, #764, #10946 ),
 ( #21147, #31347, #18617 ),
 ( #28812, #5907, #16100 ) ),
 .UNSPECIFIED., .F., .F., .F. ) 
 B_SPLINE_SURFACE_WITH_KNOTS ( ( 4, 4 ),
 ( 3, 3 ),
 ( 0.000000000000000000, 0.003454001599076465465 ),
 ( 0.000000000000000000, 1.000000000000000000 ),
 .UNSPECIFIED. ) 
 GEOMETRIC_REPRESENTATION_ITEM ( )  RATIONAL_B_SPLINE_SURFACE ( (
 ( 1.000000000000000000, 0.7097644798780626818, 1.000000000000000000),
 ( 1.000000000000000000, 0.7097691176663369905, 1.000000000000000000),
 ( 1.000000000000000000, 0.7097737773069662248, 1.000000000000000000),
 ( 1.000000000000000000, 0.7097784590644244940, 1.000000000000000000) ) ) 
 REPRESENTATION_ITEM ( '' )  SURFACE ( )  );
#4056 = DIRECTION ( 'NONE',  ( -0.9993908270190957621, 0.03489949670250105246, 0.000000000000000000 ) ) ;
#4058 = VERTEX_POINT ( 'NONE', #14065 ) ;
#4057 = CARTESIAN_POINT ( 'NONE',  ( 54.94550075121934185, -5.360342395864071463, -3.995006645025575232 ) ) ;
#4059 = ORIENTED_EDGE ( 'NONE', *, *, #29651, .T. ) ;
#4060 = EDGE_CURVE ( 'NONE', #24044, #21075, #1137, .T. ) ;
#4061 = DIRECTION ( 'NONE',  ( -0.1437473352845080599, 0.000000000000000000, 0.9896144216807893912 ) ) ;
#4062 = CARTESIAN_POINT ( 'NONE',  ( -23.54713438637982748, 8.275374457817619600, 8.600000000000004974 ) ) ;
#4064 = ORIENTED_EDGE ( 'NONE', *, *, #11126, .F. ) ;
#4063 = CARTESIAN_POINT ( 'NONE',  ( -30.51827900900859447, 4.402097243136374516, 5.049999999999999822 ) ) ;
#4065 = CARTESIAN_POINT ( 'NONE',  ( 11.83739209453320740, 5.126178544244889501, -1.500000000000000000 ) ) ;
#4066 = PLANE ( 'NONE',  #13309 ) ;
#4067 = CARTESIAN_POINT ( 'NONE',  ( 108.1013391355022861, -19.52862045784693024, -2.195867232700793981 ) ) ;
#4068 = CARTESIAN_POINT ( 'NONE',  ( 10.90710808013608002, -12.60204455941997992, -1.000000000000000000 ) ) ;
#4070 = VERTEX_POINT ( 'NONE', #14726 ) ;
#4069 = CARTESIAN_POINT ( 'NONE',  ( 108.0210557654949213, -18.37255990186116250, -5.108931023128011617 ) ) ;
#4071 = CARTESIAN_POINT ( 'NONE',  ( -4.700050802731189137, -2.853674364686378695, -1.549418761218566809 ) ) ;
#4072 = EDGE_CURVE ( 'NONE', #2577, #30211, #32136, .T. ) ;
#4073 = B_SPLINE_CURVE_WITH_KNOTS ( 'NONE', 3,
 ( #22961, #5257, #25642, #2757, #26318, #21621, #9048, #3429, #16578, #26790 ),
 .UNSPECIFIED., .F., .F.,
 ( 4, 2, 2, 2, 4 ),
 ( 2.740849916261192663E-07, 0.0005478761651001754851, 0.001095478245208724843, 0.001643080325317274092, 0.002190682405425823341 ),
 .UNSPECIFIED. ) ;
#4074 = LINE ( 'NONE', #31671, #26259 ) ;
#4075 = DIRECTION ( 'NONE',  ( -1.000000000000000000, -0.000000000000000000, -0.000000000000000000 ) ) ;
#4076 = CARTESIAN_POINT ( 'NONE',  ( 24.39659513448100725, -17.41072360183587264, -1.416990234759457401 ) ) ;
#4077 = DIRECTION ( 'NONE',  ( 1.000000000000000000, 0.000000000000000000, 0.000000000000000000 ) ) ;
#4078 = ORIENTED_EDGE ( 'NONE', *, *, #29184, .T. ) ;
#4079 = CARTESIAN_POINT ( 'NONE',  ( -6.500050800000000351, -0.3135853898029607456, 2.983565686104819648 ) ) ;
#4080 = FACE_BOUND ( 'NONE', #17194, .T. ) ;
#4081 = DIRECTION ( 'NONE',  ( 0.000000000000000000, -0.9205048534524477022, 0.3907311284892561742 ) ) ;
#4082 = ORIENTED_EDGE ( 'NONE', *, *, #32280, .T. ) ;
#4083 = CARTESIAN_POINT ( 'NONE',  ( 2.589202944057205968, -6.846250362091585551, 7.715757980413542327 ) ) ;
#4084 = EDGE_CURVE ( 'NONE', #9305, #29668, #1658, .T. ) ;
#4085 = CARTESIAN_POINT ( 'NONE',  ( 79.17573959169237696, 22.98125563777605151, -4.612695725900423760 ) ) ;
#4086 = EDGE_LOOP ( 'NONE', ( #19106, #17914, #27843, #25051, #22770 ) ) ;
#4087 = CARTESIAN_POINT ( 'NONE',  ( 8.778793719788994920, -1.107495284042741668, 0.9999999999999997780 ) ) ;
#4088 = EDGE_CURVE ( 'NONE', #4337, #23656, #26727, .T. ) ;
#4089 = ORIENTED_EDGE ( 'NONE', *, *, #13721, .T. ) ;
#4090 = ORIENTED_EDGE ( 'NONE', *, *, #21198, .T. ) ;
#4091 = CONTEXT_DEPENDENT_SHAPE_REPRESENTATION ( #23367, #18053 ) ;
#4093 = VERTEX_POINT ( 'NONE', #24924 ) ;
#4092 = DIRECTION ( 'NONE',  ( -1.000000000000000000, -0.000000000000000000, 0.000000000000000000 ) ) ;
#4094 = EDGE_LOOP ( 'NONE', ( #32039, #9240, #30605, #31332 ) ) ;
#4095 = LINE ( 'NONE', #9420, #18216 ) ;
#4096 = ADVANCED_FACE ( 'NONE', ( #2037 ), #12209, .T. ) ;
#4097 = ORIENTED_EDGE ( 'NONE', *, *, #13527, .F. ) ;
#4098 = DIRECTION ( 'NONE',  ( 0.000000000000000000, 1.000000000000000000, 0.000000000000000000 ) ) ;
#4099 = DIRECTION ( 'NONE',  ( -1.000000000000000000, -0.000000000000000000, -0.000000000000000000 ) ) ;
#4101 = VERTEX_POINT ( 'NONE', #4859 ) ;
#4100 = CARTESIAN_POINT ( 'NONE',  ( 41.34499449509760893, -4.297820755681335925, -1.873789611272560718 ) ) ;
#4102 = CARTESIAN_POINT ( 'NONE',  ( 22.45654965262580660, -21.89488356522464230, 1.207177750837651775 ) ) ;
#4103 = CARTESIAN_POINT ( 'NONE',  ( 1.052005621165114757, 19.51744974835124680, -7.242429449796464525 ) ) ;
#4104 = CARTESIAN_POINT ( 'NONE',  ( 7.064632879756603145, 0.8180878109961848832, 8.711672189281427947 ) ) ;
#4105 = CARTESIAN_POINT ( 'NONE',  ( 5.377543748152549874, 5.151476664237477188, 6.139290821770273077 ) ) ;
#4106 = EDGE_CURVE ( 'NONE', #28120, #29752, #2187, .T. ) ;
#4107 = CC_DESIGN_PERSON_AND_ORGANIZATION_ASSIGNMENT ( #19124, #21642, ( #32825 ) ) ;
#4108 = DIRECTION ( 'NONE',  ( 0.000000000000000000, 0.000000000000000000, 1.000000000000000000 ) ) ;
#4109 = CARTESIAN_POINT ( 'NONE',  ( -10.00000000000000000, 0.000000000000000000, 0.000000000000000000 ) ) ;
#4110 = DIRECTION ( 'NONE',  ( -0.08910563629484158366, -0.9960221812693186294, 0.000000000000000000 ) ) ;
#4111 = DIRECTION ( 'NONE',  ( -5.361488761196502513E-16, 1.000000000000000000, 0.000000000000000000 ) ) ;
#4112 = CARTESIAN_POINT ( 'NONE',  ( 3.499999999999999556, 0.000000000000000000, 0.000000000000000000 ) ) ;
#4113 = CARTESIAN_POINT ( 'NONE',  ( 23.79750000273118715, -2.594547506269383685, -0.7685399846772043020 ) ) ;
#4114 = LINE ( 'NONE', #16635, #15580 ) ;
#4115 = CARTESIAN_POINT ( 'NONE',  ( -5.500050802731188071, -2.853674364686378695, -1.549418761218566809 ) ) ;
#4116 = EDGE_LOOP ( 'NONE', ( #32107, #16025 ) ) ;
#4117 = CARTESIAN_POINT ( 'NONE',  ( -7.887550801365593500, 2.228590825266444142, 2.752080473201636845 ) ) ;
#4118 = CARTESIAN_POINT ( 'NONE',  ( 107.3033141393571981, 17.10611366274323331, -3.000076723692274960 ) ) ;
#4119 = EDGE_CURVE ( 'NONE', #32242, #7729, #2749, .T. ) ;
#4120 = CARTESIAN_POINT ( 'NONE',  ( -5.650050802731187538, -2.331437884370912705, 1.887961173149512062 ) ) ;
#4121 = CARTESIAN_POINT ( 'NONE',  ( 8.305304941488214965, -2.146676032724874617, 1.500000000000000222 ) ) ;
#4122 = ORIENTED_EDGE ( 'NONE', *, *, #15321, .F. ) ;
#4123 = DIRECTION ( 'NONE',  ( 0.000000000000000000, 0.000000000000000000, 1.000000000000000000 ) ) ;
#4124 = VERTEX_POINT ( 'NONE', #30288 ) ;
#4125 = CARTESIAN_POINT ( 'NONE',  ( 0.5438373813056243122, -6.199957864112706218, 1.500000000000000444 ) ) ;
#4126 = COORDINATED_UNIVERSAL_TIME_OFFSET ( 0, 0, .AHEAD. ) ;
#4127 = CARTESIAN_POINT ( 'NONE',  ( 56.97280603064898941, -277.2763395528616002, -4.621439243524461560 ) ) ;
#4128 = ORIENTED_EDGE ( 'NONE', *, *, #29590, .F. ) ;
#4129 = CARTESIAN_POINT ( 'NONE',  ( 14.44927029820895292, -20.94157174084352491, 1.499999999999999556 ) ) ;
#4130 = CARTESIAN_POINT ( 'NONE',  ( 10.52034268205830614, -3.641590349731950393, 3.055657119358789142 ) ) ;
#4131 = CARTESIAN_POINT ( 'NONE',  ( -2.620518043835247113, -0.1971982189170117805, 1.631770423870609221 ) ) ;
#4132 = CARTESIAN_POINT ( 'NONE',  ( 24.25321317638936947, -17.33169478063224389, -1.345077977219350185 ) ) ;
#4133 = CARTESIAN_POINT ( 'NONE',  ( 9.149098621172166546, 18.06225657836807841, 4.629213727441584325 ) ) ;
#4134 = EDGE_LOOP ( 'NONE', ( #7495, #6868, #25711, #27032 ) ) ;
#4135 = CARTESIAN_POINT ( 'NONE',  ( 0.7632845268398871230, -7.360373001730951437, 4.729683950898845524 ) ) ;
#4136 = DIRECTION ( 'NONE',  ( 1.000000000000000000, -8.574039729943018344E-17, -0.000000000000000000 ) ) ;
#4137 = CARTESIAN_POINT ( 'NONE',  ( 2.437082530871043762, -5.244446742619423674, -9.289394354155845690 ) ) ;
#4138 = EDGE_CURVE ( 'NONE', #20071, #115, #7523, .T. ) ;
#4140 = ORIENTED_EDGE ( 'NONE', *, *, #10311, .F. ) ;
#4139 = DIRECTION ( 'NONE',  ( 0.000000000000000000, 0.000000000000000000, -1.000000000000000000 ) ) ;
#4141 = CARTESIAN_POINT ( 'NONE',  ( 7.249760686538667009, 5.151476664237558900, -6.139290821770204687 ) ) ;
#4142 = CARTESIAN_POINT ( 'NONE',  ( 69.09268213438591033, -2.232183665269761086, -0.07017451552781628354 ) ) ;
#4143 = CARTESIAN_POINT ( 'NONE',  ( -1.082681991931091492, 0.000000000000000000, 4.629213727441584325 ) ) ;
#4144 = CARTESIAN_POINT ( 'NONE',  ( 2.274274201620947622, 4.762163868927166810, 9.915734732518528105 ) ) ;
#4145 = CARTESIAN_POINT ( 'NONE',  ( 3.063284526843245370, -8.152713396074034335, 3.174628368989241611 ) ) ;
#4146 = CARTESIAN_POINT ( 'NONE',  ( -31.69719015456885103, -21.93932300455405482, 1.000000000000000444 ) ) ;
#4147 = DIRECTION ( 'NONE',  ( -1.000000000000000000, -0.000000000000000000, -0.000000000000000000 ) ) ;
#4148 = DIRECTION ( 'NONE',  ( -1.000000000000000000, 0.000000000000000000, 0.000000000000000000 ) ) ;
#4149 = CARTESIAN_POINT ( 'NONE',  ( -3.830085165118302378E-16, -4.467071865485461757, -1.625881193364742572 ) ) ;
#4150 = ORIENTED_EDGE ( 'NONE', *, *, #30056, .T. ) ;
#4151 = CARTESIAN_POINT ( 'NONE',  ( -2.900050802731187538, 1.549418761218566143, -2.853674364686379583 ) ) ;
#4152 = VERTEX_POINT ( 'NONE', #30139 ) ;
#4153 = ADVANCED_FACE ( 'NONE', ( #32809 ), #32317, .T. ) ;
#4154 = PLANE ( 'NONE',  #17241 ) ;
#4155 = FACE_OUTER_BOUND ( 'NONE', #3966, .T. ) ;
#4156 = ADVANCED_FACE ( 'NONE', ( #12552 ), #27258, .T. ) ;
#4157 = DIRECTION ( 'NONE',  ( 0.000000000000000000, 0.000000000000000000, 1.000000000000000000 ) ) ;
#4158 = CARTESIAN_POINT ( 'NONE',  ( -5.312942406915326821, -3.366872799099910998E-15, -3.000000000000000000 ) ) ;
#4159 = FACE_OUTER_BOUND ( 'NONE', #13084, .T. ) ;
#4160 = ORIENTED_EDGE ( 'NONE', *, *, #18307, .T. ) ;
#4161 = CYLINDRICAL_SURFACE ( 'NONE', #18297, 6.248999999999999666 ) ;
#4162 = VERTEX_POINT ( 'NONE', #22755 ) ;
#4163 = APPROVAL_ROLE ( '' ) ;
#4164 = CARTESIAN_POINT ( 'NONE',  ( 69.07033661638675426, -6.114099455435076713, 3.997239029219557871 ) ) ;
#4165 = LINE ( 'NONE', #14331, #13338 ) ;
#4166 = CARTESIAN_POINT ( 'NONE',  ( 6.356382477965132338, 6.209963745178092687, -5.959271875177088340 ) ) ;
#4167 = ORIENTED_EDGE ( 'NONE', *, *, #32280, .F. ) ;
#4168 = EDGE_LOOP ( 'NONE', ( #11446, #28406 ) ) ;
#4169 = CARTESIAN_POINT ( 'NONE',  ( 3.020080146450413228, 8.942241244976921521, -0.5244911560323413102 ) ) ;
#4170 = CARTESIAN_POINT ( 'NONE',  ( 24.60999999999999943, -1.942864903642428587, -1.573300977624592756 ) ) ;
#4171 = CARTESIAN_POINT ( 'NONE',  ( 2.123790277358594381, -10.79657358825966540, -1.499999999999929834 ) ) ;
#4173 = EDGE_LOOP ( 'NONE', ( #25861, #16720, #14284, #32183, #6832, #15793, #30963, #10003, #21188, #31609, #14023, #6192, #5159, #7832, #13280, #32765 ) ) ;
#4172 = CARTESIAN_POINT ( 'NONE',  ( 9.513442983150083521, 1.350987762931694647, -1.500000000000000444 ) ) ;
#4174 = CARTESIAN_POINT ( 'NONE',  ( -2.537550801365592967, 1.828967928396027176, -3.368539882008727115 ) ) ;
#4175 = CARTESIAN_POINT ( 'NONE',  ( 4.749760686538667009, -2.789499415801756586E-14, 8.014274990069656823 ) ) ;
#4176 = DIRECTION ( 'NONE',  ( 0.9842544651762055175, -0.1767573132311700268, 0.000000000000000000 ) ) ;
#4177 = DIRECTION ( 'NONE',  ( 0.000000000000000000, 0.000000000000000000, 1.000000000000000000 ) ) ;
#4178 = VERTEX_POINT ( 'NONE', #17726 ) ;
#4180 = ORIENTED_EDGE ( 'NONE', *, *, #15880, .T. ) ;
#4179 = CARTESIAN_POINT ( 'NONE',  ( 13.62547635268498780, 21.94000000000002970, 1.050000000000000044 ) ) ;
#4181 = DIRECTION ( 'NONE',  ( 1.000000000000000000, -0.000000000000000000, -0.000000000000000000 ) ) ;
#4182 = CARTESIAN_POINT ( 'NONE',  ( 3.499999999999999556, 4.137773741518454784, -5.705158055754753654 ) ) ;
#4183 = EDGE_CURVE ( 'NONE', #7539, #635, #32467, .T. ) ;
#4184 = EDGE_CURVE ( 'NONE', #32821, #5447, #20351, .T. ) ;
#4185 = CARTESIAN_POINT ( 'NONE',  ( 25.23500000136559507, -3.156283516753370488, -0.9349337715887220401 ) ) ;
#4186 = ADVANCED_FACE ( 'NONE', ( #4374 ), #19269, .T. ) ;
#4187 = CARTESIAN_POINT ( 'NONE',  ( 3.063284526843251587, -3.174628368989204308, -8.152713396074016572 ) ) ;
#4188 = DIRECTION ( 'NONE',  ( 1.000000000000000000, 0.000000000000000000, 0.000000000000000000 ) ) ;
#4189 = DIRECTION ( 'NONE',  ( 0.000000000000000000, 0.08715574274764853469, 0.9961946980917464334 ) ) ;
#4190 = CARTESIAN_POINT ( 'NONE',  ( 35.33570769238654918, -4.203675997508045548, 1.873789188777248871 ) ) ;
#4191 = CARTESIAN_POINT ( 'NONE',  ( -3.837550801365593234, 1.088641768524161613, 3.675193018007247403 ) ) ;
#4192 = ORIENTED_EDGE ( 'NONE', *, *, #187, .F. ) ;
#4193 = CARTESIAN_POINT ( 'NONE',  ( 29.18953645666586638, -9.308308156628569918, -0.07017451552783579571 ) ) ;
#4194 = ORIENTED_EDGE ( 'NONE', *, *, #10389, .F. ) ;
#4195 = CARTESIAN_POINT ( 'NONE',  ( -7.000050800000000351, 0.000000000000000000, -6.000000000000000888 ) ) ;
#4196 = DIRECTION ( 'NONE',  ( -1.000000000000000000, 0.000000000000000000, 0.000000000000000000 ) ) ;
#4197 = DIRECTION ( 'NONE',  ( 1.000000000000000000, -0.000000000000000000, -0.000000000000000000 ) ) ;
#4198 = ORIENTED_EDGE ( 'NONE', *, *, #12253, .F. ) ;
#4199 = CARTESIAN_POINT ( 'NONE',  ( -53.55623634834322644, 5.485000000000006537, 1.500000000000000888 ) ) ;
#4200 = ORIENTED_EDGE ( 'NONE', *, *, #32445, .T. ) ;
#4202 = ORIENTED_EDGE ( 'NONE', *, *, #20906, .F. ) ;
#4201 = CARTESIAN_POINT ( 'NONE',  ( 54.94547365672024597, -5.359363431720396420, -3.993434333307572359 ) ) ;
#4203 = VERTEX_POINT ( 'NONE', #29785 ) ;
#4204 = CARTESIAN_POINT ( 'NONE',  ( 17.39502519978889694, -21.04076415203780925, 1.751145182513948351 ) ) ;
#4205 = B_SPLINE_CURVE_WITH_KNOTS ( 'NONE', 3,
 ( #10271, #20491, #4934, #2263, #17800, #30704, #17968, #7777, #27503, #7267 ),
 .UNSPECIFIED., .F., .F.,
 ( 4, 2, 2, 2, 4 ),
 ( 1.968338519010778477E-07, 0.0005467930078056964724, 0.001093389181759491739, 0.001639985355713287222, 0.002186581529667082704 ),
 .UNSPECIFIED. ) ;
#4206 = CARTESIAN_POINT ( 'NONE',  ( 41.44907012427937332, -8.741883605783066002, -2.713652344655542059 ) ) ;
#4208 = VERTEX_POINT ( 'NONE', #22258 ) ;
#4207 = CARTESIAN_POINT ( 'NONE',  ( -4.176564909271631265, -3.225750814637073915, -1.500000000000000000 ) ) ;
#4209 = CARTESIAN_POINT ( 'NONE',  ( 3.499999999999999556, -6.700937042937042065, 0.8165525598867410251 ) ) ;
#4210 = FACE_OUTER_BOUND ( 'NONE', #27037, .T. ) ;
#4211 = CARTESIAN_POINT ( 'NONE',  ( -3.135269660805080516, -0.4999999999999986122, 1.499999999999999112 ) ) ;
#4212 = CARTESIAN_POINT ( 'NONE',  ( 6.734961451239279029, -5.723322302742661627, -1.500000000000000000 ) ) ;
#4214 = ORIENTED_EDGE ( 'NONE', *, *, #9124, .T. ) ;
#4213 = CARTESIAN_POINT ( 'NONE',  ( 107.4706864324941762, -17.65962134356383473, -4.956537357604676508 ) ) ;
#4215 = FACE_OUTER_BOUND ( 'NONE', #9448, .T. ) ;
#4216 = ADVANCED_FACE ( 'NONE', ( #24921 ), #6861, .T. ) ;
#4217 = CARTESIAN_POINT ( 'NONE',  ( 2.037945749704362236E-16, 2.376879293651122271, -4.116875700062057497 ) ) ;
#4218 = CARTESIAN_POINT ( 'NONE',  ( 25.04750000136559507, -3.024605502323851169, 0.3178988483021052969 ) ) ;
#4219 = EDGE_CURVE ( 'NONE', #16746, #19457, #19742, .T. ) ;
#4220 = DIRECTION ( 'NONE',  ( -0.9896144216807899463, -8.678901113238557421E-19, -0.1437473352845038133 ) ) ;
#4221 = CARTESIAN_POINT ( 'NONE',  ( -0.9801757370192284435, 20.00000000000000000, 6.747923662139668544 ) ) ;
#4222 = ORIENTED_EDGE ( 'NONE', *, *, #29987, .F. ) ;
#4223 = CARTESIAN_POINT ( 'NONE',  ( 10.56183597391177464, -1.750323540954535505E-14, 4.753758587302147731 ) ) ;
#4224 = ADVANCED_FACE ( 'NONE', ( #14560 ), #12062, .T. ) ;
#4225 = PLANE ( 'NONE',  #1198 ) ;
#4226 = FACE_OUTER_BOUND ( 'NONE', #5838, .T. ) ;
#4227 = ORIENTED_EDGE ( 'NONE', *, *, #8514, .F. ) ;
#4228 =( BOUNDED_CURVE ( )  B_SPLINE_CURVE ( 2, ( #3869, #2024, #24562, #4362, #22091, #12196, #16733, #11882, #19423, #9514, #1686 ),
 .UNSPECIFIED., .F., .F. ) 
 B_SPLINE_CURVE_WITH_KNOTS ( ( 3, 2, 2, 2, 2, 3 ),
 ( 0.1853822619934377414, 0.1875000000000000000, 0.2031250000000000000, 0.2187500000000000000, 0.2343750000000000000, 0.2478822619934377414 ),
 .UNSPECIFIED. ) 
 CURVE ( )  GEOMETRIC_REPRESENTATION_ITEM ( )  RATIONAL_B_SPLINE_CURVE ( ( 0.9821626249036861100, 0.9896829947469993893, 1.000000000000000000, 0.9238795325112867385, 1.000000000000000000, 0.9238795325112867385, 1.000000000000000000, 0.9238795325112867385, 1.000000000000000000, 0.9341965377642873491, 0.9821626249036861100 ) ) 
 REPRESENTATION_ITEM ( '' )  );
#4229 = CARTESIAN_POINT ( 'NONE',  ( -61.68687437218811453, -10.96999999999998643, 2.028141679950118625 ) ) ;
#4230 = EDGE_CURVE ( 'NONE', #31957, #24212, #30443, .T. ) ;
#4231 = CARTESIAN_POINT ( 'NONE',  ( 3.295700863922525148, -0.1006852655820348191, -1.307585114970547746 ) ) ;
#4232 = ORIENTED_EDGE ( 'NONE', *, *, #33046, .F. ) ;
#4233 = CARTESIAN_POINT ( 'NONE',  ( 8.265818664828525897, -2.240834465000072662, 1.000000000000000000 ) ) ;
#4234 = ORIENTED_EDGE ( 'NONE', *, *, #21044, .F. ) ;
#4235 = VERTEX_POINT ( 'NONE', #4703 ) ;
#4236 = CARTESIAN_POINT ( 'NONE',  ( 3.499999999999999556, 0.000000000000000000, 0.000000000000000000 ) ) ;
#4237 = DATE_TIME_ROLE ( 'classification_date' ) ;
#4239 = ORIENTED_EDGE ( 'NONE', *, *, #5401, .F. ) ;
#4238 = CARTESIAN_POINT ( 'NONE',  ( 2.592584839945471842, -5.238191131136688661, 8.898511132913965227 ) ) ;
#4240 = EDGE_CURVE ( 'NONE', #29734, #12461, #18299, .T. ) ;
#4241 = ORIENTED_EDGE ( 'NONE', *, *, #19595, .T. ) ;
#4242 = CARTESIAN_POINT ( 'NONE',  ( 21.67250000136559507, 2.363507492473148286, 1.913930629741525058 ) ) ;
#4244 = ORIENTED_EDGE ( 'NONE', *, *, #17005, .T. ) ;
#4243 = AXIS2_PLACEMENT_3D ( 'NONE', #10289, #28024, #23475 ) ;
#4245 = DIRECTION ( 'NONE',  ( 0.000000000000000000, -0.000000000000000000, 1.000000000000000000 ) ) ;
#4246 = CARTESIAN_POINT ( 'NONE',  ( 5.612974259723586989, -7.650268724902040240, -2.996912441296252005 ) ) ;
#4248 = VERTEX_POINT ( 'NONE', #7713 ) ;
#4247 = CARTESIAN_POINT ( 'NONE',  ( -28.64263641446437347, 5.485000000000014531, 1.500000000000000000 ) ) ;
#4249 = DIRECTION ( 'NONE',  ( -1.000000000000000000, -0.000000000000000000, -0.000000000000000000 ) ) ;
#4250 = VECTOR ( 'NONE', #25334, 1000.000000000000000 ) ;
#4251 = CARTESIAN_POINT ( 'NONE',  ( 2.857987896741710276, 2.305585824582336407, -9.278099925253918911 ) ) ;
#4252 = EDGE_CURVE ( 'NONE', #31255, #1418, #11788, .T. ) ;
#4253 = CARTESIAN_POINT ( 'NONE',  ( 5.377543748152548986, 1.391664247347228045, 7.892520144992438702 ) ) ;
#4254 = CARTESIAN_POINT ( 'NONE',  ( 22.98500000136559507, -2.892927487894331406, 1.570731468192932301 ) ) ;
#4255 = CARTESIAN_POINT ( 'NONE',  ( -8.000050800000002127, 3.541248556864417196, 0.01107501445590582979 ) ) ;
#4256 = AXIS2_PLACEMENT_3D ( 'NONE', #16448, #9084, #11117 ) ;
#4257 = CARTESIAN_POINT ( 'NONE',  ( 17.49368528860006222, -18.49828807951654497, -5.485967528433937979 ) ) ;
#4258 = DIRECTION ( 'NONE',  ( 0.000000000000000000, 0.000000000000000000, 1.000000000000000000 ) ) ;
#4259 = DIRECTION ( 'NONE',  ( -1.000000000000000000, 0.000000000000000000, 0.000000000000000000 ) ) ;
#4260 = EDGE_CURVE ( 'NONE', #20898, #15360, #9636, .T. ) ;
#4261 = EDGE_CURVE ( 'NONE', #14918, #19163, #27480, .T. ) ;
#4262 = DIRECTION ( 'NONE',  ( 0.000000000000000000, 0.000000000000000000, 1.000000000000000000 ) ) ;
#4263 = FACE_OUTER_BOUND ( 'NONE', #2466, .T. ) ;
#4264 = CYLINDRICAL_SURFACE ( 'NONE', #25759, 2.499999999999997780 ) ;
#4265 = DIRECTION ( 'NONE',  ( -1.000000000000000000, 0.000000000000000000, 0.000000000000000000 ) ) ;
#4266 = EDGE_CURVE ( 'NONE', #7057, #19157, #20897, .T. ) ;
#4267 = CARTESIAN_POINT ( 'NONE',  ( -5.550050802731187893, -2.983565686104819648, -0.3135853898029605791 ) ) ;
#4268 = ORIENTED_EDGE ( 'NONE', *, *, #29875, .T. ) ;
#4269 = CARTESIAN_POINT ( 'NONE',  ( -2.750050800000000351, 3.113457007523260156, -0.9222479816126439855 ) ) ;
#4270 = AXIS2_PLACEMENT_3D ( 'NONE', #18114, #6958, #27371 ) ;
#4271 = AXIS2_PLACEMENT_3D ( 'NONE', #7634, #20175, #18328 ) ;
#4272 = CARTESIAN_POINT ( 'NONE',  ( 10.00000000000000178, 4.971152295393311604, -0.6226916219171535483 ) ) ;
#4273 = CARTESIAN_POINT ( 'NONE',  ( -4.157304906975410219, 1.062355717592091686, 3.000000000000001332 ) ) ;
#4274 = ORIENTED_EDGE ( 'NONE', *, *, #6708, .T. ) ;
#4275 = DIRECTION ( 'NONE',  ( -1.000000000000000000, 0.000000000000000000, 0.000000000000000000 ) ) ;
#4276 = CARTESIAN_POINT ( 'NONE',  ( 7.249760686538667009, -7.199384779417084879, -4.973063321323951236 ) ) ;
#4277 = EDGE_CURVE ( 'NONE', #30410, #32250, #10192, .T. ) ;
#4278 = B_SPLINE_CURVE_WITH_KNOTS ( 'NONE', 3,
 ( #23321, #23804, #11096, #21294, #28997, #6098, #16278, #26491 ),
 .UNSPECIFIED., .F., .F.,
 ( 4, 2, 2, 4 ),
 ( 2.024520226828571228E-07, 0.001261135997420231077, 0.001891602770119004849, 0.002522069542817778620 ),
 .UNSPECIFIED. ) ;
#4279 = VERTEX_POINT ( 'NONE', #5691 ) ;
#4280 = CARTESIAN_POINT ( 'NONE',  ( 9.054625866885391616, -14.53177083716424889, 1.499999999999929390 ) ) ;
#4281 = APPROVAL_STATUS ( 'not_yet_approved' ) ;
#4282 = CARTESIAN_POINT ( 'NONE',  ( 3.249999999999999556, 4.729683950898872169, 7.360373001730934561 ) ) ;
#4283 = VERTEX_POINT ( 'NONE', #20417 ) ;
#4284 = CARTESIAN_POINT ( 'NONE',  ( 18.65791233782715963, -7.001076235476726417, -2.184956778830003277 ) ) ;
#4285 = EDGE_CURVE ( 'NONE', #7137, #15697, #4332, .T. ) ;
#4286 = CARTESIAN_POINT ( 'NONE',  ( 9.909835366851556415, 1.133397303054362037, -1.050000000000000266 ) ) ;
#4287 = CARTESIAN_POINT ( 'NONE',  ( 102.4232908028701985, -3.999773562678796690, -3.993434327364950853 ) ) ;
#4288 = CARTESIAN_POINT ( 'NONE',  ( 6.038144853276843804, -1.911563584435252539, 8.256557579931657287 ) ) ;
#4289 = CARTESIAN_POINT ( 'NONE',  ( 3.499999999999999556, 6.704570150426983233, 2.172265885002680808 ) ) ;
#4290 = EDGE_LOOP ( 'NONE', ( #25318, #17320, #13618, #7211 ) ) ;
#4291 = VECTOR ( 'NONE', #5322, 1000.000000000000000 ) ;
#4292 = DIRECTION ( 'NONE',  ( -3.469446951953478110E-15, -1.087146173449926665E-32, 1.000000000000000000 ) ) ;
#4293 = EDGE_CURVE ( 'NONE', #1346, #29154, #16686, .T. ) ;
#4294 = DIRECTION ( 'NONE',  ( -7.770718973608971261E-17, -0.9063077870366493816, -0.4226182617407005515 ) ) ;
#4295 = CARTESIAN_POINT ( 'NONE',  ( 18.92729423629925378, -3.989927253179415878, -2.790733528450975331 ) ) ;
#4296 = CIRCLE ( 'NONE', #4270, 0.5000000000000003331 ) ;
#4298 = VERTEX_POINT ( 'NONE', #13194 ) ;
#4297 = CARTESIAN_POINT ( 'NONE',  ( 25.59647104375314441, 0.9427069350839755169, -2.712103814530933743 ) ) ;
#4299 = CARTESIAN_POINT ( 'NONE',  ( 5.612973690782940395, -8.213905076232780544, -0.1996300861631225554 ) ) ;
#4300 = VECTOR ( 'NONE', #26617, 1000.000000000000000 ) ;
#4301 = CARTESIAN_POINT ( 'NONE',  ( 47.98568197278775216, -2.821418575600922019, 0.07017451552781951707 ) ) ;
#4302 = CARTESIAN_POINT ( 'NONE',  ( -4.450050802731187360, 2.331437884370912705, -1.887961173149511618 ) ) ;
#4303 = FACE_OUTER_BOUND ( 'NONE', #9384, .T. ) ;
#4304 = DIRECTION ( 'NONE',  ( -1.000000000000000000, 0.000000000000000000, 0.000000000000000000 ) ) ;
#4305 = EDGE_CURVE ( 'NONE', #19445, #32003, #31565, .T. ) ;
#4306 = VECTOR ( 'NONE', #22189, 1000.000000000000000 ) ;
#4307 = ADVANCED_FACE ( 'NONE', ( #8209 ), #10871, .F. ) ;
#4308 = AXIS2_PLACEMENT_3D ( 'NONE', #8304, #29029, #3292 ) ;
#4309 = DIRECTION ( 'NONE',  ( 1.000000000000000000, -8.574039729943018344E-17, -0.000000000000000000 ) ) ;
#4310 =( BOUNDED_CURVE ( )  B_SPLINE_CURVE ( 2, ( #22550, #2336, #1532, #12516, #2500, #33074, #26947, #19246, #25216, #29445, #32926 ),
 .UNSPECIFIED., .F., .F. ) 
 B_SPLINE_CURVE_WITH_KNOTS ( ( 3, 2, 2, 2, 2, 3 ),
 ( 0.7478822619934377691, 0.7500000000000000000, 0.7656250000000000000, 0.7812500000000000000, 0.7968750000000000000, 0.8103822619934377691 ),
 .UNSPECIFIED. ) 
 CURVE ( )  GEOMETRIC_REPRESENTATION_ITEM ( )  RATIONAL_B_SPLINE_CURVE ( ( 0.9821626249036861100, 0.9896829947469995004, 1.000000000000000000, 0.9238795325112867385, 1.000000000000000000, 0.9238795325112867385, 1.000000000000000000, 0.9238795325112867385, 1.000000000000000000, 0.9341965377642872381, 0.9821626249036861100 ) ) 
 REPRESENTATION_ITEM ( '' )  );
#4311 = CARTESIAN_POINT ( 'NONE',  ( 3.063284526846072442, -8.461683424479964799, -2.223716399039827429 ) ) ;
#4312 = CARTESIAN_POINT ( 'NONE',  ( 24.48500000273118715, 0.2613211581691317065, 2.486304738420681559 ) ) ;
#4313 = CARTESIAN_POINT ( 'NONE',  ( -29.97923030674312983, 9.414801368908669588, 1.999766382938328313 ) ) ;
#4314 = VERTEX_POINT ( 'NONE', #2887 ) ;
#4315 = FACE_OUTER_BOUND ( 'NONE', #11760, .T. ) ;
#4316 = ORIENTED_EDGE ( 'NONE', *, *, #32615, .F. ) ;
#4317 = CARTESIAN_POINT ( 'NONE',  ( -7.504531657079157370, 2.975847129947406522, 0.3127741368606808403 ) ) ;
#4318 = CARTESIAN_POINT ( 'NONE',  ( 25.42250000136559507, -0.3178988483021076838, -3.024605502323848949 ) ) ;
#4319 = AXIS2_PLACEMENT_3D ( 'NONE', #17025, #27231, #11688 ) ;
#4320 = CARTESIAN_POINT ( 'NONE',  ( -23.35000000000000142, -10.96966150227469505, -11.50000000000000000 ) ) ;
#4321 = AXIS2_PLACEMENT_3D ( 'NONE', #18066, #20598, #28256 ) ;
#4322 = CARTESIAN_POINT ( 'NONE',  ( 109.4757865442224443, 20.73844717707612872, -1.106576248373506655 ) ) ;
#4323 = CARTESIAN_POINT ( 'NONE',  ( 41.35597062189852835, -8.086568374297849360, 1.873789609323120331 ) ) ;
#4324 = ORIENTED_EDGE ( 'NONE', *, *, #14019, .F. ) ;
#4325 = CARTESIAN_POINT ( 'NONE',  ( -1.394036994807634510E-16, -1.625881193364727917, 4.467071865485467086 ) ) ;
#4326 = AXIS2_PLACEMENT_3D ( 'NONE', #21017, #28544, #16452 ) ;
#4328 = ADVANCED_FACE ( 'NONE', ( #2690 ), #31090, .T. ) ;
#4327 = CIRCLE ( 'NONE', #13370, 10.99999999999999822 ) ;
#4329 = ORIENTED_EDGE ( 'NONE', *, *, #32340, .F. ) ;
#4330 = PERSON_AND_ORGANIZATION_ROLE ( 'design_owner' ) ;
#4331 = CARTESIAN_POINT ( 'NONE',  ( 18.75849706888935131, -5.876740812950394854, 3.997238537398870584 ) ) ;
#4332 = CIRCLE ( 'NONE', #27285, 5.000000000000002665 ) ;
#4333 = LINE ( 'NONE', #21568, #11230 ) ;
#4335 = CARTESIAN_POINT ( 'NONE',  ( 23.00111451137534502, -1.283275288181523244E-15, -2.499999999999998668 ) ) ;
#4334 = CARTESIAN_POINT ( 'NONE',  ( 0.000000000000000000, -27.93932300454937590, 11.00000000000000000 ) ) ;
#4336 = ORIENTED_EDGE ( 'NONE', *, *, #15816, .T. ) ;
#4337 = VERTEX_POINT ( 'NONE', #13051 ) ;
#4338 = CARTESIAN_POINT ( 'NONE',  ( -8.125050801365594211, 0.3135853898029611342, -2.983565686104819648 ) ) ;
#4339 = CARTESIAN_POINT ( 'NONE',  ( -2.512550801365593056, -1.088641768524163611, -3.675193018007245627 ) ) ;
#4340 = EDGE_CURVE ( 'NONE', #6237, #14980, #25756, .T. ) ;
#4341 = CARTESIAN_POINT ( 'NONE',  ( 23.48500000000000298, -2.486304738420683780, 0.2613211581691335383 ) ) ;
#4342 = CARTESIAN_POINT ( 'NONE',  ( 0.2309693770184315653, -6.520999745069206099, -1.500000000000070832 ) ) ;
#4344 = ORIENTED_EDGE ( 'NONE', *, *, #20308, .F. ) ;
#4343 = DIRECTION ( 'NONE',  ( -1.000000000000000000, 0.000000000000000000, 0.000000000000000000 ) ) ;
#4345 = CARTESIAN_POINT ( 'NONE',  ( -3.387550801365593056, 0.3701630799359330593, -3.521866450007987037 ) ) ;
#4346 = CARTESIAN_POINT ( 'NONE',  ( 21.32535692059155963, -21.82495604402122069, 1.318256435726650633 ) ) ;
#4347 = EDGE_CURVE ( 'NONE', #8185, #17721, #5948, .T. ) ;
#4348 = VECTOR ( 'NONE', #9938, 1000.000000000000000 ) ;
#4349 = CARTESIAN_POINT ( 'NONE',  ( -5.749676575031998027, 0.000000000000000000, 0.000000000000000000 ) ) ;
#4350 = CARTESIAN_POINT ( 'NONE',  ( 107.5951944727603404, -19.46454432636559417, -3.536284406027203175 ) ) ;
#4351 = ORIENTED_EDGE ( 'NONE', *, *, #9757, .F. ) ;
#4353 = ORIENTED_EDGE ( 'NONE', *, *, #3773, .T. ) ;
#4352 = CARTESIAN_POINT ( 'NONE',  ( 6.530491712438077023, -7.168846788212658971, -4.859093986587931013 ) ) ;
#4354 = CIRCLE ( 'NONE', #19836, 0.5000000000000004441 ) ;
#4355 = VECTOR ( 'NONE', #22703, 1000.000000000000000 ) ;
#4357 = AXIS2_PLACEMENT_3D ( 'NONE', #11728, #23792, #24282 ) ;
#4356 = DIRECTION ( 'NONE',  ( 0.000000000000000000, 0.000000000000000000, -1.000000000000000000 ) ) ;
#4358 = LINE ( 'NONE', #14537, #810 ) ;
#4359 = CIRCLE ( 'NONE', #8096, 8.749000000000002331 ) ;
#4360 = CARTESIAN_POINT ( 'NONE',  ( 25.04750000136559507, -1.913930629741527500, 2.363507492473149618 ) ) ;
#4361 = AXIS2_PLACEMENT_3D ( 'NONE', #23605, #8543, #11220 ) ;
#4362 = CARTESIAN_POINT ( 'NONE',  ( -6.500050802731188959, -1.549418761218565255, 2.853674364686380471 ) ) ;
#4363 = CARTESIAN_POINT ( 'NONE',  ( -2.454768102818410291, -12.18272399704959064, -1.743819976092190416 ) ) ;
#4364 = AXIS2_PLACEMENT_3D ( 'NONE', #2978, #13132, #10618 ) ;
#4365 = CARTESIAN_POINT ( 'NONE',  ( 24.92249999999999943, 2.378061970571979433, -1.291182301015470602 ) ) ;
#4366 = CARTESIAN_POINT ( 'NONE',  ( 54.91389575943538404, -4.233367447935240335, 2.184956776131665279 ) ) ;
#4367 = CARTESIAN_POINT ( 'NONE',  ( -2.437550801365593767, 3.675193018007247403, -1.088641768524161391 ) ) ;
#4368 = ORIENTED_EDGE ( 'NONE', *, *, #11514, .T. ) ;
#4369 = CARTESIAN_POINT ( 'NONE',  ( 101.6570814670602374, -1.960542089248300535, 2.484897212538878186 ) ) ;
#4370 = VERTEX_POINT ( 'NONE', #29092 ) ;
#4371 = CARTESIAN_POINT ( 'NONE',  ( 56.97280603064898941, -277.2763395528616002, -5.471072653611063430 ) ) ;
#4372 = AXIS2_PLACEMENT_3D ( 'NONE', #43, #27780, #30313 ) ;
#4373 = CARTESIAN_POINT ( 'NONE',  ( 29.35001421184127324, -4.582605737176272953, -4.522129901861162260 ) ) ;
#4374 = FACE_OUTER_BOUND ( 'NONE', #20381, .T. ) ;
#4375 = VERTEX_POINT ( 'NONE', #13833 ) ;
#4376 = CIRCLE ( 'NONE', #19337, 10.94895958125474245 ) ;
#4377 = VECTOR ( 'NONE', #25290, 1000.000000000000227 ) ;
#4378 = DIRECTION ( 'NONE',  ( -0.8476835837759374437, 0.5305021600302710638, 0.000000000000000000 ) ) ;
#4379 = AXIS2_PLACEMENT_3D ( 'NONE', #340, #10513, #18196 ) ;
#4380 = ORIENTED_EDGE ( 'NONE', *, *, #28017, .F. ) ;
#4381 = DIRECTION ( 'NONE',  ( 0.000000000000000000, -1.000000000000000000, 0.000000000000000000 ) ) ;
#4383 = ORIENTED_EDGE ( 'NONE', *, *, #26972, .T. ) ;
#4382 = CARTESIAN_POINT ( 'NONE',  ( 69.01321520914181917, -4.970018244500666427, -3.993434826699699514 ) ) ;
#4384 = ORIENTED_EDGE ( 'NONE', *, *, #7055, .T. ) ;
#4385 = ADVANCED_FACE ( 'NONE', ( #21717 ), #27306, .T. ) ;
#4386 = CARTESIAN_POINT ( 'NONE',  ( 2.898814881667754584, -7.987392794009419816, 5.028251054972114886 ) ) ;
#4387 = EDGE_CURVE ( 'NONE', #4009, #12812, #6015, .T. ) ;
#4388 = CIRCLE ( 'NONE', #21467, 4.000000000000001776 ) ;
#4390 = AXIS2_PLACEMENT_3D ( 'NONE', #475, #643, #17877 ) ;
#4389 = CARTESIAN_POINT ( 'NONE',  ( 29.38825086720287771, -3.456623792451290811, 2.713652344655541615 ) ) ;
#4392 = VERTEX_POINT ( 'NONE', #16213 ) ;
#4391 = CARTESIAN_POINT ( 'NONE',  ( 107.4398938657686671, -17.21413326613983941, 4.222672820008001260 ) ) ;
#4393 = CARTESIAN_POINT ( 'NONE',  ( 23.60846595399739911, 18.33789664323239421, -1.500000000000000000 ) ) ;
#4394 = CARTESIAN_POINT ( 'NONE',  ( 8.911384905465460804, 0.2172754300401000538, -1.412391582771750365 ) ) ;
#4395 = EDGE_CURVE ( 'NONE', #23437, #29657, #24098, .T. ) ;
#4396 = CARTESIAN_POINT ( 'NONE',  ( 9.282537329959909655, 0.2172754300399125094, 1.041239158277188048 ) ) ;
#4397 = CARTESIAN_POINT ( 'NONE',  ( 8.690022415557999480, -0.1784382875756254372, -1.500000000000000000 ) ) ;
#4399 = VERTEX_POINT ( 'NONE', #8845 ) ;
#4398 = CARTESIAN_POINT ( 'NONE',  ( 108.0076416556349841, -18.17940005675781379, -4.637887581615233401 ) ) ;
#4400 = CARTESIAN_POINT ( 'NONE',  ( 2.382865613620174905, -1.226387906749791482E-16, 1.292893218813452982 ) ) ;
#4401 = AXIS2_PLACEMENT_3D ( 'NONE', #12060, #17243, #27445 ) ;
#4402 = AXIS2_PLACEMENT_3D ( 'NONE', #30318, #27125, #4416 ) ;
#4403 = CARTESIAN_POINT ( 'NONE',  ( -38.14293509397970183, 21.94000000000000128, 1.500000000000000000 ) ) ;
#4404 = CARTESIAN_POINT ( 'NONE',  ( 25.17250000136559507, -2.363507492473152283, -1.913930629741525280 ) ) ;
#4405 = AXIS2_PLACEMENT_3D ( 'NONE', #22355, #12157, #29732 ) ;
#4406 = AXIS2_PLACEMENT_3D ( 'NONE', #23165, #87, #10093 ) ;
#4407 = DIRECTION ( 'NONE',  ( -3.623545766764139434E-17, -0.4226182617406906705, -0.9063077870366540445 ) ) ;
#4408 = CIRCLE ( 'NONE', #27878, 0.05000000000000143219 ) ;
#4409 = LINE ( 'NONE', #17277, #1697 ) ;
#4410 = CARTESIAN_POINT ( 'NONE',  ( 10.57125986779756843, -0.6226916219171712008, -4.971152295393308052 ) ) ;
#4411 = VERTEX_POINT ( 'NONE', #14015 ) ;
#4412 = DIRECTION ( 'NONE',  ( 1.000000000000000000, 0.000000000000000000, -0.000000000000000000 ) ) ;
#4413 = CIRCLE ( 'NONE', #2827, 10.95101833074431852 ) ;
#4414 = CLOSED_SHELL ( 'NONE', ( #8963, #5866, #15214, #16706, #1998, #8735, #11094, #9310, #32964, #22541, #13934, #8865, #2367, #27788, #33066, #23886, #16101, #17549, #5293, #22009, #32301, #1270, #19495, #23457, #23706, #20413, #10270 ) ) ;
#4415 = CIRCLE ( 'NONE', #8155, 8.750000000000000000 ) ;
#4416 = DIRECTION ( 'NONE',  ( 0.000000000000000000, -0.9961946980917466554, 0.08715574274764535667 ) ) ;
#4417 = LINE ( 'NONE', #14249, #25818 ) ;
#4418 = ORIENTED_EDGE ( 'NONE', *, *, #13371, .F. ) ;
#4419 = AXIS2_PLACEMENT_3D ( 'NONE', #330, #10503, #18183 ) ;
#4420 = FACE_OUTER_BOUND ( 'NONE', #26443, .T. ) ;
#4421 = CARTESIAN_POINT ( 'NONE',  ( 0.000000000000000000, 5.471841788314708133, 3.018103451449746899 ) ) ;
#4422 = ORIENTED_EDGE ( 'NONE', *, *, #33077, .F. ) ;
#4423 = CARTESIAN_POINT ( 'NONE',  ( 7.196283458169095759, -7.682271642713033089, 1.000000000000000444 ) ) ;
#4424 = ORIENTED_EDGE ( 'NONE', *, *, #5940, .T. ) ;
#4425 = EDGE_CURVE ( 'NONE', #3368, #15820, #8076, .T. ) ;
#4426 = CIRCLE ( 'NONE', #13982, 8.500000000000000000 ) ;
#4427 = ORIENTED_EDGE ( 'NONE', *, *, #28258, .T. ) ;
#4428 = FACE_OUTER_BOUND ( 'NONE', #9884, .T. ) ;
#4429 = VECTOR ( 'NONE', #24258, 1000.000000000000114 ) ;
#4431 = ORIENTED_EDGE ( 'NONE', *, *, #3964, .T. ) ;
#4430 = FACE_OUTER_BOUND ( 'NONE', #15913, .T. ) ;
#4432 = ORIENTED_EDGE ( 'NONE', *, *, #25378, .F. ) ;
#4433 = CARTESIAN_POINT ( 'NONE',  ( 24.17250000136559507, -2.363507492473152283, -1.913930629741525280 ) ) ;
#4434 = VECTOR ( 'NONE', #28813, 1000.000000000000114 ) ;
#4435 = AXIS2_PLACEMENT_3D ( 'NONE', #8010, #5347, #28092 ) ;
#4436 = VECTOR ( 'NONE', #13117, 1000.000000000000000 ) ;
#4437 = EDGE_LOOP ( 'NONE', ( #15762, #12391, #14912, #15303 ) ) ;
#4438 = DIRECTION ( 'NONE',  ( 0.000000000000000000, 1.000000000000000000, 0.000000000000000000 ) ) ;
#4440 = ORIENTED_EDGE ( 'NONE', *, *, #5741, .T. ) ;
#4439 = CARTESIAN_POINT ( 'NONE',  ( 35.33811999952403227, -4.049688432971476182, -1.529339875353190825 ) ) ;
#4441 = CARTESIAN_POINT ( 'NONE',  ( -56.61120226097368402, 0.1221716369093696630, -1.032972126671726221 ) ) ;
#4442 = AXIS2_PLACEMENT_3D ( 'NONE', #7153, #32251, #9313 ) ;
#4443 = CARTESIAN_POINT ( 'NONE',  ( 18.51491971917340607, -8.599446730134173933, 0.07017451552781736601 ) ) ;
#4444 = CARTESIAN_POINT ( 'NONE',  ( 22.67250000136559507, 2.363507492473148286, 1.913930629741525058 ) ) ;
#4445 = CARTESIAN_POINT ( 'NONE',  ( -14.63259398290947289, -27.93932300454937590, -0.9045955023117272509 ) ) ;
#4446 = CIRCLE ( 'NONE', #639, 297.9081695149526468 ) ;
#4447 = CARTESIAN_POINT ( 'NONE',  ( -2.092582746845232489, -9.051626392537000854, -5.485967528433938867 ) ) ;
#4448 = DIRECTION ( 'NONE',  ( 1.000000000000000000, -8.574039729943018344E-17, -0.000000000000000000 ) ) ;
#4449 = LINE ( 'NONE', #1943, #6629 ) ;
#4450 = CARTESIAN_POINT ( 'NONE',  ( 3.008223337240918838, 8.722904517541643088, 2.275671791456698845 ) ) ;
#4451 = CARTESIAN_POINT ( 'NONE',  ( -2.223027892448377951, -2.927336879245634460, 4.522129901861159595 ) ) ;
#4452 = CIRCLE ( 'NONE', #1250, 0.5000000000000004441 ) ;
#4453 = CARTESIAN_POINT ( 'NONE',  ( 3.249999999999999556, 3.174628368996075256, 8.152713396088774545 ) ) ;
#4454 = CARTESIAN_POINT ( 'NONE',  ( 41.19430503359171070, -3.886431767412232396, 0.02339150516273359043 ) ) ;
#4455 = ADVANCED_FACE ( 'NONE', ( #1496 ), #6252, .F. ) ;
#4456 = CIRCLE ( 'NONE', #12989, 10.19912342234043834 ) ;
#4457 = PLANE ( 'NONE',  #28427 ) ;
#4458 = CARTESIAN_POINT ( 'NONE',  ( -6.350050802731187716, -2.983565686104819648, -0.3135853898029605791 ) ) ;
#4459 = ORIENTED_EDGE ( 'NONE', *, *, #28987, .T. ) ;
#4460 = VECTOR ( 'NONE', #32921, 1000.000000000000000 ) ;
#4461 = CIRCLE ( 'NONE', #23145, 6.035938585833444670 ) ;
#4462 = CARTESIAN_POINT ( 'NONE',  ( -4.150050799999999818, 0.9222479816126443186, 3.113457007523260156 ) ) ;
#4463 = EDGE_CURVE ( 'NONE', #17640, #22010, #24999, .T. ) ;
#4464 = CARTESIAN_POINT ( 'NONE',  ( 23.19698494435080960, -21.93770714115886378, -1.040523891066395201 ) ) ;
#4465 = CARTESIAN_POINT ( 'NONE',  ( 3.499999999999999556, -0.1221666339524086348, 6.247805719894683918 ) ) ;
#4466 = PRODUCT_DEFINITION_FORMATION_WITH_SPECIFIED_SOURCE ( 'ANY', '', #25253, .NOT_KNOWN. ) ;
#4467 = ORIENTED_EDGE ( 'NONE', *, *, #21807, .F. ) ;
#4468 = CARTESIAN_POINT ( 'NONE',  ( -2.156376981307136287, 0.1572233378491263989, -2.999999999999999556 ) ) ;
#4469 = ORIENTED_EDGE ( 'NONE', *, *, #17760, .F. ) ;
#4470 = DIRECTION ( 'NONE',  ( 0.000000000000000000, -0.9510565162951502005, -0.3090169943749573878 ) ) ;
#4471 = PERSON_AND_ORGANIZATION ( #6766, #25292 ) ;
#4472 = CARTESIAN_POINT ( 'NONE',  ( 6.037141879243262288, 5.783072176360644079, 6.194548269014904740 ) ) ;
#4474 = EDGE_CURVE ( 'NONE', #9606, #16325, #7290, .T. ) ;
#4473 = ORIENTED_EDGE ( 'NONE', *, *, #31259, .F. ) ;
#4475 = CARTESIAN_POINT ( 'NONE',  ( -3.135269660805080516, -0.5000000000000000000, 1.500000000000000000 ) ) ;
#4476 = EDGE_CURVE ( 'NONE', #3441, #1994, #24673, .T. ) ;
#4477 = CARTESIAN_POINT ( 'NONE',  ( 56.97280603064898941, -277.2763395528616002, -4.999054092451827636 ) ) ;
#4478 = CIRCLE ( 'NONE', #5002, 8.750000000000000000 ) ;
#4479 = CARTESIAN_POINT ( 'NONE',  ( 18.77836082091640080, -5.654703931375024695, -4.215290389458773213 ) ) ;
#4480 = CARTESIAN_POINT ( 'NONE',  ( -41.30970132048468457, -16.45499999999997343, 1.500000000000000000 ) ) ;
#4481 = DIRECTION ( 'NONE',  ( 0.000000000000000000, 0.000000000000000000, 1.000000000000000000 ) ) ;
#4482 = ORIENTED_EDGE ( 'NONE', *, *, #14680, .F. ) ;
#4483 = ADVANCED_FACE ( 'NONE', ( #24848 ), #1966, .T. ) ;
#4484 = CARTESIAN_POINT ( 'NONE',  ( 8.900602013106571064, 0.09531162291654332597, 1.304562659182832540 ) ) ;
#4485 = CARTESIAN_POINT ( 'NONE',  ( 23.22564588060109259, -21.93932300456764040, -1.000000000000000000 ) ) ;
#4486 = CARTESIAN_POINT ( 'NONE',  ( -15.51216819290874227, 0.000000000000000000, 1.000000000000000000 ) ) ;
#4488 = ORIENTED_EDGE ( 'NONE', *, *, #16769, .F. ) ;
#4487 = FACE_OUTER_BOUND ( 'NONE', #14201, .T. ) ;
#4489 = CARTESIAN_POINT ( 'NONE',  ( 107.6901625442183672, 19.30163305711951338, -4.728018791096159745 ) ) ;
#4490 = CARTESIAN_POINT ( 'NONE',  ( 69.09268213438591033, -2.232183665269761086, 0.07017451552781951707 ) ) ;
#4491 = DIRECTION ( 'NONE',  ( 0.000000000000000000, 0.000000000000000000, 1.000000000000000000 ) ) ;
#4492 = DIRECTION ( 'NONE',  ( 1.000000000000000000, -8.574039729943018344E-17, -0.000000000000000000 ) ) ;
#4493 = CARTESIAN_POINT ( 'NONE',  ( 0.7632845268430009655, 4.729683950891516275, 7.360373001717795738 ) ) ;
#4494 = CC_DESIGN_APPROVAL ( #29231, ( #2068 ) ) ;
#4495 = EDGE_CURVE ( 'NONE', #27584, #593, #21827, .T. ) ;
#4496 = DIRECTION ( 'NONE',  ( -0.08910563629484094528, -0.9960221812693187404, 0.000000000000000000 ) ) ;
#4497 = CARTESIAN_POINT ( 'NONE',  ( 6.357668022120090079, -6.210015626210345197, -5.959864878090739282 ) ) ;
#4498 = CARTESIAN_POINT ( 'NONE',  ( -2.500050800000000351, -0.3135853898029607456, 2.983565686104819648 ) ) ;
#4499 = PLANE ( 'NONE',  #24113 ) ;
#4500 = EDGE_LOOP ( 'NONE', ( #30114, #13348, #31409, #21095 ) ) ;
#4501 = CARTESIAN_POINT ( 'NONE',  ( 20.98500000273118715, -0.2613211581691358698, -2.486304738420681559 ) ) ;
#4502 = ORIENTED_EDGE ( 'NONE', *, *, #32372, .T. ) ;
#4503 = CARTESIAN_POINT ( 'NONE',  ( -5.904531657079157725, 2.975847129947406522, 0.3127741368606808403 ) ) ;
#4504 = VECTOR ( 'NONE', #31906, 1000.000000000000114 ) ;
#4505 = CARTESIAN_POINT ( 'NONE',  ( 25.04750000136559507, -1.913930629741527500, 2.363507492473149618 ) ) ;
#4506 = AXIS2_PLACEMENT_3D ( 'NONE', #19523, #19025, #29720 ) ;
#4507 = CARTESIAN_POINT ( 'NONE',  ( 25.75999999999998380, 2.578868840510358584, 1.660716374619295443 ) ) ;
#4508 = FACE_OUTER_BOUND ( 'NONE', #5786, .T. ) ;
#4509 = EDGE_LOOP ( 'NONE', ( #32318, #7322, #32085, #31877, #10658 ) ) ;
#4510 = ORIENTED_EDGE ( 'NONE', *, *, #25925, .F. ) ;
#4511 = APPLICATION_PROTOCOL_DEFINITION ( 'international standard', 'config_control_design', 1994, #31920 ) ;
#4512 = EDGE_CURVE ( 'NONE', #14095, #2672, #20244, .T. ) ;
#4514 = CARTESIAN_POINT ( 'NONE',  ( 54.97700003622870213, -6.498459964805339162, 4.006107073540763786 ) ) ;
#4513 = CC_DESIGN_SECURITY_CLASSIFICATION ( #6102, ( #33103 ) ) ;
#4515 = EDGE_CURVE ( 'NONE', #18559, #11672, #16979, .T. ) ;
#4516 = DIRECTION ( 'NONE',  ( 1.000000000000000000, -0.000000000000000000, -0.000000000000000000 ) ) ;
#4518 = DIRECTION ( 'NONE',  ( -0.000000000000000000, -0.7071067811865516806, 0.7071067811865434649 ) ) ;
#4517 = CARTESIAN_POINT ( 'NONE',  ( 5.612718761614564400, 7.212912035758809459, 3.934162523501257613 ) ) ;
#4519 = ORIENTED_EDGE ( 'NONE', *, *, #5574, .F. ) ;
#4520 = LINE ( 'NONE', #6833, #11910 ) ;
#4521 = CARTESIAN_POINT ( 'NONE',  ( 3.063284526839887167, 8.734705317681626724, -0.4999240074894737984 ) ) ;
#4522 = CARTESIAN_POINT ( 'NONE',  ( 25.73500000136559507, 3.156283516753366047, 0.9349337715887203748 ) ) ;
#4523 = CARTESIAN_POINT ( 'NONE',  ( 9.144688568536819773, -14.26363490968651071, -1.499999999999999556 ) ) ;
#4525 = ORIENTED_EDGE ( 'NONE', *, *, #10065, .T. ) ;
#4524 = CARTESIAN_POINT ( 'NONE',  ( 6.013832568680315127, -13.53405802968792848, 1.500000000000000444 ) ) ;
#4526 = CIRCLE ( 'NONE', #9860, 4.999999999999999112 ) ;
#4527 = CARTESIAN_POINT ( 'NONE',  ( -2.987550801365593145, -0.3701630799359326152, 3.521866450007987037 ) ) ;
#4528 = DIRECTION ( 'NONE',  ( 0.000000000000000000, 0.000000000000000000, -1.000000000000000000 ) ) ;
#4529 = CARTESIAN_POINT ( 'NONE',  ( 3.063284526839887167, -8.734705317681623171, -0.4999240074895356933 ) ) ;
#4530 = CARTESIAN_POINT ( 'NONE',  ( 108.1293191351601877, -19.93152549159189135, -2.509206947347181416 ) ) ;
#4531 = ORIENTED_EDGE ( 'NONE', *, *, #15541, .T. ) ;
#4533 = VERTEX_POINT ( 'NONE', #4284 ) ;
#4532 = CARTESIAN_POINT ( 'NONE',  ( 13.61462910219950473, 21.93664948940024928, 1.110678092886302260 ) ) ;
#4534 = EDGE_CURVE ( 'NONE', #22777, #3718, #2326, .T. ) ;
#4535 = CC_DESIGN_DATE_AND_TIME_ASSIGNMENT ( #3011, #18368, ( #15168 ) ) ;
#4536 = CARTESIAN_POINT ( 'NONE',  ( 0.000000000000000000, 0.000000000000000000, 0.000000000000000000 ) ) ;
#4537 = CARTESIAN_POINT ( 'NONE',  ( 6.038144853276842916, 8.256557579931664392, 1.911563584435225005 ) ) ;
#4538 = CARTESIAN_POINT ( 'NONE',  ( -20.19984785985500508, 17.54567542505805733, 1.795026885182644749 ) ) ;
#4539 = CARTESIAN_POINT ( 'NONE',  ( -30.01044711289841516, 13.10789634492816447, 1.904575337205761887 ) ) ;
#4540 = CARTESIAN_POINT ( 'NONE',  ( -1.898110288140231861, -13.58794273181078438, -1.499999999999999556 ) ) ;
#4541 = DIRECTION ( 'NONE',  ( -1.000000000000000000, 0.000000000000000000, 0.000000000000000000 ) ) ;
#4542 = CARTESIAN_POINT ( 'NONE',  ( 54.90427307174406479, -3.885678510653658879, 1.529339875079268829 ) ) ;
#4543 = CARTESIAN_POINT ( 'NONE',  ( 85.45070076415389337, -7.158483446636730640, 2.713652344655544724 ) ) ;
#4544 = EDGE_LOOP ( 'NONE', ( #21828, #31758, #20018, #27758 ) ) ;
#4545 = LINE ( 'NONE', #22403, #4937 ) ;
#4546 = ORIENTED_EDGE ( 'NONE', *, *, #17931, .T. ) ;
#4547 = EDGE_CURVE ( 'NONE', #5967, #23561, #19294, .T. ) ;
#4548 = AXIS2_PLACEMENT_3D ( 'NONE', #22580, #32300, #12193 ) ;
#4549 = CARTESIAN_POINT ( 'NONE',  ( 13.62547635268498780, 21.94000000000002970, 1.050000000000000044 ) ) ;
#4550 =( NAMED_UNIT ( * ) SI_UNIT ( $, .STERADIAN. ) SOLID_ANGLE_UNIT ( ) );
#4551 = DIRECTION ( 'NONE',  ( 0.9993908270190957621, -0.03489949670250111491, 0.000000000000000000 ) ) ;
#4552 = VERTEX_POINT ( 'NONE', #31032 ) ;
#4553 = FACE_OUTER_BOUND ( 'NONE', #22215, .T. ) ;
#4554 = VERTEX_POINT ( 'NONE', #17994 ) ;
#4555 = DIRECTION ( 'NONE',  ( 1.000000000000000000, -0.000000000000000000, -0.000000000000000000 ) ) ;
#4557 = ORIENTED_EDGE ( 'NONE', *, *, #8931, .F. ) ;
#4556 = CARTESIAN_POINT ( 'NONE',  ( 54.94583599702954757, -5.372455163404658229, -4.013697991747248395 ) ) ;
#4558 = ORIENTED_EDGE ( 'NONE', *, *, #30929, .T. ) ;
#4559 = DIRECTION ( 'NONE',  ( 1.000000000000000000, -0.000000000000000000, -0.000000000000000000 ) ) ;
#4560 = CARTESIAN_POINT ( 'NONE',  ( 47.99837860531645362, -3.577301031424839906, 2.713652344655541615 ) ) ;
#4562 = ORIENTED_EDGE ( 'NONE', *, *, #6001, .F. ) ;
#4561 = DIRECTION ( 'NONE',  ( 0.9563911903463306885, -1.156482317317869713E-14, 0.2920888409849449752 ) ) ;
#4563 = CARTESIAN_POINT ( 'NONE',  ( 22.43659417819815616, 17.13630711803212492, -1.050000000000000044 ) ) ;
#4564 = LINE ( 'NONE', #31975, #30953 ) ;
#4565 = SPHERICAL_SURFACE ( 'NONE', #23062, 0.5000000000000000000 ) ;
#4566 = CARTESIAN_POINT ( 'NONE',  ( 5.338982705821348503E-17, 0.6226916219172716760, -4.971152295393295617 ) ) ;
#4569 = EDGE_CURVE ( 'NONE', #32499, #17584, #8294, .T. ) ;
#4568 = ORIENTED_EDGE ( 'NONE', *, *, #25358, .T. ) ;
#4567 = CARTESIAN_POINT ( 'NONE',  ( 107.9910452807461638, -17.94041638701884267, -4.566009972856815757 ) ) ;
#4570 = CARTESIAN_POINT ( 'NONE',  ( 2.589202905186824388, -9.453729690310135325, -4.126870756446575861 ) ) ;
#4571 = CARTESIAN_POINT ( 'NONE',  ( 34.55410851074696410, 0.5000000000000000000, -3.046816775802624999 ) ) ;
#4572 = SPHERICAL_SURFACE ( 'NONE', #15202, 0.5000000000000000000 ) ;
#4573 = CARTESIAN_POINT ( 'NONE',  ( 108.2840637929627832, 19.75993920996065967, -3.567582149746106435 ) ) ;
#4574 = DIRECTION ( 'NONE',  ( -1.000000000000000000, 0.000000000000000000, 0.000000000000000000 ) ) ;
#4575 = DIRECTION ( 'NONE',  ( 0.000000000000000000, 0.000000000000000000, 1.000000000000000000 ) ) ;
#4576 = ORIENTED_EDGE ( 'NONE', *, *, #4084, .T. ) ;
#4577 = DIRECTION ( 'NONE',  ( 0.000000000000000000, 0.000000000000000000, -1.000000000000000000 ) ) ;
#4578 = PLANE ( 'NONE',  #16118 ) ;
#4579 = ADVANCED_FACE ( 'NONE', ( #15809 ), #4965, .T. ) ;
#4580 = CARTESIAN_POINT ( 'NONE',  ( -6.137550801365595277, -1.828967928396026732, 3.368539882008728004 ) ) ;
#4581 = VERTEX_POINT ( 'NONE', #15461 ) ;
#4582 = EDGE_CURVE ( 'NONE', #16032, #15630, #18325, .T. ) ;
#4583 = EDGE_CURVE ( 'NONE', #24312, #4070, #18141, .T. ) ;
#4584 = CARTESIAN_POINT ( 'NONE',  ( 25.00111451137534146, -4.139597703811366476E-17, -2.499999999999998668 ) ) ;
#4585 = LINE ( 'NONE', #1741, #23682 ) ;
#4586 = EDGE_LOOP ( 'NONE', ( #33037, #14307, #27680, #25195 ) ) ;
#4587 = LINE ( 'NONE', #17441, #7019 ) ;
#4588 = ORIENTED_EDGE ( 'NONE', *, *, #10902, .F. ) ;
#4589 = VERTEX_POINT ( 'NONE', #25860 ) ;
#4590 = LINE ( 'NONE', #12101, #25214 ) ;
#4592 = EDGE_LOOP ( 'NONE', ( #29294, #28533, #3179, #8053 ) ) ;
#4591 = LINE ( 'NONE', #26815, #21854 ) ;
#4593 = EDGE_LOOP ( 'NONE', ( #27261, #26979, #6287, #31088 ) ) ;
#4594 = CARTESIAN_POINT ( 'NONE',  ( 23.54750000136559507, 3.024605502323846729, -0.3178988483021056854 ) ) ;
#4595 = EDGE_LOOP ( 'NONE', ( #6117, #25342, #29758, #26951 ) ) ;
#4596 = CARTESIAN_POINT ( 'NONE',  ( 4.749760686538667009, 7.530955069117513112, 2.741043480754951744 ) ) ;
#4598 = VERTEX_POINT ( 'NONE', #25670 ) ;
#4597 = DIRECTION ( 'NONE',  ( -1.000000000000000000, 2.473959037481237219E-13, -0.000000000000000000 ) ) ;
#4599 = CARTESIAN_POINT ( 'NONE',  ( 2.274274201627632941, 1.975651141464536797, -10.82112760146234720 ) ) ;
#4600 = FACE_OUTER_BOUND ( 'NONE', #29901, .T. ) ;
#4601 = CARTESIAN_POINT ( 'NONE',  ( 23.73500000136559152, 1.570731468192929858, 2.892927487894329186 ) ) ;
#4602 = CARTESIAN_POINT ( 'NONE',  ( 0.7632845268449801601, 2.223716399040764014, 8.461683424485153537 ) ) ;
#4603 = LINE ( 'NONE', #12448, #17148 ) ;
#4604 = CARTESIAN_POINT ( 'NONE',  ( 109.3697760341437828, 14.49066428361113346, 0.4463807625373157340 ) ) ;
#4605 = CYLINDRICAL_SURFACE ( 'NONE', #23213, 5.000000000000000888 ) ;
#4606 = CARTESIAN_POINT ( 'NONE',  ( -35.00000000000000000, 0.5000000000000000000, -2.982234843104710986 ) ) ;
#4607 = DIRECTION ( 'NONE',  ( -0.9960221812693186294, 0.08910563629484180570, 0.000000000000000000 ) ) ;
#4608 = DIRECTION ( 'NONE',  ( 0.000000000000000000, 1.000000000000000000, 0.000000000000000000 ) ) ;
#4609 = CARTESIAN_POINT ( 'NONE',  ( 23.84714171513466141, -3.444070612163573575, 0.02339150516273077324 ) ) ;
#4610 = CYLINDRICAL_SURFACE ( 'NONE', #12929, 0.5000000000000004441 ) ;
#4611 = EDGE_CURVE ( 'NONE', #15271, #17041, #23555, .T. ) ;
#4612 = ADVANCED_FACE ( 'NONE', ( #30542 ), #13279, .T. ) ;
#4613 = CARTESIAN_POINT ( 'NONE',  ( -3.100050802731187272, -2.853674364686378695, -1.549418761218566809 ) ) ;
#4614 = VERTEX_POINT ( 'NONE', #11112 ) ;
#4615 = EDGE_CURVE ( 'NONE', #2199, #10723, #933, .T. ) ;
#4616 = CARTESIAN_POINT ( 'NONE',  ( -4.600050799999999995, -1.887961173149512062, -2.331437884370912261 ) ) ;
#4617 = CARTESIAN_POINT ( 'NONE',  ( 16.36487458112951643, 19.37645981759113667, -4.612695725900422872 ) ) ;
#4618 = CARTESIAN_POINT ( 'NONE',  ( 10.00000000000000178, -8.574039729943018837E-16, 0.000000000000000000 ) ) ;
#4619 = VERTEX_POINT ( 'NONE', #13615 ) ;
#4620 = CARTESIAN_POINT ( 'NONE',  ( -2.050050802731187449, 2.331437884370912705, -1.887961173149511618 ) ) ;
#4621 = VERTEX_POINT ( 'NONE', #3458 ) ;
#4622 = DIRECTION ( 'NONE',  ( -1.000000000000000000, -0.000000000000000000, 0.000000000000000000 ) ) ;
#4623 = PERSON_AND_ORGANIZATION ( #6766, #25292 ) ;
#4624 = CARTESIAN_POINT ( 'NONE',  ( 0.000000000000000000, 5.471841788314749877, -3.018103451449674068 ) ) ;
#4625 = ORIENTED_EDGE ( 'NONE', *, *, #28956, .F. ) ;
#4626 = CARTESIAN_POINT ( 'NONE',  ( 0.5664946525207626982, 9.241976615239526183, 2.300561732649596181 ) ) ;
#4627 = ORIENTED_EDGE ( 'NONE', *, *, #3383, .T. ) ;
#4628 = CARTESIAN_POINT ( 'NONE',  ( 107.9852729111968728, -17.85729570149337064, -4.475837141004190833 ) ) ;
#4629 = CARTESIAN_POINT ( 'NONE',  ( 9.295274190224857236, 0.2358592590667328848, -1.049999640971083892 ) ) ;
#4630 = DIRECTION ( 'NONE',  ( 0.000000000000000000, 0.000000000000000000, 1.000000000000000000 ) ) ;
#4631 = DIRECTION ( 'NONE',  ( -1.000000000000000000, 8.574039729943018344E-17, -0.000000000000000000 ) ) ;
#4632 = EDGE_LOOP ( 'NONE', ( #27455, #14111, #31030, #21166 ) ) ;
#4633 = FACE_OUTER_BOUND ( 'NONE', #29254, .T. ) ;
#4634 = LINE ( 'NONE', #1973, #20469 ) ;
#4636 = ORIENTED_EDGE ( 'NONE', *, *, #11276, .F. ) ;
#4635 = LINE ( 'NONE', #31001, #30991 ) ;
#4637 = ADVANCED_FACE ( 'NONE', ( #5928 ), #26352, .T. ) ;
#4638 = DIRECTION ( 'NONE',  ( -1.000000000000000000, 0.000000000000000000, -0.000000000000000000 ) ) ;
#4639 = CARTESIAN_POINT ( 'NONE',  ( 10.00000000000000000, 0.8254815157535864145, -4.681538312723508177 ) ) ;
#4640 = CARTESIAN_POINT ( 'NONE',  ( 0.1606232843943643518, 1.177222770082358316, -10.56438947504860337 ) ) ;
#4641 = CARTESIAN_POINT ( 'NONE',  ( 10.56870887191539587, -4.787500056513379398, 1.476463073999619846 ) ) ;
#4642 = EDGE_CURVE ( 'NONE', #18387, #25095, #2215, .T. ) ;
#4643 = CARTESIAN_POINT ( 'NONE',  ( 18.80941384712784981, -5.307593421039076276, -3.636029349014984202 ) ) ;
#4644 = DIRECTION ( 'NONE',  ( -1.000000000000000000, 0.000000000000000000, 0.000000000000000000 ) ) ;
#4645 = CARTESIAN_POINT ( 'NONE',  ( -56.44230307511855216, 0.02673048711865717159, -1.015476362562965251 ) ) ;
#4646 = PLANE ( 'NONE',  #7067 ) ;
#4647 = VERTEX_POINT ( 'NONE', #31511 ) ;
#4648 = EDGE_CURVE ( 'NONE', #1423, #21855, #28390, .T. ) ;
#4649 = CARTESIAN_POINT ( 'NONE',  ( -2.700050802731186916, 2.853674364686379583, 1.549418761218565921 ) ) ;
#4650 = ORIENTED_EDGE ( 'NONE', *, *, #18095, .T. ) ;
#4651 = CARTESIAN_POINT ( 'NONE',  ( -7.304531657079158080, -0.3127741368606806738, 2.975847129947406522 ) ) ;
#4652 = CARTESIAN_POINT ( 'NONE',  ( 56.97280603064904625, -277.2763395528616002, -554.0683451992334767 ) ) ;
#4653 = EDGE_CURVE ( 'NONE', #1302, #7812, #11298, .T. ) ;
#4654 = CARTESIAN_POINT ( 'NONE',  ( 107.5617723795401872, -18.98359893170738744, -4.522129901861166701 ) ) ;
#4655 = CARTESIAN_POINT ( 'NONE',  ( 41.44907012423725234, -8.741883605788331124, -2.713652344655543391 ) ) ;
#4656 = CARTESIAN_POINT ( 'NONE',  ( 7.249760686538666121, 0.000000000000000000, 0.000000000000000000 ) ) ;
#4657 = ORIENTED_EDGE ( 'NONE', *, *, #3484, .T. ) ;
#4658 = CARTESIAN_POINT ( 'NONE',  ( 21.56498441094940688, -21.75760761563370949, 1.480179746966302945 ) ) ;
#4659 = ORIENTED_EDGE ( 'NONE', *, *, #17436, .F. ) ;
#4660 = CARTESIAN_POINT ( 'NONE',  ( 5.377543748152549874, -5.151476664237518044, 6.139290821770238438 ) ) ;
#4661 = DATE_AND_TIME ( #7834, #18899 ) ;
#4662 = EDGE_CURVE ( 'NONE', #14763, #12234, #23967, .T. ) ;
#4663 = CARTESIAN_POINT ( 'NONE',  ( 18.75945136020123982, -5.866073751327065544, 4.013697994447678496 ) ) ;
#4664 = EDGE_CURVE ( 'NONE', #11567, #20134, #3808, .T. ) ;
#4665 = B_SPLINE_CURVE_WITH_KNOTS ( 'NONE', 3,
 ( #30234, #27379, #12309, #30069, #25189, #7306, #17496, #12796, #2312, #7816 ),
 .UNSPECIFIED., .F., .F.,
 ( 4, 3, 3, 4 ),
 ( 0.000000000000000000, 0.0005352572989639532318, 0.001070514597927906897, 0.002130599830189221569 ),
 .UNSPECIFIED. ) ;
#4666 = CARTESIAN_POINT ( 'NONE',  ( 5.489321676144490958, 4.149060317827602873, -6.978593840069401644 ) ) ;
#4668 = DIRECTION ( 'NONE',  ( -0.000000000000000000, -0.000000000000000000, -1.000000000000000000 ) ) ;
#4667 = CARTESIAN_POINT ( 'NONE',  ( 7.249760686538667009, 6.226446564518003157, -6.147671362329155009 ) ) ;
#4669 = ORIENTED_EDGE ( 'NONE', *, *, #7010, .T. ) ;
#4670 = CARTESIAN_POINT ( 'NONE',  ( -8.000050800000000351, -2.754924098389954779, -1.195686321225201576 ) ) ;
#4671 = CARTESIAN_POINT ( 'NONE',  ( 7.249760686538667009, -5.064320921489771976, -7.135485519862050374 ) ) ;
#4672 = ADVANCED_FACE ( 'NONE', ( #26505 ), #29168, .F. ) ;
#4673 = CARTESIAN_POINT ( 'NONE',  ( 23.54750000136559862, 1.913930629741522838, -2.363507492473150062 ) ) ;
#4674 = CARTESIAN_POINT ( 'NONE',  ( 7.321588594920942938, -13.58956495849201929, -1.499999999999999556 ) ) ;
#4676 = ORIENTED_EDGE ( 'NONE', *, *, #12412, .T. ) ;
#4675 = CARTESIAN_POINT ( 'NONE',  ( 1.828104818894226380, -1.262475772535087915, 1.500000000000000444 ) ) ;
#4677 = CARTESIAN_POINT ( 'NONE',  ( -2.837550801365592790, -3.675193018007246071, 1.088641768524163167 ) ) ;
#4678 = FACE_OUTER_BOUND ( 'NONE', #28401, .T. ) ;
#4679 = EDGE_CURVE ( 'NONE', #14707, #25174, #6112, .T. ) ;
#4680 = DIRECTION ( 'NONE',  ( 0.000000000000000000, 0.000000000000000000, 1.000000000000000000 ) ) ;
#4681 = CARTESIAN_POINT ( 'NONE',  ( 7.249760686538667009, -7.892520144992426268, -1.391664247347309535 ) ) ;
#4682 = ORIENTED_EDGE ( 'NONE', *, *, #15933, .T. ) ;
#4684 = VERTEX_POINT ( 'NONE', #23485 ) ;
#4683 = CARTESIAN_POINT ( 'NONE',  ( 22.16261821944387123, -17.22505787984022874, 1.541391846741430260 ) ) ;
#4685 = DIRECTION ( 'NONE',  ( -0.9164966213036979115, 0.4000424266736042900, 0.000000000000000000 ) ) ;
#4686 = DIRECTION ( 'NONE',  ( -1.000000000000000000, -0.000000000000000000, -0.000000000000000000 ) ) ;
#4687 = DIRECTION ( 'NONE',  ( -1.000000000000000000, -0.000000000000000000, -0.000000000000000000 ) ) ;
#4688 = EDGE_CURVE ( 'NONE', #27483, #32821, #16295, .T. ) ;
#4689 = EDGE_CURVE ( 'NONE', #31644, #3406, #6584, .T. ) ;
#4690 = CARTESIAN_POINT ( 'NONE',  ( -16.41799616858202171, 10.20678673897635313, 1.500000000000000000 ) ) ;
#4691 = CARTESIAN_POINT ( 'NONE',  ( -30.67627260417763679, 10.20678673897636912, 1.500000000000000000 ) ) ;
#4692 = CARTESIAN_POINT ( 'NONE',  ( 10.35382568889080979, -19.59147244278173261, -1.750308525318766684 ) ) ;
#4693 = CARTESIAN_POINT ( 'NONE',  ( 7.249760686538667009, 7.199384779417119518, 4.973063321323901498 ) ) ;
#4694 = PRODUCT ( 'Part1_handle1', 'Part1_handle1', '', ( #26859 ) ) ;
#4695 = CARTESIAN_POINT ( 'NONE',  ( 29.33867311914967146, -3.750126786196623652, 0.8105614676246016836 ) ) ;
#4696 = DIRECTION ( 'NONE',  ( -1.000000000000000000, -0.000000000000000000, 0.000000000000000000 ) ) ;
#4697 = EDGE_LOOP ( 'NONE', ( #26250, #2972, #15379, #28472 ) ) ;
#4698 = EDGE_CURVE ( 'NONE', #285, #16126, #4095, .T. ) ;
#4699 = DIRECTION ( 'NONE',  ( 0.000000000000000000, 1.000000000000000000, 0.000000000000000000 ) ) ;
#4700 = ORIENTED_EDGE ( 'NONE', *, *, #31970, .T. ) ;
#4701 = CARTESIAN_POINT ( 'NONE',  ( 3.499999999999999556, -5.979767908488853756, 1.814490771706161354 ) ) ;
#4702 = DIRECTION ( 'NONE',  ( 0.4727189256607252088, -0.8170467111647613523, -0.3301082990429303199 ) ) ;
#4703 = CARTESIAN_POINT ( 'NONE',  ( 10.00000000000000000, -4.116875700062099241, 2.376879293651050329 ) ) ;
#4704 = ORIENTED_EDGE ( 'NONE', *, *, #18789, .T. ) ;
#4705 = EDGE_CURVE ( 'NONE', #11560, #19335, #23909, .T. ) ;
#4706 =( BOUNDED_CURVE ( )  B_SPLINE_CURVE ( 2, ( #25489, #5265, #15439, #24776, #32818, #11721, #14882, #12387, #9538, #26958, #17059 ),
 .UNSPECIFIED., .F., .F. ) 
 B_SPLINE_CURVE_WITH_KNOTS ( ( 3, 2, 2, 2, 2, 3 ),
 ( 0.4966116191895003640, 0.5000000000000000000, 0.5250000000000000222, 0.5500000000000000444, 0.5749999999999999556, 0.5966116191895003418 ),
 .UNSPECIFIED. ) 
 CURVE ( )  GEOMETRIC_REPRESENTATION_ITEM ( )  RATIONAL_B_SPLINE_CURVE ( ( 0.9821626249036858880, 0.9896829947469992783, 1.000000000000000000, 0.9238795325112867385, 1.000000000000000000, 0.9238795325112867385, 1.000000000000000000, 0.9238795325112867385, 1.000000000000000000, 0.9341965377642874602, 0.9821626249036858880 ) ) 
 REPRESENTATION_ITEM ( '' )  );
#4707 = CARTESIAN_POINT ( 'NONE',  ( 108.0435829116943438, 18.42084677419104821, -5.131407418483624028 ) ) ;
#4708 = VERTEX_POINT ( 'NONE', #27493 ) ;
#4709 = PLANE ( 'NONE',  #6027 ) ;
#4711 = VERTEX_POINT ( 'NONE', #20478 ) ;
#4710 = CARTESIAN_POINT ( 'NONE',  ( 69.01386799616022927, -4.983101923413928880, -4.013698489648152901 ) ) ;
#4712 = ORIENTED_EDGE ( 'NONE', *, *, #18621, .T. ) ;
#4713 = DIRECTION ( 'NONE',  ( 0.000000000000000000, -1.000000000000000000, 0.000000000000000000 ) ) ;
#4714 = CARTESIAN_POINT ( 'NONE',  ( 29.21519671781910077, -8.552672223075463265, -2.713652344655542059 ) ) ;
#4716 = EDGE_LOOP ( 'NONE', ( #10045, #23819, #18674 ) ) ;
#4715 = CARTESIAN_POINT ( 'NONE',  ( 22.42250000273118715, 1.291182301015469047, 2.378061970571981654 ) ) ;
#4717 = CARTESIAN_POINT ( 'NONE',  ( 107.5617797207340800, -18.98359842993768964, 4.522129901861158707 ) ) ;
#4718 = CARTESIAN_POINT ( 'NONE',  ( 7.249760686538667009, -2.210816291636156006, -8.466096581343503402 ) ) ;
#4719 = DIRECTION ( 'NONE',  ( 1.000000000000000000, 0.000000000000000000, 0.000000000000000000 ) ) ;
#4720 = CARTESIAN_POINT ( 'NONE',  ( 9.283830569144292610, -0.1241467201999828379, -1.500000000000000000 ) ) ;
#4723 = EDGE_CURVE ( 'NONE', #15974, #14650, #2942, .T. ) ;
#4722 = ORIENTED_EDGE ( 'NONE', *, *, #1018, .T. ) ;
#4721 = CARTESIAN_POINT ( 'NONE',  ( 108.0613680874162554, -18.95304730895377432, -4.512352198926723901 ) ) ;
#4724 = CARTESIAN_POINT ( 'NONE',  ( -34.50091246256902622, -0.01740729335041210982, -3.000607876078560388 ) ) ;
#4725 = DIRECTION ( 'NONE',  ( 0.000000000000000000, 0.000000000000000000, 1.000000000000000000 ) ) ;
#4726 = CARTESIAN_POINT ( 'NONE',  ( 23.04750000136559862, -3.024605502323851169, 0.3178988483021052969 ) ) ;
#4727 = ADVANCED_FACE ( 'NONE', ( #12748 ), #2250, .F. ) ;
#4728 = PLANE ( 'NONE',  #10264 ) ;
#4729 = LINE ( 'NONE', #14749, #16616 ) ;
#4730 = FACE_OUTER_BOUND ( 'NONE', #14846, .T. ) ;
#4731 = ORIENTED_EDGE ( 'NONE', *, *, #20687, .T. ) ;
#4732 = CARTESIAN_POINT ( 'NONE',  ( 2.037945749704362236E-16, 2.376879293651122271, -4.116875700062057497 ) ) ;
#4733 = CARTESIAN_POINT ( 'NONE',  ( 25.75960661490314507, 24.76082900280850652, 0.4463807625372899768 ) ) ;
#4734 = CARTESIAN_POINT ( 'NONE',  ( -7.137550801365592612, 3.368539882008727115, 1.828967928396027176 ) ) ;
#4735 = ORIENTED_EDGE ( 'NONE', *, *, #381, .T. ) ;
#4736 = EDGE_CURVE ( 'NONE', #7787, #14600, #8072, .T. ) ;
#4737 = FACE_OUTER_BOUND ( 'NONE', #19242, .T. ) ;
#4738 = CARTESIAN_POINT ( 'NONE',  ( 3.499999999999999556, 0.000000000000000000, 0.000000000000000000 ) ) ;
#4739 = CARTESIAN_POINT ( 'NONE',  ( 0.000000000000000000, -9.915734732513254102, 4.762163868918234400 ) ) ;
#4740 = VERTEX_POINT ( 'NONE', #30845 ) ;
#4741 = DIRECTION ( 'NONE',  ( -1.000000000000000000, 0.000000000000000000, 0.000000000000000000 ) ) ;
#4742 = ORIENTED_EDGE ( 'NONE', *, *, #19419, .T. ) ;
#4743 = EDGE_CURVE ( 'NONE', #12746, #1423, #7913, .T. ) ;
#4744 = ORIENTED_EDGE ( 'NONE', *, *, #25298, .T. ) ;
#4745 = CARTESIAN_POINT ( 'NONE',  ( -2.672624763096138167, -0.4219952926969707807, 1.725256589882031344 ) ) ;
#4747 = ORIENTED_EDGE ( 'NONE', *, *, #20616, .F. ) ;
#4746 = DIRECTION ( 'NONE',  ( -8.519590295723598769E-19, -5.916484360648977690E-20, -1.000000000000000000 ) ) ;
#4748 = ORIENTED_EDGE ( 'NONE', *, *, #1309, .F. ) ;
#4749 = FACE_OUTER_BOUND ( 'NONE', #23268, .T. ) ;
#4750 = VERTEX_POINT ( 'NONE', #2583 ) ;
#4751 = DIRECTION ( 'NONE',  ( -0.000000000000000000, -0.000000000000000000, 1.000000000000000000 ) ) ;
#4753 = ORIENTED_EDGE ( 'NONE', *, *, #5915, .T. ) ;
#4752 = FACE_OUTER_BOUND ( 'NONE', #7083, .T. ) ;
#4754 = DIRECTION ( 'NONE',  ( -1.000000000000000000, 0.000000000000000000, 0.000000000000000000 ) ) ;
#4755 = DIRECTION ( 'NONE',  ( -1.000000000000000000, 0.000000000000000000, 0.000000000000000000 ) ) ;
#4756 = FACE_OUTER_BOUND ( 'NONE', #31174, .T. ) ;
#4757 = EDGE_CURVE ( 'NONE', #31656, #6932, #7021, .T. ) ;
#4758 = ADVANCED_FACE ( 'NONE', ( #23142 ), #29435, .T. ) ;
#4759 = CARTESIAN_POINT ( 'NONE',  ( 14.23800746264080885, 22.11259878822730229, -1.491740999229417941 ) ) ;
#4760 = CARTESIAN_POINT ( 'NONE',  ( 107.8806061107227379, -16.35011981549162741, -2.521000801038054906 ) ) ;
#4761 = CARTESIAN_POINT ( 'NONE',  ( 24.55820472632769835, -17.37661330403878424, 1.293157874817708164 ) ) ;
#4762 = FACE_OUTER_BOUND ( 'NONE', #25079, .T. ) ;
#4763 = CARTESIAN_POINT ( 'NONE',  ( 6.220890055303850197, -15.20372210278348035, 4.522129901861156931 ) ) ;
#4764 = LINE ( 'NONE', #28013, #11337 ) ;
#4765 = CARTESIAN_POINT ( 'NONE',  ( 54.64624227588102201, -3.635739347938792054, -0.07017451552781628354 ) ) ;
#4766 = B_SPLINE_CURVE_WITH_KNOTS ( 'NONE', 3,
 ( #6595, #32509, #21794, #22146, #24622, #14411, #9417, #32001, #32357, #1752 ),
 .UNSPECIFIED., .F., .F.,
 ( 4, 2, 2, 2, 4 ),
 ( -0.0003514200626105848141, 0.0001564218602127746675, 0.0006642637830361342033, 0.001679947628682841023, 0.003711315319976244906 ),
 .UNSPECIFIED. ) ;
#4767 = CARTESIAN_POINT ( 'NONE',  ( 4.749760686538667009, 4.007137495034812424, 6.940565734314612101 ) ) ;
#4768 = CARTESIAN_POINT ( 'NONE',  ( -3.200050802731187360, -3.113457007523259268, 0.9222479816126455399 ) ) ;
#4769 = ORIENTED_EDGE ( 'NONE', *, *, #20957, .F. ) ;
#4770 = CARTESIAN_POINT ( 'NONE',  ( -4.350050800000000883, 3.113457007523260156, -0.9222479816126439855 ) ) ;
#4771 = DIRECTION ( 'NONE',  ( 0.000000000000000000, -7.993605777301127091E-15, 1.000000000000000000 ) ) ;
#4772 = CARTESIAN_POINT ( 'NONE',  ( -53.45715098423449518, 5.485000000000009202, 1.500000000000000000 ) ) ;
#4773 = ORIENTED_EDGE ( 'NONE', *, *, #4679, .F. ) ;
#4774 = DIRECTION ( 'NONE',  ( 8.281886410780533213E-17, 0.9659258262890707547, -0.2588190451025115246 ) ) ;
#4775 = CARTESIAN_POINT ( 'NONE',  ( 107.9522592018893192, -17.38190650023669548, 4.650312831055688712 ) ) ;
#4776 = AXIS2_PLACEMENT_3D ( 'NONE', #11344, #8664, #26230 ) ;
#4777 = ORIENTED_EDGE ( 'NONE', *, *, #26555, .F. ) ;
#4778 = CARTESIAN_POINT ( 'NONE',  ( 7.321283561615676838, -13.58944227021806128, 1.499999999999999556 ) ) ;
#4779 = DATE_TIME_ROLE ( 'classification_date' ) ;
#4780 = CARTESIAN_POINT ( 'NONE',  ( 6.749760686538667009, 0.000000000000000000, 0.000000000000000000 ) ) ;
#4781 = ORIENTED_EDGE ( 'NONE', *, *, #5491, .T. ) ;
#4782 = CARTESIAN_POINT ( 'NONE',  ( 34.99999999999999289, 0.5000000000000000000, 2.482234843104954791 ) ) ;
#4783 = ORIENTED_EDGE ( 'NONE', *, *, #32746, .T. ) ;
#4784 = AXIS2_PLACEMENT_3D ( 'NONE', #3465, #6418, #1090 ) ;
#4785 = CARTESIAN_POINT ( 'NONE',  ( 107.9802527803231129, -17.78500706576168611, -4.325704939595124365 ) ) ;
#4786 = CARTESIAN_POINT ( 'NONE',  ( 69.06793210257949056, -6.065973107585926449, -4.074610585182336209 ) ) ;
#4787 = CARTESIAN_POINT ( 'NONE',  ( 7.249760686538667009, -2.210816291636271025, 8.466096581343474980 ) ) ;
#4788 = FACE_OUTER_BOUND ( 'NONE', #19682, .T. ) ;
#4789 = ADVANCED_FACE ( 'NONE', ( #7406 ), #18278, .F. ) ;
#4790 = LINE ( 'NONE', #27536, #23700 ) ;
#4791 = CARTESIAN_POINT ( 'NONE',  ( 1.624999999999999778, 10.90201369670498721, 1.464956435139580515 ) ) ;
#4792 = ADVANCED_FACE ( 'NONE', ( #4749 ), #17601, .T. ) ;
#4793 = ORIENTED_EDGE ( 'NONE', *, *, #3822, .T. ) ;
#4794 = CARTESIAN_POINT ( 'NONE',  ( -5.304000690461529555E-12, -21.43932300456189566, -1.500000000000000000 ) ) ;
#4795 = DIRECTION ( 'NONE',  ( 0.000000000000000000, 1.000000000000000000, 0.000000000000000000 ) ) ;
#4796 = DIRECTION ( 'NONE',  ( -0.000000000000000000, -1.000000000000000000, -0.000000000000000000 ) ) ;
#4797 = CIRCLE ( 'NONE', #18134, 2.999999999999999556 ) ;
#4798 = CARTESIAN_POINT ( 'NONE',  ( -8.000050799999993245, 1.538656665208432806, 2.942827626578075950 ) ) ;
#4799 = CARTESIAN_POINT ( 'NONE',  ( 0.3076688720830444423, -0.9727984658975878940, 10.24120291391358251 ) ) ;
#4800 = CARTESIAN_POINT ( 'NONE',  ( -56.77795429543039774, 0.4641589773180558320, -1.049999627028684879 ) ) ;
#4802 = CARTESIAN_POINT ( 'NONE',  ( 23.03032540518177385, -21.91564990537362689, 1.226001752879403606 ) ) ;
#4801 = UNCERTAINTY_MEASURE_WITH_UNIT (LENGTH_MEASURE( 1.000000000000000082E-05 ), #20670, 'distance_accuracy_value', 'NONE');
#4803 = AXIS2_PLACEMENT_3D ( 'NONE', #27803, #9924, #25316 ) ;
#4804 = ORIENTED_EDGE ( 'NONE', *, *, #854, .F. ) ;
#4805 = CARTESIAN_POINT ( 'NONE',  ( -7.112550801365592257, 3.675193018007247403, -1.088641768524161391 ) ) ;
#4806 = EDGE_LOOP ( 'NONE', ( #17638, #29586, #25669 ) ) ;
#4807 = CARTESIAN_POINT ( 'NONE',  ( -6.804531657079157192, 2.325406398514293205, -1.883076972206379374 ) ) ;
#4808 = VECTOR ( 'NONE', #8412, 1000.000000000000227 ) ;
#4809 = DIRECTION ( 'NONE',  ( 0.04852105321274372690, -0.4695180821586373288, -0.8815886103626799919 ) ) ;
#4810 = CARTESIAN_POINT ( 'NONE',  ( 5.377543748152548986, -5.151476664237435443, -6.139290821770307716 ) ) ;
#4811 = CARTESIAN_POINT ( 'NONE',  ( 0.4080279096648676274, -4.540264344697044763, 1.766711686091106959 ) ) ;
#4812 = DIRECTION ( 'NONE',  ( -1.000000000000000000, 0.000000000000000000, 0.000000000000000000 ) ) ;
#4813 = ORIENTED_EDGE ( 'NONE', *, *, #2182, .F. ) ;
#4814 = CARTESIAN_POINT ( 'NONE',  ( 0.000000000000000000, -4.147285340411824173, 5.698247474649390298 ) ) ;
#4815 = EDGE_LOOP ( 'NONE', ( #20785, #31518, #28810, #10230 ) ) ;
#4816 = CARTESIAN_POINT ( 'NONE',  ( 5.489343806296447248, 1.512045527216204110, 7.976812024616029895 ) ) ;
#4817 = COORDINATED_UNIVERSAL_TIME_OFFSET ( 0, 0, .AHEAD. ) ;
#4818 = CARTESIAN_POINT ( 'NONE',  ( 85.03555310018248292, -5.200489395553704597, 3.999772873871539680 ) ) ;
#4819 = CIRCLE ( 'NONE', #25097, 10.94895958125474245 ) ;
#4820 = EDGE_CURVE ( 'NONE', #22329, #7687, #21957, .T. ) ;
#4821 = CARTESIAN_POINT ( 'NONE',  ( 18.97846294920850241, -3.417963736839119360, -1.868788737059456029 ) ) ;
#4823 = DIRECTION ( 'NONE',  ( -1.000000000000000000, 0.000000000000000000, 0.000000000000000000 ) ) ;
#4822 = CARTESIAN_POINT ( 'NONE',  ( 0.5704035945090664139, -9.255216539914215446, -2.319683995708284652 ) ) ;
#4824 = B_SPLINE_CURVE_WITH_KNOTS ( 'NONE', 3,
 ( #25922, #15365, #28590, #25571, #18051, #492, #3352, #23548 ),
 .UNSPECIFIED., .F., .F.,
 ( 4, 2, 2, 4 ),
 ( 2.049880227661072699E-07, 0.001261138121172437291, 0.001891604687747272832, 0.002522071254322108373 ),
 .UNSPECIFIED. ) ;
#4825 = VERTEX_POINT ( 'NONE', #404 ) ;
#4826 = LINE ( 'NONE', #14841, #731 ) ;
#4827 = CARTESIAN_POINT ( 'NONE',  ( -7.998722633285748174, -2.371517779863575370, 1.837526800715260533 ) ) ;
#4828 = CARTESIAN_POINT ( 'NONE',  ( 22.79750000136559862, 2.363507492473148286, 1.913930629741525058 ) ) ;
#4829 = CARTESIAN_POINT ( 'NONE',  ( 15.94387883179147281, -16.27117267478923424, -1.500000000000139222 ) ) ;
#4830 = CIRCLE ( 'NONE', #29378, 4.000000000000000000 ) ;
#4832 = VERTEX_POINT ( 'NONE', #10255 ) ;
#4831 = CARTESIAN_POINT ( 'NONE',  ( 109.5084093630373729, -17.21855534384546971, 4.522129901861157819 ) ) ;
#4833 = CARTESIAN_POINT ( 'NONE',  ( -4.087550801365593678, 2.752080473201636845, -2.228590825266444142 ) ) ;
#4834 = CARTESIAN_POINT ( 'NONE',  ( -12.44989959798873791, 20.00000000000000000, -12.99999999999999645 ) ) ;
#4835 = EDGE_CURVE ( 'NONE', #12982, #8819, #26245, .T. ) ;
#4836 = CARTESIAN_POINT ( 'NONE',  ( 5.612974441954674099, -6.420536856479970744, 5.126870824538740656 ) ) ;
#4837 = FACE_BOUND ( 'NONE', #26089, .T. ) ;
#4838 = EDGE_LOOP ( 'NONE', ( #32322, #1187, #17155 ) ) ;
#4840 = VERTEX_POINT ( 'NONE', #15603 ) ;
#4839 = CARTESIAN_POINT ( 'NONE',  ( 24.30482536760843715, -17.42173634883311095, 1.458717893414389177 ) ) ;
#4841 = CARTESIAN_POINT ( 'NONE',  ( -4.013969549054180728E-16, -4.681538312723511730, -0.8254815157535732029 ) ) ;
#4842 = FACE_OUTER_BOUND ( 'NONE', #22849, .T. ) ;
#4843 = AXIS2_PLACEMENT_3D ( 'NONE', #8037, #10397, #5562 ) ;
#4844 = EDGE_CURVE ( 'NONE', #16537, #8026, #13553, .T. ) ;
#4845 = LINE ( 'NONE', #20578, #19392 ) ;
#4846 = AXIS2_PLACEMENT_3D ( 'NONE', #25052, #2360, #5181 ) ;
#4847 = CARTESIAN_POINT ( 'NONE',  ( -24.38478530838886371, 4.195786794270493836, 1.500000000001213474 ) ) ;
#4848 = CARTESIAN_POINT ( 'NONE',  ( -1.597341074173299846, -13.32274319403951601, -1.744099774574995987 ) ) ;
#4849 = FACE_OUTER_BOUND ( 'NONE', #24306, .T. ) ;
#4850 = AXIS2_PLACEMENT_3D ( 'NONE', #6559, #11724, #24778 ) ;
#4851 = EDGE_CURVE ( 'NONE', #15111, #10785, #16076, .T. ) ;
#4852 = DIRECTION ( 'NONE',  ( -1.000000000000000000, -0.000000000000000000, -0.000000000000000000 ) ) ;
#4853 = CARTESIAN_POINT ( 'NONE',  ( 18.58227844715246135, -7.846511338401735536, 2.713652344655544724 ) ) ;
#4854 = ORIENTED_EDGE ( 'NONE', *, *, #16281, .T. ) ;
#4855 = DIRECTION ( 'NONE',  ( -0.1027947991993878041, 0.9947025833170222153, 0.000000000000000000 ) ) ;
#4856 = AXIS2_PLACEMENT_3D ( 'NONE', #25974, #1214, #8399 ) ;
#4857 = EDGE_CURVE ( 'NONE', #10930, #15521, #14475, .T. ) ;
#4858 = PERSON_AND_ORGANIZATION ( #6766, #25292 ) ;
#4859 = CARTESIAN_POINT ( 'NONE',  ( 10.00000000000000000, -3.993798362933289159, -3.024842911000733547 ) ) ;
#4860 = ORIENTED_EDGE ( 'NONE', *, *, #11126, .T. ) ;
#4861 = CARTESIAN_POINT ( 'NONE',  ( 108.0732742559233515, 18.58617989449696140, -4.624430632823066212 ) ) ;
#4862 = VERTEX_POINT ( 'NONE', #25631 ) ;
#4863 = CARTESIAN_POINT ( 'NONE',  ( -17.11836807087407664, 9.444159879341990305, 1.999016699742306891 ) ) ;
#4865 = ORIENTED_EDGE ( 'NONE', *, *, #31653, .F. ) ;
#4864 = CARTESIAN_POINT ( 'NONE',  ( 84.96769306194079263, -4.093459866477664910, -4.043899880962059434 ) ) ;
#4866 = AXIS2_PLACEMENT_3D ( 'NONE', #21984, #11779, #29690 ) ;
#4867 = ORIENTED_EDGE ( 'NONE', *, *, #178, .T. ) ;
#4868 = EDGE_CURVE ( 'NONE', #12161, #20071, #2746, .T. ) ;
#4869 = CIRCLE ( 'NONE', #22480, 5.010000000000000675 ) ;
#4870 = EDGE_CURVE ( 'NONE', #27483, #20748, #10925, .T. ) ;
#4871 = DIRECTION ( 'NONE',  ( -1.000000000000000000, 0.000000000000000000, 0.000000000000000000 ) ) ;
#4872 = PLANE ( 'NONE',  #28873 ) ;
#4873 = VECTOR ( 'NONE', #16496, 1000.000000000000000 ) ;
#4874 = CARTESIAN_POINT ( 'NONE',  ( 2.619932554246601438E-16, 3.055657119358849982, -3.641590349731898879 ) ) ;
#4875 = VECTOR ( 'NONE', #9633, 1000.000000000000227 ) ;
#4876 = CARTESIAN_POINT ( 'NONE',  ( -61.56966150227469114, -10.96966150227468972, 1.000000000000000000 ) ) ;
#4878 = ORIENTED_EDGE ( 'NONE', *, *, #13433, .T. ) ;
#4877 = CARTESIAN_POINT ( 'NONE',  ( 0.7212197917577920503, 4.829101774917357481, 7.537903528354168436 ) ) ;
#4879 = DIRECTION ( 'NONE',  ( 6.938893903907222067E-15, 1.000000000000000000, 0.000000000000000000 ) ) ;
#4880 = VECTOR ( 'NONE', #16871, 1000.000000000000000 ) ;
#4881 = CARTESIAN_POINT ( 'NONE',  ( 3.541509388326462116, -13.88765124358084968, 4.522129901861156931 ) ) ;
#4882 = CARTESIAN_POINT ( 'NONE',  ( 6.530491627857223591, -3.540416224243723597, 7.903708701126678449 ) ) ;
#4883 = CARTESIAN_POINT ( 'NONE',  ( 7.278212736155910356, -5.482579125107631235, -1.500000000000000000 ) ) ;
#4885 = ORIENTED_EDGE ( 'NONE', *, *, #11774, .F. ) ;
#4884 = CARTESIAN_POINT ( 'NONE',  ( 2.274274201625327230, 0.000000000000000000, 0.000000000000000000 ) ) ;
#4886 = DIRECTION ( 'NONE',  ( 1.000000000000000000, 0.000000000000000000, 0.000000000000000000 ) ) ;
#4887 = AXIS2_PLACEMENT_3D ( 'NONE', #29401, #24230, #14182 ) ;
#4888 = CARTESIAN_POINT ( 'NONE',  ( 5.612974259723586101, -2.621729824970331357, -7.786824029658790280 ) ) ;
#4889 = CARTESIAN_POINT ( 'NONE',  ( 23.67250000136559507, 2.363507492473148286, 1.913930629741525058 ) ) ;
#4890 = CYLINDRICAL_SURFACE ( 'NONE', #4952, 4.000000000000001776 ) ;
#4891 = EDGE_CURVE ( 'NONE', #11796, #22238, #10772, .T. ) ;
#4892 = B_SPLINE_CURVE_WITH_KNOTS ( 'NONE', 3,
 ( #31002, #18462, #2591, #25992, #23454, #23311, #8269, #7775, #10753, #10439, #10591, #28311, #18290 ),
 .UNSPECIFIED., .F., .F.,
 ( 4, 3, 3, 3, 4 ),
 ( 1.301042606982605321E-18, 0.0005743798323162931140, 0.001512856554034470568, 0.002920571641052362513, 0.003274063357800027687 ),
 .UNSPECIFIED. ) ;
#4893 = CARTESIAN_POINT ( 'NONE',  ( 6.880159396099836400, 7.192972099401698571, -4.949130873693301957 ) ) ;
#4894 = FACE_OUTER_BOUND ( 'NONE', #33069, .T. ) ;
#4895 = ORIENTED_EDGE ( 'NONE', *, *, #9647, .F. ) ;
#4896 = DIRECTION ( 'NONE',  ( -1.000000000000000000, 0.000000000000000000, 0.000000000000000000 ) ) ;
#4897 = CARTESIAN_POINT ( 'NONE',  ( 7.249760686538667009, 1.391664247347228045, 7.892520144992438702 ) ) ;
#4898 = CARTESIAN_POINT ( 'NONE',  ( -6.987550801365594033, -0.3701630799359326152, 3.521866450007987037 ) ) ;
#4899 = ORIENTED_EDGE ( 'NONE', *, *, #4106, .T. ) ;
#4900 = AXIS2_PLACEMENT_3D ( 'NONE', #23685, #23836, #26376 ) ;
#4901 = AXIS2_PLACEMENT_3D ( 'NONE', #4935, #27504, #32694 ) ;
#4902 =( BOUNDED_CURVE ( )  B_SPLINE_CURVE ( 2, ( #7136, #27525, #14800, #14456, #19670, #1458, #24846, #29862, #22332, #1611, #16977 ),
 .UNSPECIFIED., .F., .F. ) 
 B_SPLINE_CURVE_WITH_KNOTS ( ( 3, 2, 2, 2, 2, 3 ),
 ( 0.8728822619934377691, 0.8750000000000000000, 0.8906250000000000000, 0.9062500000000000000, 0.9218750000000000000, 0.9353822619934377691 ),
 .UNSPECIFIED. ) 
 CURVE ( )  GEOMETRIC_REPRESENTATION_ITEM ( )  RATIONAL_B_SPLINE_CURVE ( ( 0.9821626249036861100, 0.9896829947469995004, 1.000000000000000000, 0.9238795325112867385, 1.000000000000000000, 0.9238795325112867385, 1.000000000000000000, 0.9238795325112867385, 1.000000000000000000, 0.9341965377642872381, 0.9821626249036861100 ) ) 
 REPRESENTATION_ITEM ( '' )  );
#4903 = AXIS2_PLACEMENT_3D ( 'NONE', #31334, #28980, #16266 ) ;
#4904 = DIRECTION ( 'NONE',  ( 1.000000000000000000, 0.000000000000000000, 0.000000000000000000 ) ) ;
#4905 = DIRECTION ( 'NONE',  ( -1.000000000000000000, 8.574039729943018344E-17, -0.000000000000000000 ) ) ;
#4906 = CARTESIAN_POINT ( 'NONE',  ( 3.090086839177710321, 0.04810462266637633572, -0.6765469099969410038 ) ) ;
#4907 = ORIENTED_EDGE ( 'NONE', *, *, #22837, .F. ) ;
#4909 = CARTESIAN_POINT ( 'NONE',  ( 108.0068349480237515, 18.21621961241920573, -4.398253369385427547 ) ) ;
#4908 = AXIS2_PLACEMENT_3D ( 'NONE', #9371, #19581, #6856 ) ;
#4910 = EDGE_CURVE ( 'NONE', #15944, #31503, #7577, .T. ) ;
#4911 = ORIENTED_EDGE ( 'NONE', *, *, #18960, .T. ) ;
#4912 = VECTOR ( 'NONE', #28066, 1000.000000000000000 ) ;
#4913 = VECTOR ( 'NONE', #23708, 1000.000000000000114 ) ;
#4914 = PLANE ( 'NONE',  #20325 ) ;
#4915 = EDGE_LOOP ( 'NONE', ( #10887, #12325, #28221, #29751, #29239, #2822, #4919, #15962, #3459, #10361 ) ) ;
#4916 = LINE ( 'NONE', #14408, #18792 ) ;
#4918 = EDGE_LOOP ( 'NONE', ( #25985, #9610, #14730, #18902 ) ) ;
#4917 = FACE_OUTER_BOUND ( 'NONE', #24499, .T. ) ;
#4919 = ORIENTED_EDGE ( 'NONE', *, *, #23946, .T. ) ;
#4920 = DIRECTION ( 'NONE',  ( 0.000000000000000000, 0.000000000000000000, 1.000000000000000000 ) ) ;
#4921 = EDGE_CURVE ( 'NONE', #31196, #16940, #5595, .T. ) ;
#4922 = ADVANCED_FACE ( 'NONE', ( #26471 ), #550, .T. ) ;
#4923 = ORIENTED_EDGE ( 'NONE', *, *, #22535, .F. ) ;
#4924 = PLANE ( 'NONE',  #30084 ) ;
#4926 = ORIENTED_EDGE ( 'NONE', *, *, #27007, .T. ) ;
#4925 = LINE ( 'NONE', #23148, #28853 ) ;
#4927 = CIRCLE ( 'NONE', #17723, 4.999999999999998224 ) ;
#4928 = CARTESIAN_POINT ( 'NONE',  ( 2.865321775463968379, -11.57729440622175154, -1.759700797516209114 ) ) ;
#4929 = AXIS2_PLACEMENT_3D ( 'NONE', #5678, #11016, #15859 ) ;
#4930 = CARTESIAN_POINT ( 'NONE',  ( 41.43709133142961321, -4.769546740945156849, -4.522129901861162260 ) ) ;
#4931 = AXIS2_PLACEMENT_3D ( 'NONE', #3736, #13901, #11431 ) ;
#4932 = AXIS2_PLACEMENT_3D ( 'NONE', #21106, #20614, #17755 ) ;
#4933 = TOROIDAL_SURFACE ( 'NONE', #25739, 6.923700951379999857, 9.000000000000001776 ) ;
#4934 = CARTESIAN_POINT ( 'NONE',  ( 6.883866357751288412, 8.704251636488463006, 0.6899766464187978565 ) ) ;
#4935 = CARTESIAN_POINT ( 'NONE',  ( 3.249999999999999556, 4.472189673936902032, -8.264486777890061475 ) ) ;
#4936 = CARTESIAN_POINT ( 'NONE',  ( 25.16500339546638187, -17.49275296966148474, 1.172809483626021665 ) ) ;
#4937 = VECTOR ( 'NONE', #1376, 1000.000000000000000 ) ;
#4938 = EDGE_CURVE ( 'NONE', #32336, #264, #1714, .T. ) ;
#4939 = CARTESIAN_POINT ( 'NONE',  ( -1.331261126401621420, -14.27417440010058414, 0.9788672205877712029 ) ) ;
#4940 = DIRECTION ( 'NONE',  ( 0.000000000000000000, 0.000000000000000000, -1.000000000000000000 ) ) ;
#4941 = CC_DESIGN_PERSON_AND_ORGANIZATION_ASSIGNMENT ( #27355, #12134, ( #4694 ) ) ;
#4942 = CARTESIAN_POINT ( 'NONE',  ( 0.000000000000000000, 0.000000000000000000, 0.000000000000000000 ) ) ;
#4943 = CARTESIAN_POINT ( 'NONE',  ( 68.56906952848913761, -3.255983411058661847, 0.07017451550800900273 ) ) ;
#4944 = DIRECTION ( 'NONE',  ( 0.000000000000000000, -0.9945218953682742891, 0.1045284632676437286 ) ) ;
#4945 = CARTESIAN_POINT ( 'NONE',  ( -4.250050802731187183, 1.887961173149511618, 2.331437884370912705 ) ) ;
#4946 = EDGE_LOOP ( 'NONE', ( #13574, #19189, #28106, #26641 ) ) ;
#4947 = CARTESIAN_POINT ( 'NONE',  ( -5.037550801365593856, -1.088641768524163389, -3.675193018007246071 ) ) ;
#4948 = CIRCLE ( 'NONE', #30062, 8.749000000000002331 ) ;
#4949 = VECTOR ( 'NONE', #671, 1000.000000000000227 ) ;
#4950 = CARTESIAN_POINT ( 'NONE',  ( 23.21956271100826541, -21.93898037844929760, -1.019911551275596517 ) ) ;
#4951 = DIRECTION ( 'NONE',  ( 1.000000000000000000, 0.000000000000000000, 0.000000000000000000 ) ) ;
#4953 = ORIENTED_EDGE ( 'NONE', *, *, #26490, .F. ) ;
#4952 = AXIS2_PLACEMENT_3D ( 'NONE', #17759, #236, #10717 ) ;
#4954 = DIRECTION ( 'NONE',  ( -0.1327696077594705815, 0.9911469271785068313, 0.000000000000000000 ) ) ;
#4955 = CARTESIAN_POINT ( 'NONE',  ( 3.063284526839890720, 6.772677083992379110, 5.538577986808916442 ) ) ;
#4956 = EDGE_CURVE ( 'NONE', #19712, #11907, #794, .T. ) ;
#4957 = VECTOR ( 'NONE', #3173, 1000.000000000000000 ) ;
#4958 = VECTOR ( 'NONE', #8904, 1000.000000000000114 ) ;
#4959 = VERTEX_POINT ( 'NONE', #18763 ) ;
#4960 = CARTESIAN_POINT ( 'NONE',  ( 101.8016823592329274, -4.042758964359259188, -3.993434276136486716 ) ) ;
#4961 = VECTOR ( 'NONE', #5817, 1000.000000000000000 ) ;
#4963 = ORIENTED_EDGE ( 'NONE', *, *, #19908, .T. ) ;
#4962 = CARTESIAN_POINT ( 'NONE',  ( 68.79832465278998654, -7.861404707920828905, 0.07017451552781736601 ) ) ;
#4964 = ORIENTED_EDGE ( 'NONE', *, *, #15500, .T. ) ;
#4965 = CYLINDRICAL_SURFACE ( 'NONE', #13916, 3.000000000000000444 ) ;
#4966 = AXIS2_PLACEMENT_3D ( 'NONE', #32471, #27606, #4381 ) ;
#4967 = ORIENTED_EDGE ( 'NONE', *, *, #15895, .T. ) ;
#4968 = CYLINDRICAL_SURFACE ( 'NONE', #32610, 4.000000000000001776 ) ;
#4970 = VERTEX_POINT ( 'NONE', #31815 ) ;
#4969 = CARTESIAN_POINT ( 'NONE',  ( 0.6728001045953906356, -8.512517952473988458, -3.357496170320755091 ) ) ;
#4971 = DIRECTION ( 'NONE',  ( -8.541412920197207489E-17, -0.9961946980917444350, -0.08715574274767159957 ) ) ;
#4972 = FACE_OUTER_BOUND ( 'NONE', #31095, .T. ) ;
#4973 = B_SPLINE_CURVE_WITH_KNOTS ( 'NONE', 3,
 ( #18038, #21357, #15514, #13503, #5982, #28576, #7845, #23716, #2857, #26061, #3163, #337, #20722 ),
 .UNSPECIFIED., .F., .F.,
 ( 4, 3, 3, 3, 4 ),
 ( 8.673617379884034509E-19, 0.0008924055619933561265, 0.001784811123946879966, 0.002677216685860944918, 0.003343752506362699349 ),
 .UNSPECIFIED. ) ;
#4974 = CARTESIAN_POINT ( 'NONE',  ( 107.6641581766430278, -20.45810077038846586, 1.500000000000000000 ) ) ;
#4975 = DIRECTION ( 'NONE',  ( 0.000000000000000000, 0.08715574274766134388, -0.9961946980917452121 ) ) ;
#4976 = ORIENTED_EDGE ( 'NONE', *, *, #12245, .T. ) ;
#4977 = CIRCLE ( 'NONE', #27400, 10.96966150227469328 ) ;
#4978 = LINE ( 'NONE', #4794, #9079 ) ;
#4979 = DIRECTION ( 'NONE',  ( 0.000000000000000000, 0.4226182617406968878, 0.9063077870366511579 ) ) ;
#4980 = LINE ( 'NONE', #23008, #4355 ) ;
#4981 = DIRECTION ( 'NONE',  ( 0.000000000000000000, -0.9271838545667856479, -0.3746065934159162891 ) ) ;
#4982 = CIRCLE ( 'NONE', #28463, 4.000000000000001776 ) ;
#4983 = ADVANCED_FACE ( 'NONE', ( #13577 ), #15853, .T. ) ;
#4984 = AXIS2_PLACEMENT_3D ( 'NONE', #11667, #16507, #11174 ) ;
#4985 = VECTOR ( 'NONE', #10184, 1000.000000000000000 ) ;
#4986 = CARTESIAN_POINT ( 'NONE',  ( 5.612717990268491164, 0.1993707932846012776, 8.213645783354285967 ) ) ;
#4987 = CARTESIAN_POINT ( 'NONE',  ( 0.000000000000000000, 0.000000000000000000, 0.000000000000000000 ) ) ;
#4988 = CARTESIAN_POINT ( 'NONE',  ( -56.69596708151924247, 0.1891862907730448851, -1.417079347435143966 ) ) ;
#4989 = CARTESIAN_POINT ( 'NONE',  ( 23.24965750580003387, -21.93932300456764395, 1.000000000000000000 ) ) ;
#4990 = ORIENTED_EDGE ( 'NONE', *, *, #28175, .F. ) ;
#4991 = CARTESIAN_POINT ( 'NONE',  ( -7.162550801365593856, 2.752080473201636845, -2.228590825266444142 ) ) ;
#4992 = ORIENTED_EDGE ( 'NONE', *, *, #26574, .F. ) ;
#4993 = CARTESIAN_POINT ( 'NONE',  ( -8.204531657079158435, 1.883076972206379374, 2.325406398514293205 ) ) ;
#4994 = CARTESIAN_POINT ( 'NONE',  ( 21.61000000136559507, 2.892927487894327410, -1.570731468192931635 ) ) ;
#4995 = CARTESIAN_POINT ( 'NONE',  ( 108.1300413742128796, -20.08325238768393461, 1.420916680473288896 ) ) ;
#4996 = CARTESIAN_POINT ( 'NONE',  ( 69.38611993481310947, -8.080330187063884395, -2.713652344655543391 ) ) ;
#4997 = DIRECTION ( 'NONE',  ( -1.000000000000000000, 0.000000000000000000, -0.000000000000000000 ) ) ;
#4998 = ORIENTED_EDGE ( 'NONE', *, *, #18380, .F. ) ;
#4999 = EDGE_CURVE ( 'NONE', #15334, #25541, #3088, .T. ) ;
#5000 = CARTESIAN_POINT ( 'NONE',  ( 4.104821569165022408E-16, 4.787500056513387392, -1.476463073999588538 ) ) ;
#5001 = EDGE_CURVE ( 'NONE', #17100, #6901, #29461, .T. ) ;
#5002 = AXIS2_PLACEMENT_3D ( 'NONE', #18115, #76, #28004 ) ;
#5003 = LINE ( 'NONE', #15186, #15453 ) ;
#5004 = ORIENTED_EDGE ( 'NONE', *, *, #12814, .F. ) ;
#5005 = DIRECTION ( 'NONE',  ( -1.000000000000000000, 0.000000000000000000, 0.000000000000000000 ) ) ;
#5006 = EDGE_CURVE ( 'NONE', #5447, #30423, #21275, .T. ) ;
#5008 = VECTOR ( 'NONE', #8875, 1000.000000000000000 ) ;
#5007 = APPROVAL_DATE_TIME ( #7985, #19229 ) ;
#5009 = CARTESIAN_POINT ( 'NONE',  ( 28.66858063836256676, -6.589466490307128943, 4.185347664752067764 ) ) ;
#5010 = VECTOR ( 'NONE', #28207, 1000.000000000000114 ) ;
#5011 = CIRCLE ( 'NONE', #31717, 0.5000000000000004441 ) ;
#5012 = CIRCLE ( 'NONE', #27874, 8.500000000000000000 ) ;
#5013 = DIRECTION ( 'NONE',  ( 0.000000000000000000, 0.000000000000000000, 1.000000000000000000 ) ) ;
#5015 = CARTESIAN_POINT ( 'NONE',  ( 6.356381451270080696, -0.5733789922930644378, -8.587653982362821736 ) ) ;
#5014 = CARTESIAN_POINT ( 'NONE',  ( 0.6791197550704926034, -8.860977624947322440, -2.303133748654038193 ) ) ;
#5016 = ORIENTED_EDGE ( 'NONE', *, *, #25752, .T. ) ;
#5017 = PRODUCT_DEFINITION_FORMATION_WITH_SPECIFIED_SOURCE ( 'ANY', '', #5241, .NOT_KNOWN. ) ;
#5018 = CARTESIAN_POINT ( 'NONE',  ( -8.000050800000000351, -2.415348148595104938, -1.802067931085318930 ) ) ;
#5019 = FACE_OUTER_BOUND ( 'NONE', #9252, .T. ) ;
#5020 = CARTESIAN_POINT ( 'NONE',  ( 24.54750000136559507, 1.913930629741522838, -2.363507492473150062 ) ) ;
#5021 = LINE ( 'NONE', #30773, #21981 ) ;
#5023 = ORIENTED_EDGE ( 'NONE', *, *, #5122, .F. ) ;
#5022 = CARTESIAN_POINT ( 'NONE',  ( 40.91321928711098366, -19.30714377376088464, 0.9788672205888330202 ) ) ;
#5024 = CARTESIAN_POINT ( 'NONE',  ( -7.162550801365593856, 2.752080473201636845, -2.228590825266444142 ) ) ;
#5025 = CARTESIAN_POINT ( 'NONE',  ( 10.00000000000000178, -8.574039729943018837E-16, 0.000000000000000000 ) ) ;
#5026 = CARTESIAN_POINT ( 'NONE',  ( 10.52034268205830259, 3.993798362933308255, 3.024842911000705570 ) ) ;
#5027 = DIRECTION ( 'NONE',  ( 8.281886410780493770E-17, 0.9659258262890664248, 0.2588190451025276784 ) ) ;
#5028 = ORIENTED_EDGE ( 'NONE', *, *, #24682, .F. ) ;
#5030 = ORIENTED_EDGE ( 'NONE', *, *, #20956, .T. ) ;
#5029 = CARTESIAN_POINT ( 'NONE',  ( 24.27681693764444049, -17.38739216502004226, 1.394420419282020207 ) ) ;
#5031 = VECTOR ( 'NONE', #14967, 1000.000000000000000 ) ;
#5032 = CARTESIAN_POINT ( 'NONE',  ( 13.41780342409107973, 19.07609913100965571, -4.612695725900421984 ) ) ;
#5033 = CARTESIAN_POINT ( 'NONE',  ( 0.3749742512055983523, 5.190538276686016417, -8.659825570211875601 ) ) ;
#5034 = AXIS2_PLACEMENT_3D ( 'NONE', #9061, #22291, #19778 ) ;
#5035 = CARTESIAN_POINT ( 'NONE',  ( 22.61000000136559507, 2.892927487894327410, -1.570731468192931635 ) ) ;
#5036 = CARTESIAN_POINT ( 'NONE',  ( -25.27811764180047760, 4.185543752813269514, 2.140960162089065033 ) ) ;
#5037 = CARTESIAN_POINT ( 'NONE',  ( 10.25023147436447069, -19.98140232867044830, -1.499999999999998668 ) ) ;
#5038 = ADVANCED_FACE ( 'NONE', ( #31473 ), #23932, .T. ) ;
#5039 = CARTESIAN_POINT ( 'NONE',  ( -2.794738735352966685, 0.000000000000000000, 1.508259000770582059 ) ) ;
#5040 = APPROVAL_PERSON_ORGANIZATION ( #15689, #29663, #11316 ) ;
#5041 = CARTESIAN_POINT ( 'NONE',  ( -1.762942409646513164, -5.022711880624455567E-15, 2.999999999999999556 ) ) ;
#5042 = CARTESIAN_POINT ( 'NONE',  ( 25.75999999999999801, -2.208672634433321348E-15, 0.000000000000000000 ) ) ;
#5043 = ORIENTED_EDGE ( 'NONE', *, *, #10053, .F. ) ;
#5044 = CARTESIAN_POINT ( 'NONE',  ( 0.1255855353732055757, -9.314797388894898944, 5.239665997526856245 ) ) ;
#5045 = APPLICATION_PROTOCOL_DEFINITION ( 'international standard', 'config_control_design', 1994, #28512 ) ;
#5046 = CARTESIAN_POINT ( 'NONE',  ( -18.30155664144426453, 0.000000000000000000, 0.000000000000000000 ) ) ;
#5047 = ORIENTED_EDGE ( 'NONE', *, *, #30913, .T. ) ;
#5048 = CIRCLE ( 'NONE', #21597, 5.010000000000000675 ) ;
#5049 = VERTEX_POINT ( 'NONE', #15918 ) ;
#5050 = CARTESIAN_POINT ( 'NONE',  ( -22.63903668291242610, 18.41081583916481534, 1.774234584568461726 ) ) ;
#5052 = EDGE_LOOP ( 'NONE', ( #152, #7642, #15647, #25000 ) ) ;
#5051 = CARTESIAN_POINT ( 'NONE',  ( 18.85937633404960678, -4.749113090755953337, -4.013697994455524665 ) ) ;
#5053 = ORIENTED_EDGE ( 'NONE', *, *, #23741, .T. ) ;
#5054 = CARTESIAN_POINT ( 'NONE',  ( -0.1366093623685602776, -14.96249823008941604, 1.500000000000000000 ) ) ;
#5055 = CARTESIAN_POINT ( 'NONE',  ( -6.462550801365593678, 0.3701630799359330593, -3.521866450007987037 ) ) ;
#5056 = CARTESIAN_POINT ( 'NONE',  ( 12.44989959798868817, 18.00000000000000355, 13.00000000000004441 ) ) ;
#5057 = CARTESIAN_POINT ( 'NONE',  ( 107.6023762549644687, -19.56795552613751354, -3.324358428442364843 ) ) ;
#5059 = ORIENTED_EDGE ( 'NONE', *, *, #23, .T. ) ;
#5058 = CYLINDRICAL_SURFACE ( 'NONE', #29935, 0.4500000000000025646 ) ;
#5060 = DIRECTION ( 'NONE',  ( 0.000000000000000000, -0.5877852522924804646, 0.8090169943749422332 ) ) ;
#5061 = CYLINDRICAL_SURFACE ( 'NONE', #18724, 3.499999999999999556 ) ;
#5062 = CARTESIAN_POINT ( 'NONE',  ( 2.226738579662389306, -16.57423758818535475, 1.500000000000000444 ) ) ;
#5063 = CC_DESIGN_SECURITY_CLASSIFICATION ( #16786, ( #33098 ) ) ;
#5064 = CARTESIAN_POINT ( 'NONE',  ( 8.305304941487758441, -2.146676032726119399, -1.500000000000000000 ) ) ;
#5066 = EDGE_LOOP ( 'NONE', ( #20249, #27638, #30882, #1150, #9852, #7439, #12246 ) ) ;
#5065 = CARTESIAN_POINT ( 'NONE',  ( 108.0293225756549731, -18.49159991151093863, -4.319987168239894260 ) ) ;
#5067 = CARTESIAN_POINT ( 'NONE',  ( 2.274274201625327230, -9.915734732513254102, 4.762163868918234400 ) ) ;
#5068 = EDGE_CURVE ( 'NONE', #469, #30909, #15596, .T. ) ;
#5069 = CARTESIAN_POINT ( 'NONE',  ( 107.3477315916820913, -15.88627780335592732, 1.500000000000000000 ) ) ;
#5070 = CARTESIAN_POINT ( 'NONE',  ( 21.17250000136559507, -2.363507492473152283, -1.913930629741525280 ) ) ;
#5071 = DIRECTION ( 'NONE',  ( 0.000000000000000000, 1.000000000000000000, 0.000000000000000000 ) ) ;
#5072 = CARTESIAN_POINT ( 'NONE',  ( 7.064423659272770273, 7.199384779417568048, -4.973063321325217778 ) ) ;
#5073 = CARTESIAN_POINT ( 'NONE',  ( -3.082813266615065828, -0.4373090928651341414, -1.500000000000000222 ) ) ;
#5074 = CIRCLE ( 'NONE', #25911, 2.999999999999999112 ) ;
#5075 = VERTEX_POINT ( 'NONE', #25223 ) ;
#5076 = CARTESIAN_POINT ( 'NONE',  ( -5.533288710217214579, 0.000000000000000000, -5.777777777777776791 ) ) ;
#5077 = EDGE_CURVE ( 'NONE', #15820, #28329, #27334, .T. ) ;
#5078 = DIRECTION ( 'NONE',  ( 0.000000000000000000, -0.000000000000000000, -1.000000000000000000 ) ) ;
#5079 = CARTESIAN_POINT ( 'NONE',  ( -6.337550801365593678, 3.368539882008727115, 1.828967928396027176 ) ) ;
#5080 = ORIENTED_EDGE ( 'NONE', *, *, #12575, .T. ) ;
#5081 = DIRECTION ( 'NONE',  ( 0.000000000000000000, 0.000000000000000000, 1.000000000000000000 ) ) ;
#5082 = DIRECTION ( 'NONE',  ( -1.000000000000000000, -0.000000000000000000, 0.000000000000000000 ) ) ;
#5083 = CARTESIAN_POINT ( 'NONE',  ( 6.524594682510452159, -8.636529731786344755, 0.6222547417166852668 ) ) ;
#5084 = EDGE_LOOP ( 'NONE', ( #24274, #24959, #5640, #12656 ) ) ;
#5085 = CARTESIAN_POINT ( 'NONE',  ( 15.90111129030948334, -14.71846482507236153, 1.000000000000000000 ) ) ;
#5086 = ADVANCED_FACE ( 'NONE', ( #12176 ), #26777, .F. ) ;
#5087 = ORIENTED_EDGE ( 'NONE', *, *, #29999, .T. ) ;
#5088 = CARTESIAN_POINT ( 'NONE',  ( -47.25352234179201361, 16.22999999999998266, 1.500000000000000000 ) ) ;
#5089 = ORIENTED_EDGE ( 'NONE', *, *, #4547, .F. ) ;
#5090 = CARTESIAN_POINT ( 'NONE',  ( 107.5574907784328076, -18.92149145723228898, 4.691813801508712523 ) ) ;
#5092 = ORIENTED_EDGE ( 'NONE', *, *, #22020, .T. ) ;
#5091 = DIRECTION ( 'NONE',  ( 0.000000000000000000, 0.9961946980917455452, -0.08715574274765799934 ) ) ;
#5093 = ORIENTED_EDGE ( 'NONE', *, *, #8866, .T. ) ;
#5094 = DIRECTION ( 'NONE',  ( -1.000000000000000000, -0.000000000000000000, -0.000000000000000000 ) ) ;
#5095 = EDGE_CURVE ( 'NONE', #14743, #29348, #30105, .T. ) ;
#5096 = ORIENTED_EDGE ( 'NONE', *, *, #947, .T. ) ;
#5097 = DIRECTION ( 'NONE',  ( 0.000000000000000000, 0.9063077870366476052, 0.4226182617407045483 ) ) ;
#5099 = ORIENTED_EDGE ( 'NONE', *, *, #10708, .F. ) ;
#5098 = LINE ( 'NONE', #2945, #26722 ) ;
#5100 = CARTESIAN_POINT ( 'NONE',  ( 1.944141728803306490, -0.8659045317505551509, -1.758037889546375743 ) ) ;
#5101 = DIRECTION ( 'NONE',  ( 0.000000000000000000, 0.000000000000000000, -1.000000000000000000 ) ) ;
#5102 = CARTESIAN_POINT ( 'NONE',  ( 18.93617721851659041, -3.890633339435721982, -4.522129901861162260 ) ) ;
#5103 = CARTESIAN_POINT ( 'NONE',  ( 4.888486331236938389E-17, -10.76487093102066517, 1.999317321091457655 ) ) ;
#5104 = CARTESIAN_POINT ( 'NONE',  ( 77.65715268217998357, 26.11770293189133341, -1.491740999229417941 ) ) ;
#5105 = FACE_OUTER_BOUND ( 'NONE', #30272, .T. ) ;
#5106 = CARTESIAN_POINT ( 'NONE',  ( 0.5704039292222269353, 7.316743080999716931, -6.124150562935458453 ) ) ;
#5107 = CARTESIAN_POINT ( 'NONE',  ( 111.3844470440328251, -20.20075132222358505, 1.500000000000000000 ) ) ;
#5108 = DIRECTION ( 'NONE',  ( 0.000000000000000000, 0.000000000000000000, 1.000000000000000000 ) ) ;
#5109 = DIRECTION ( 'NONE',  ( 0.1908089953765452762, 0.000000000000000000, -0.9816271834476639757 ) ) ;
#5110 = CARTESIAN_POINT ( 'NONE',  ( 84.37491783462850492, -2.359815117480457136, -0.02339150518254430253 ) ) ;
#5111 = EDGE_CURVE ( 'NONE', #14007, #17751, #29285, .T. ) ;
#5112 = CARTESIAN_POINT ( 'NONE',  ( 69.29300722455955963, -6.224615717686389438, 5.695980980372492120 ) ) ;
#5113 = ADVANCED_FACE ( 'NONE', ( #17688 ), #27569, .T. ) ;
#5114 = DIRECTION ( 'NONE',  ( 1.000000000000000000, 0.000000000000000000, 0.000000000000000000 ) ) ;
#5115 = ORIENTED_EDGE ( 'NONE', *, *, #29562, .T. ) ;
#5116 = CARTESIAN_POINT ( 'NONE',  ( -6.287550801365593856, 2.228590825266444142, 2.752080473201636845 ) ) ;
#5117 = DIRECTION ( 'NONE',  ( 0.03487826274237706969, -0.9987827659587180662, 0.03487826274237759705 ) ) ;
#5118 = LINE ( 'NONE', #7791, #9815 ) ;
#5119 = ORIENTED_EDGE ( 'NONE', *, *, #21285, .F. ) ;
#5120 = CARTESIAN_POINT ( 'NONE',  ( 13.62547635268498780, 21.94000000000002970, -1.050000000000000044 ) ) ;
#5121 = CARTESIAN_POINT ( 'NONE',  ( 56.97280603064898941, -277.2763395528616002, 0.4463807625373348298 ) ) ;
#5122 = EDGE_CURVE ( 'NONE', #15836, #30672, #16564, .T. ) ;
#5123 = ORIENTED_EDGE ( 'NONE', *, *, #25553, .F. ) ;
#5124 = FACE_OUTER_BOUND ( 'NONE', #25683, .T. ) ;
#5125 = SHAPE_DEFINITION_REPRESENTATION ( #29774, #5606 ) ;
#5127 = ORIENTED_EDGE ( 'NONE', *, *, #16827, .F. ) ;
#5126 = CARTESIAN_POINT ( 'NONE',  ( 43.74661801760413482, -24.08792321988613594, -1.499999999999999556 ) ) ;
#5128 = EDGE_LOOP ( 'NONE', ( #29622, #11412, #25999, #26651 ) ) ;
#5129 = DIRECTION ( 'NONE',  ( 0.000000000000000000, 0.000000000000000000, -1.000000000000000000 ) ) ;
#5130 = EDGE_CURVE ( 'NONE', #4589, #25021, #12367, .T. ) ;
#5131 = ORIENTED_EDGE ( 'NONE', *, *, #13527, .T. ) ;
#5132 = CARTESIAN_POINT ( 'NONE',  ( 26.27358061090008690, 19.78731608622338101, 0.4463807625373084065 ) ) ;
#5134 = EDGE_LOOP ( 'NONE', ( #19692, #7796, #14103, #18314 ) ) ;
#5133 = LINE ( 'NONE', #9965, #6403 ) ;
#5135 = CARTESIAN_POINT ( 'NONE',  ( 23.57316428367447614, -9.051964865574914754, 1.010822989962089746 ) ) ;
#5136 = PLANE ( 'NONE',  #6363 ) ;
#5137 = B_SPLINE_CURVE_WITH_KNOTS ( 'NONE', 3,
 ( #23441, #25814, #23297, #401 ),
 .UNSPECIFIED., .F., .F.,
 ( 4, 4 ),
 ( 0.000000000000000000, 0.003022500881216829988 ),
 .UNSPECIFIED. ) ;
#5138 = CARTESIAN_POINT ( 'NONE',  ( 22.23809519008879221, -21.82720698518721747, -1.456112634554884933 ) ) ;
#5139 = DIRECTION ( 'NONE',  ( -0.000000000000000000, -0.000000000000000000, -1.000000000000000000 ) ) ;
#5140 = ORIENTED_EDGE ( 'NONE', *, *, #19783, .F. ) ;
#5141 = CARTESIAN_POINT ( 'NONE',  ( 21.29750000273119070, 2.594547506269380133, 0.7685399846772031918 ) ) ;
#5142 = CARTESIAN_POINT ( 'NONE',  ( 10.00000000000000000, 3.055657119358800244, 3.641590349731939735 ) ) ;
#5143 = FACE_OUTER_BOUND ( 'NONE', #29624, .T. ) ;
#5144 = DIRECTION ( 'NONE',  ( -0.000000000000000000, -1.000000000000000000, -0.000000000000000000 ) ) ;
#5145 = CARTESIAN_POINT ( 'NONE',  ( 24.51577259974246914, -17.45257443369953521, 1.477717642885331140 ) ) ;
#5146 = DIRECTION ( 'NONE',  ( -1.000000000000000000, 0.000000000000000000, 0.000000000000000000 ) ) ;
#5147 = SPHERICAL_SURFACE ( 'NONE', #32712, 0.5000000000000000000 ) ;
#5148 = DIRECTION ( 'NONE',  ( 1.000000000000000000, 0.000000000000000000, 0.000000000000000000 ) ) ;
#5149 = VERTEX_POINT ( 'NONE', #19889 ) ;
#5150 = B_SPLINE_CURVE_WITH_KNOTS ( 'NONE', 3,
 ( #7542, #22921, #17567, #18237, #27766, #2395, #4881, #28115, #22612, #5212, #30654, #25278, #22772, #7379, #28265, #25597 ),
 .UNSPECIFIED., .F., .F.,
 ( 4, 2, 2, 2, 2, 2, 2, 4 ),
 ( 0.009305842773634975459, 0.5000000000000000000, 0.6250000000000000000, 0.7500000000000000000, 0.8125000000000000000, 0.8750000000000000000, 0.9375000000000000000, 1.000000000000000000 ),
 .UNSPECIFIED. ) ;
#5151 = ADVANCED_FACE ( 'NONE', ( #7182 ), #12029, .F. ) ;
#5152 = CARTESIAN_POINT ( 'NONE',  ( -7.512550801365593500, -3.675193018007246071, 1.088641768524163167 ) ) ;
#5153 = EDGE_LOOP ( 'NONE', ( #17784, #28964, #21202, #17131, #11812 ) ) ;
#5154 = CARTESIAN_POINT ( 'NONE',  ( -8.400050800000000706, 2.331437884370912705, -1.887961173149511618 ) ) ;
#5155 = CARTESIAN_POINT ( 'NONE',  ( 22.73500000136559862, 3.156283516753366047, 0.9349337715887203748 ) ) ;
#5156 = CARTESIAN_POINT ( 'NONE',  ( 107.9828061044025418, 18.08241752981144046, 5.008628968642859114 ) ) ;
#5157 = CARTESIAN_POINT ( 'NONE',  ( 18.58227844715246135, -7.846511338401735536, -2.713652344655542947 ) ) ;
#5158 = CARTESIAN_POINT ( 'NONE',  ( 25.46419143546241060, -18.07592536767356250, 1.500000000000000000 ) ) ;
#5159 = ORIENTED_EDGE ( 'NONE', *, *, #25102, .F. ) ;
#5160 = CARTESIAN_POINT ( 'NONE',  ( -32.06740601709051930, -21.93932300455396600, -0.9045955023117262517 ) ) ;
#5161 = ORIENTED_EDGE ( 'NONE', *, *, #32082, .F. ) ;
#5162 = CARTESIAN_POINT ( 'NONE',  ( 5.377543748152548986, -1.391664247347174754, -7.892520144992448472 ) ) ;
#5163 = APPROVAL_DATE_TIME ( #33075, #6347 ) ;
#5164 = CARTESIAN_POINT ( 'NONE',  ( 40.88358382947309622, -6.821371083843753347, 4.093303308732203938 ) ) ;
#5165 = EDGE_CURVE ( 'NONE', #13430, #31497, #27715, .T. ) ;
#5166 = CYLINDRICAL_SURFACE ( 'NONE', #3236, 11.00000000000000000 ) ;
#5168 = DIRECTION ( 'NONE',  ( 0.000000000000000000, 0.9659258262890682012, -0.2588190451025209060 ) ) ;
#5167 = CARTESIAN_POINT ( 'NONE',  ( 108.9715489600704501, 17.93065334586892234, -5.381233285085805562 ) ) ;
#5169 = ORIENTED_EDGE ( 'NONE', *, *, #32303, .F. ) ;
#5170 = CARTESIAN_POINT ( 'NONE',  ( -8.000050799999998574, -2.808468352995062478, -1.064040931622213249 ) ) ;
#5171 = CYLINDRICAL_SURFACE ( 'NONE', #11261, 4.000000000000001776 ) ;
#5172 = CARTESIAN_POINT ( 'NONE',  ( 22.36000000136559152, -1.570731468192933633, -2.892927487894330074 ) ) ;
#5173 = FACE_OUTER_BOUND ( 'NONE', #5524, .T. ) ;
#5175 = ORIENTED_EDGE ( 'NONE', *, *, #33085, .F. ) ;
#5174 = CARTESIAN_POINT ( 'NONE',  ( 17.36028307725516484, -18.11957666780531895, 4.522129901861157819 ) ) ;
#5176 = CARTESIAN_POINT ( 'NONE',  ( -5.612550801365594033, 1.828967928396027176, -3.368539882008727115 ) ) ;
#5177 = CARTESIAN_POINT ( 'NONE',  ( -41.25971018530405843, -14.96514855415592216, 5.309652167554829383 ) ) ;
#5178 = LINE ( 'NONE', #25561, #7598 ) ;
#5179 = CARTESIAN_POINT ( 'NONE',  ( 21.92249999999999943, 2.378061970571979433, -1.291182301015470602 ) ) ;
#5180 = ORIENTED_EDGE ( 'NONE', *, *, #15298, .T. ) ;
#5182 = ORIENTED_EDGE ( 'NONE', *, *, #24672, .F. ) ;
#5181 = DIRECTION ( 'NONE',  ( -0.1767573132311711093, -0.9842544651762052954, 0.000000000000000000 ) ) ;
#5183 = EDGE_CURVE ( 'NONE', #8879, #6622, #25955, .T. ) ;
#5184 = DIRECTION ( 'NONE',  ( 1.000000000000000000, 0.000000000000000000, 0.000000000000000000 ) ) ;
#5185 = FACE_OUTER_BOUND ( 'NONE', #28644, .T. ) ;
#5186 = EDGE_CURVE ( 'NONE', #21400, #30724, #11845, .T. ) ;
#5187 = CARTESIAN_POINT ( 'NONE',  ( 21.04750000136559507, -1.913930629741527500, 2.363507492473149618 ) ) ;
#5188 = CARTESIAN_POINT ( 'NONE',  ( -29.77647832281393647, 7.339147416615578123, 1.500000000000000000 ) ) ;
#5189 = LINE ( 'NONE', #7858, #14553 ) ;
#5190 = CARTESIAN_POINT ( 'NONE',  ( 2.632061376486628301, -0.5000000000000000000, -1.500000000000000000 ) ) ;
#5191 = B_SPLINE_CURVE_WITH_KNOTS ( 'NONE', 3,
 ( #6701, #16889, #27087, #23767, #18740, #13714, #1026, #21417 ),
 .UNSPECIFIED., .F., .F.,
 ( 4, 2, 2, 4 ),
 ( 2.333100269151217215E-07, 0.001262083418509045343, 0.001893008472750110603, 0.002523933526991176297 ),
 .UNSPECIFIED. ) ;
#5192 = CARTESIAN_POINT ( 'NONE',  ( -56.33578448492038859, 0.003046479527604620090, 0.000000000000000000 ) ) ;
#5193 = DIRECTION ( 'NONE',  ( 1.000000000000000000, -0.000000000000000000, -0.000000000000000000 ) ) ;
#5194 = ORIENTED_EDGE ( 'NONE', *, *, #22020, .F. ) ;
#5195 = CARTESIAN_POINT ( 'NONE',  ( 0.000000000000000000, 0.000000000000000000, 0.000000000000000000 ) ) ;
#5196 = DATE_AND_TIME ( #12701, #27413 ) ;
#5197 = CARTESIAN_POINT ( 'NONE',  ( 84.55169161418007207, -5.233307109646406552, -3.993432236203768415 ) ) ;
#5198 = VERTEX_POINT ( 'NONE', #15005 ) ;
#5199 = CARTESIAN_POINT ( 'NONE',  ( 107.6331050892701739, 18.97529836792814706, -5.039948469649382368 ) ) ;
#5200 = ORIENTED_EDGE ( 'NONE', *, *, #29783, .F. ) ;
#5201 = CARTESIAN_POINT ( 'NONE',  ( -5.300050802731187893, 1.549418761218566143, -2.853674364686379583 ) ) ;
#5203 = ORIENTED_EDGE ( 'NONE', *, *, #17005, .F. ) ;
#5202 = CARTESIAN_POINT ( 'NONE',  ( 69.01353589305286107, -4.976445672242260976, -4.003575175710716749 ) ) ;
#5204 = VERTEX_POINT ( 'NONE', #4335 ) ;
#5205 = CARTESIAN_POINT ( 'NONE',  ( -2.600000000000000089, 0.000000000000000000, -1.500000000000000000 ) ) ;
#5206 = CARTESIAN_POINT ( 'NONE',  ( -7.562550801365593323, -2.752080473201636845, 2.228590825266444586 ) ) ;
#5207 = DIRECTION ( 'NONE',  ( 0.000000000000000000, -0.000000000000000000, 1.000000000000000000 ) ) ;
#5208 = DIRECTION ( 'NONE',  ( 0.000000000000000000, 0.000000000000000000, 1.000000000000000000 ) ) ;
#5210 = ORIENTED_EDGE ( 'NONE', *, *, #8031, .F. ) ;
#5209 = CARTESIAN_POINT ( 'NONE',  ( -42.46793790805479318, 24.51887538314362658, 1.050000000000000044 ) ) ;
#5211 = CARTESIAN_POINT ( 'NONE',  ( 11.90652295052632503, 20.12228623747235901, 4.629213727441584325 ) ) ;
#5212 = CARTESIAN_POINT ( 'NONE',  ( -0.7739934281325634435, -8.972773999336988382, 4.522129901861156931 ) ) ;
#5213 = CARTESIAN_POINT ( 'NONE',  ( -4.250518365315470781, -7.586662160519804132, 1.500000000000317746 ) ) ;
#5215 = CARTESIAN_POINT ( 'NONE',  ( 23.92250000136559507, -1.913930629741527500, 2.363507492473149618 ) ) ;
#5214 =( REPRESENTATION_RELATIONSHIP ('NONE','NONE', #1085, #3460 ) REPRESENTATION_RELATIONSHIP_WITH_TRANSFORMATION ( #3752 )SHAPE_REPRESENTATION_RELATIONSHIP( ) );
#5216 = CARTESIAN_POINT ( 'NONE',  ( 10.57125986779756843, -0.8254815157535575487, 4.681538312723514395 ) ) ;
#5217 = EDGE_CURVE ( 'NONE', #24285, #20812, #19711, .T. ) ;
#5219 = EDGE_LOOP ( 'NONE', ( #14394, #4059 ) ) ;
#5218 = CARTESIAN_POINT ( 'NONE',  ( 108.0617487723258279, -18.95852907696271927, -4.497374936780334842 ) ) ;
#5220 = DIRECTION ( 'NONE',  ( -1.000000000000000000, 0.000000000000000000, 0.000000000000000000 ) ) ;
#5221 = EDGE_CURVE ( 'NONE', #24971, #25459, #22877, .T. ) ;
#5222 = CARTESIAN_POINT ( 'NONE',  ( 2.866494652514124830, 9.241976615262203154, 2.300561732649596181 ) ) ;
#5223 = CARTESIAN_POINT ( 'NONE',  ( 21.42250000136559507, 1.913930629741522838, -2.363507492473150062 ) ) ;
#5224 = FACE_OUTER_BOUND ( 'NONE', #20476, .T. ) ;
#5225 = CARTESIAN_POINT ( 'NONE',  ( -34.48223484310472031, 0.5000000000000000000, 3.000000000000004441 ) ) ;
#5226 = CARTESIAN_POINT ( 'NONE',  ( 18.66634262892307916, -21.55284492811556873, -1.491166157331017317 ) ) ;
#5227 = ORIENTED_EDGE ( 'NONE', *, *, #18433, .T. ) ;
#5228 = CARTESIAN_POINT ( 'NONE',  ( 108.0161339826157985, -18.30168745265750729, 4.597046469859526141 ) ) ;
#5229 = FACE_OUTER_BOUND ( 'NONE', #16440, .T. ) ;
#5230 = CARTESIAN_POINT ( 'NONE',  ( -4.887550801365593500, 2.752080473201636845, -2.228590825266444142 ) ) ;
#5231 = ORIENTED_EDGE ( 'NONE', *, *, #25504, .F. ) ;
#5232 = FACE_OUTER_BOUND ( 'NONE', #3929, .T. ) ;
#5233 = DIRECTION ( 'NONE',  ( 1.000000000000000000, 0.000000000000000000, 0.000000000000000000 ) ) ;
#5234 = CARTESIAN_POINT ( 'NONE',  ( 1.828104818894226380, -1.262475772535087915, -1.500000000000000444 ) ) ;
#5235 = CARTESIAN_POINT ( 'NONE',  ( 41.45135008765516460, -9.497951668093163491, 0.07017451552781736601 ) ) ;
#5236 = EDGE_CURVE ( 'NONE', #16153, #22005, #29910, .T. ) ;
#5237 = VERTEX_POINT ( 'NONE', #22376 ) ;
#5238 = DIRECTION ( 'NONE',  ( -1.000000000000000000, 0.000000000000000000, 0.000000000000000000 ) ) ;
#5239 = ORIENTED_EDGE ( 'NONE', *, *, #19818, .T. ) ;
#5240 = CARTESIAN_POINT ( 'NONE',  ( -2.989861291979827751, -0.09348435554463166430, 1.299029471086685428 ) ) ;
#5241 = PRODUCT ( 'Part5_knurlingConnector', 'Part5_knurlingConnector', '', ( #20896 ) ) ;
#5243 = ORIENTED_EDGE ( 'NONE', *, *, #1304, .T. ) ;
#5242 = LINE ( 'NONE', #25469, #20298 ) ;
#5244 = EDGE_LOOP ( 'NONE', ( #21307, #19788, #30050, #5283 ) ) ;
#5245 = CARTESIAN_POINT ( 'NONE',  ( -40.27879340802675046, -12.50360960397076404, 5.949999999999999289 ) ) ;
#5246 = ORIENTED_EDGE ( 'NONE', *, *, #10345, .F. ) ;
#5247 = CYLINDRICAL_SURFACE ( 'NONE', #26778, 0.5000000000000000000 ) ;
#5248 = EDGE_CURVE ( 'NONE', #20824, #12746, #32592, .T. ) ;
#5250 = ORIENTED_EDGE ( 'NONE', *, *, #12875, .T. ) ;
#5249 = CARTESIAN_POINT ( 'NONE',  ( 71.67787245194618606, -18.34520463695562498, -1.500000000000000000 ) ) ;
#5251 = CARTESIAN_POINT ( 'NONE',  ( 10.00000000000000000, -3.641590349731950393, 3.055657119358789142 ) ) ;
#5252 = CARTESIAN_POINT ( 'NONE',  ( 5.107184442557387349, -13.01286747904930330, -1.756586276081733233 ) ) ;
#5253 = B_SPLINE_CURVE_WITH_KNOTS ( 'NONE', 3,
 ( #15717, #843, #21220, #17898, #23387, #23070, #31105, #31418 ),
 .UNSPECIFIED., .F., .F.,
 ( 4, 2, 2, 4 ),
 ( 2.213836054330188222E-07, 0.001227982086136106352, 0.001841862437401445242, 0.002455742788666784131 ),
 .UNSPECIFIED. ) ;
#5254 = DIRECTION ( 'NONE',  ( -1.000000000000000000, 0.000000000000000000, 0.000000000000000000 ) ) ;
#5255 = CARTESIAN_POINT ( 'NONE',  ( 15.65524065575999835, -15.16498509048940413, -1.499999999999999334 ) ) ;
#5256 = DIRECTION ( 'NONE',  ( 0.000000000000000000, 0.000000000000000000, 1.000000000000000000 ) ) ;
#5257 = CARTESIAN_POINT ( 'NONE',  ( 5.489343958331425632, 2.874233210898364366, 7.593062460271006842 ) ) ;
#5258 = EDGE_CURVE ( 'NONE', #16869, #18943, #1189, .T. ) ;
#5259 = CARTESIAN_POINT ( 'NONE',  ( 107.6996442589674103, 19.35565155597529596, 4.629213727441584325 ) ) ;
#5260 = ADVANCED_FACE ( 'NONE', ( #30916 ), #5810, .T. ) ;
#5261 = CARTESIAN_POINT ( 'NONE',  ( 7.307803584392339680, -13.58393279232337569, 1.499999999999999556 ) ) ;
#5262 = CARTESIAN_POINT ( 'NONE',  ( 10.00000000000000000, 1.625881193364757449, -4.467071865485455540 ) ) ;
#5263 = DIRECTION ( 'NONE',  ( 0.000000000000000000, 0.000000000000000000, -1.000000000000000000 ) ) ;
#5264 = CARTESIAN_POINT ( 'NONE',  ( 29.11693253002209403, -8.303828435806185126, -0.07017451552783579571 ) ) ;
#5265 = CARTESIAN_POINT ( 'NONE',  ( 23.74290772321994325, -0.1310194482076047495, -2.499999999999998668 ) ) ;
#5266 = DIRECTION ( 'NONE',  ( -1.000000000000000000, 0.000000000000000000, 0.000000000000000000 ) ) ;
#5267 = ADVANCED_FACE ( 'NONE', ( #25721, #7990 ), #23371, .T. ) ;
#5268 = CYLINDRICAL_SURFACE ( 'NONE', #6502, 0.5000000000000000000 ) ;
#5269 = DIRECTION ( 'NONE',  ( -6.062761635205574522E-17, -0.7071067811865465735, 0.7071067811865484609 ) ) ;
#5270 = VERTEX_POINT ( 'NONE', #15345 ) ;
#5271 = CARTESIAN_POINT ( 'NONE',  ( -6.087550801365593678, -2.752080473201636845, 2.228590825266444586 ) ) ;
#5272 = CARTESIAN_POINT ( 'NONE',  ( -10.00000000000000000, 0.000000000000000000, 0.000000000000000000 ) ) ;
#5273 = EDGE_CURVE ( 'NONE', #30224, #21233, #13018, .T. ) ;
#5274 = DIRECTION ( 'NONE',  ( -0.000000000000000000, -0.000000000000000000, 1.000000000000000000 ) ) ;
#5275 = VERTEX_POINT ( 'NONE', #3158 ) ;
#5276 = CARTESIAN_POINT ( 'NONE',  ( 18.78902641282511254, -5.535484019313972048, -4.282223223018096547 ) ) ;
#5277 = ORIENTED_EDGE ( 'NONE', *, *, #14179, .T. ) ;
#5278 = DIRECTION ( 'NONE',  ( 0.000000000000000000, 0.000000000000000000, -1.000000000000000000 ) ) ;
#5279 = EDGE_CURVE ( 'NONE', #3680, #19129, #29903, .T. ) ;
#5280 = DATE_TIME_ROLE ( 'classification_date' ) ;
#5282 = EDGE_LOOP ( 'NONE', ( #32963, #27442, #8426, #24929 ) ) ;
#5281 = CYLINDRICAL_SURFACE ( 'NONE', #504, 4.000000000000001776 ) ;
#5283 = ORIENTED_EDGE ( 'NONE', *, *, #11032, .T. ) ;
#5284 = CARTESIAN_POINT ( 'NONE',  ( -4.102033191966379277, -5.462572707106480685, 1.745628958864925639 ) ) ;
#5285 = EDGE_LOOP ( 'NONE', ( #8486, #12384, #6103, #3717 ) ) ;
#5286 = CARTESIAN_POINT ( 'NONE',  ( -7.500050800000000351, 2.983565686104819648, 0.3135853898029609677 ) ) ;
#5288 = EDGE_LOOP ( 'NONE', ( #6593, #1502, #30752, #18414 ) ) ;
#5287 = CARTESIAN_POINT ( 'NONE',  ( 0.1606233060821306291, -9.683549581721070609, -4.384181225617457045 ) ) ;
#5289 = CARTESIAN_POINT ( 'NONE',  ( 21.39187852382935517, 16.47248925749085302, 1.050000000000000044 ) ) ;
#5290 = CARTESIAN_POINT ( 'NONE',  ( -1.668773398854329396E-16, -1.946309384392623576, 4.616489984850525197 ) ) ;
#5291 = ADVANCED_FACE ( 'NONE', ( #5324 ), #331, .T. ) ;
#5292 = CARTESIAN_POINT ( 'NONE',  ( 21.37868616851651637, -21.75910453120781085, -1.431570888178362200 ) ) ;
#5293 = ADVANCED_FACE ( 'NONE', ( #20867 ), #14504, .F. ) ;
#5294 = DIRECTION ( 'NONE',  ( 1.000000000000000000, 0.000000000000000000, -1.156482317317873973E-14 ) ) ;
#5295 = ORIENTED_EDGE ( 'NONE', *, *, #22195, .T. ) ;
#5296 = CARTESIAN_POINT ( 'NONE',  ( -50.81000000000000227, -10.96999999999998643, 9.000000000000000000 ) ) ;
#5297 = DIRECTION ( 'NONE',  ( 1.000000000000000000, -0.000000000000000000, 0.000000000000000000 ) ) ;
#5298 = FACE_OUTER_BOUND ( 'NONE', #17246, .T. ) ;
#5299 = EDGE_CURVE ( 'NONE', #20515, #3016, #25744, .T. ) ;
#5300 = CARTESIAN_POINT ( 'NONE',  ( 24.47286158058016170, -17.44301205329676918, 1.467080835052755550 ) ) ;
#5301 = CARTESIAN_POINT ( 'NONE',  ( -23.35000000000000142, -10.96966150227469505, -1.500000000000000000 ) ) ;
#5302 = CARTESIAN_POINT ( 'NONE',  ( -56.77373628060693278, 0.4264188904495926913, -1.049552654929835072 ) ) ;
#5303 = CARTESIAN_POINT ( 'NONE',  ( 23.58234648083524831, -8.048792613698571685, 0.07017451552781737989 ) ) ;
#5304 = VERTEX_POINT ( 'NONE', #10157 ) ;
#5305 = FACE_OUTER_BOUND ( 'NONE', #21481, .T. ) ;
#5306 = ORIENTED_EDGE ( 'NONE', *, *, #782, .T. ) ;
#5307 = EDGE_CURVE ( 'NONE', #2513, #27551, #26298, .T. ) ;
#5308 = CARTESIAN_POINT ( 'NONE',  ( -4.104531657079157014, -0.3127741368606806738, 2.975847129947406522 ) ) ;
#5309 = PLANE ( 'NONE',  #225 ) ;
#5310 = CARTESIAN_POINT ( 'NONE',  ( 11.96689435878012553, -15.52517353469302108, 1.754064196410228371 ) ) ;
#5311 = CARTESIAN_POINT ( 'NONE',  ( 14.03158388684700242, -14.04624127993243476, 1.500000000000415223 ) ) ;
#5312 = ORIENTED_EDGE ( 'NONE', *, *, #32787, .T. ) ;
#5313 = DIRECTION ( 'NONE',  ( 0.000000000000000000, 0.000000000000000000, -1.000000000000000000 ) ) ;
#5314 = AXIS2_PLACEMENT_3D ( 'NONE', #23939, #28651, #21445 ) ;
#5315 = ADVANCED_FACE ( 'NONE', ( #8328 ), #3326, .F. ) ;
#5316 =( BOUNDED_SURFACE ( )  B_SPLINE_SURFACE ( 3, 3, ( 
 ( #18147, #15958, #10472, #300, #30550, #23667, #28038, #10794 ),
 ( #18001, #28346, #8124, #20337, #2622, #10306, #5135, #13138 ),
 ( #5462, #443, #5635, #2797, #15310, #23191, #12977, #15655 ),
 ( #20525, #15814, #13284, #25866, #25514, #28187, #22996, #12787 ) ),
 .UNSPECIFIED., .F., .F., .F. ) 
 B_SPLINE_SURFACE_WITH_KNOTS ( ( 4, 4 ),
 ( 4, 2, 2, 4 ),
 ( 0.000000000000000000, 1.000000000000000000 ),
 ( 0.000000000000000000, 0.5000000000000000000, 0.7500000000000000000, 1.000000000000000000 ),
 .UNSPECIFIED. ) 
 GEOMETRIC_REPRESENTATION_ITEM ( )  RATIONAL_B_SPLINE_SURFACE ( (
 ( 1.000000000000000000, 1.000000000000000000, 1.000000000000000000, 1.000000000000000000, 1.000000000000000000, 1.000000000000000000, 1.000000000000000000, 1.000000000000000000),
 ( 0.9743068154145673176, 0.9743068154145673176, 0.9743068154145673176, 0.9743068154145673176, 0.9743068154145673176, 0.9743068154145673176, 0.9743068154145673176, 0.9743068154145673176),
 ( 0.9743068154145673176, 0.9743068154145673176, 0.9743068154145673176, 0.9743068154145673176, 0.9743068154145673176, 0.9743068154145673176, 0.9743068154145673176, 0.9743068154145673176),
 ( 1.000000000000000000, 1.000000000000000000, 1.000000000000000000, 1.000000000000000000, 1.000000000000000000, 1.000000000000000000, 1.000000000000000000, 1.000000000000000000) ) ) 
 REPRESENTATION_ITEM ( '' )  SURFACE ( )  );
#5317 = ORIENTED_EDGE ( 'NONE', *, *, #10004, .T. ) ;
#5318 = CARTESIAN_POINT ( 'NONE',  ( 1.449017763428880334, -2.782909769958735513, 1.499999999999999556 ) ) ;
#5319 = PERSON_AND_ORGANIZATION_ROLE ( 'classification_officer' ) ;
#5320 = CARTESIAN_POINT ( 'NONE',  ( 69.06670222590935282, -6.041353941581823150, 4.093304263520331610 ) ) ;
#5321 = EDGE_CURVE ( 'NONE', #30095, #10281, #25548, .T. ) ;
#5322 = DIRECTION ( 'NONE',  ( -1.000000000000000000, 8.574039729943018344E-17, 0.000000000000000000 ) ) ;
#5324 = FACE_OUTER_BOUND ( 'NONE', #1118, .T. ) ;
#5323 = CARTESIAN_POINT ( 'NONE',  ( 0.000000000000000000, -10.76487093102063319, -1.999317321091613753 ) ) ;
#5325 = ORIENTED_EDGE ( 'NONE', *, *, #6925, .F. ) ;
#5326 = EDGE_CURVE ( 'NONE', #15255, #7000, #23071, .T. ) ;
#5327 = CARTESIAN_POINT ( 'NONE',  ( -8.000050800000000351, -1.836970198721030181E-16, -3.000000000000000444 ) ) ;
#5328 = EDGE_CURVE ( 'NONE', #30909, #16263, #28418, .T. ) ;
#5329 = DIRECTION ( 'NONE',  ( -1.000000000000000000, -0.000000000000000000, 0.000000000000000000 ) ) ;
#5330 = DIRECTION ( 'NONE',  ( 0.000000000000000000, 1.000000000000000000, 0.000000000000000000 ) ) ;
#5331 = CARTESIAN_POINT ( 'NONE',  ( 21.08401840680152617, -16.78474387323987216, -1.499999999999999556 ) ) ;
#5332 = VECTOR ( 'NONE', #11794, 1000.000000000000114 ) ;
#5334 = VERTEX_POINT ( 'NONE', #5976 ) ;
#5333 = CARTESIAN_POINT ( 'NONE',  ( -59.75626822162180218, -5.804869634004078627, 5.128141679950119602 ) ) ;
#5335 = CARTESIAN_POINT ( 'NONE',  ( -4.912550801365593856, -1.088641768524163389, -3.675193018007246071 ) ) ;
#5336 = FACE_OUTER_BOUND ( 'NONE', #26738, .T. ) ;
#5337 = AXIS2_PLACEMENT_3D ( 'NONE', #275, #4607, #25148 ) ;
#5338 = CARTESIAN_POINT ( 'NONE',  ( -53.72801162551947840, 5.497307881342318403, 1.430198536305348656 ) ) ;
#5339 = DIRECTION ( 'NONE',  ( -1.000000000000000000, -0.000000000000000000, -0.000000000000000000 ) ) ;
#5340 = ORIENTED_EDGE ( 'NONE', *, *, #27574, .T. ) ;
#5341 = VERTEX_POINT ( 'NONE', #967 ) ;
#5342 = CIRCLE ( 'NONE', #21883, 2.999999999999999556 ) ;
#5343 = DIRECTION ( 'NONE',  ( 0.000000000000000000, 0.000000000000000000, 1.000000000000000000 ) ) ;
#5344 = FACE_OUTER_BOUND ( 'NONE', #6791, .T. ) ;
#5345 = DIRECTION ( 'NONE',  ( 6.062761635205570824E-17, 0.7071067811865460184, 0.7071067811865490160 ) ) ;
#5346 = EDGE_CURVE ( 'NONE', #3542, #32298, #2804, .T. ) ;
#5347 = DIRECTION ( 'NONE',  ( 0.9842544651762055175, -0.1767573132311700268, 0.000000000000000000 ) ) ;
#5348 = LINE ( 'NONE', #12696, #23655 ) ;
#5349 = CARTESIAN_POINT ( 'NONE',  ( 47.88260332740731684, -3.822977517009183757, 0.07017451552782355551 ) ) ;
#5350 = CARTESIAN_POINT ( 'NONE',  ( 47.95950916398559372, -8.432626694227655761, 0.07017451552782036361 ) ) ;
#5351 = ORIENTED_EDGE ( 'NONE', *, *, #14019, .T. ) ;
#5352 = DIRECTION ( 'NONE',  ( -0.000000000000000000, -0.000000000000000000, -1.000000000000000000 ) ) ;
#5353 = TOROIDAL_SURFACE ( 'NONE', #16541, 7.144028715714068056, 0.5000000000000000000 ) ;
#5354 = COORDINATED_UNIVERSAL_TIME_OFFSET ( 0, 0, .AHEAD. ) ;
#5355 = CARTESIAN_POINT ( 'NONE',  ( 2.274274201625327230, 7.593217523260696211, -7.958834565716686349 ) ) ;
#5356 = ORIENTED_EDGE ( 'NONE', *, *, #17554, .F. ) ;
#5357 = ADVANCED_FACE ( 'NONE', ( #13799 ), #23587, .T. ) ;
#5358 = CIRCLE ( 'NONE', #1636, 8.749000000000002331 ) ;
#5359 = CARTESIAN_POINT ( 'NONE',  ( 107.9372220951237011, 17.82858777955670249, -4.726288973428885321 ) ) ;
#5360 = ORIENTED_EDGE ( 'NONE', *, *, #2918, .F. ) ;
#5361 = CARTESIAN_POINT ( 'NONE',  ( -16.95666531389092313, 12.15481017292670884, 1.928847951723336784 ) ) ;
#5362 = EDGE_CURVE ( 'NONE', #32789, #26634, #32674, .T. ) ;
#5364 = VERTEX_POINT ( 'NONE', #26543 ) ;
#5363 = CARTESIAN_POINT ( 'NONE',  ( 40.87814480304709264, -5.823931514470607418, -4.093303308743350577 ) ) ;
#5365 = ORIENTED_EDGE ( 'NONE', *, *, #20622, .T. ) ;
#5366 = CARTESIAN_POINT ( 'NONE',  ( -30.51827900900860158, 4.402097243136374516, 5.500000000000000000 ) ) ;
#5367 = CARTESIAN_POINT ( 'NONE',  ( -7.012550801365592612, 3.368539882008727115, 1.828967928396027176 ) ) ;
#5368 = DIRECTION ( 'NONE',  ( 0.000000000000000000, 1.000000000000000000, 0.000000000000000000 ) ) ;
#5369 = CARTESIAN_POINT ( 'NONE',  ( 29.18953645666586638, -9.308308156628569918, -0.07017451552783579571 ) ) ;
#5371 = ORIENTED_EDGE ( 'NONE', *, *, #10634, .T. ) ;
#5370 = CARTESIAN_POINT ( 'NONE',  ( 22.00111451137534502, -1.241879311143409511E-16, -2.499999999999998668 ) ) ;
#5372 = FACE_BOUND ( 'NONE', #23120, .T. ) ;
#5373 = CARTESIAN_POINT ( 'NONE',  ( 24.28956136216245199, 18.19040579244978773, 1.050000000000177458 ) ) ;
#5374 = CARTESIAN_POINT ( 'NONE',  ( -4.067339738659994097, -9.772649268812690693, 1.499999999999999112 ) ) ;
#5375 = CARTESIAN_POINT ( 'NONE',  ( 23.61000000136559507, 3.156283516753366047, 0.9349337715887203748 ) ) ;
#5376 = AXIS2_PLACEMENT_3D ( 'NONE', #12174, #23039, #22374 ) ;
#5377 = DIRECTION ( 'NONE',  ( 7.023442172597869187E-17, 0.8191520442889931308, -0.5735764363510441610 ) ) ;
#5379 = ORIENTED_EDGE ( 'NONE', *, *, #1479, .F. ) ;
#5378 = DIRECTION ( 'NONE',  ( 0.000000000000000000, 0.000000000000000000, 1.000000000000000000 ) ) ;
#5380 = LINE ( 'NONE', #25784, #12482 ) ;
#5381 = AXIS2_PLACEMENT_3D ( 'NONE', #16721, #6519, #29260 ) ;
#5382 = CIRCLE ( 'NONE', #21381, 2.099999999999990319 ) ;
#5383 = DIRECTION ( 'NONE',  ( 0.000000000000000000, 1.000000000000000000, 0.000000000000000000 ) ) ;
#5384 = CARTESIAN_POINT ( 'NONE',  ( 20.86000000136559507, -0.9349337715887248157, 3.156283516753367824 ) ) ;
#5385 = CIRCLE ( 'NONE', #12826, 10.99999999999999822 ) ;
#5386 = DIRECTION ( 'NONE',  ( 0.000000000000000000, 0.7071067811865431318, 0.7071067811865520136 ) ) ;
#5387 = CYLINDRICAL_SURFACE ( 'NONE', #11307, 0.5000000000000004441 ) ;
#5388 = CYLINDRICAL_SURFACE ( 'NONE', #1757, 0.5000000000000004441 ) ;
#5389 = CIRCLE ( 'NONE', #6434, 8.749000000000002331 ) ;
#5390 =( BOUNDED_SURFACE ( )  B_SPLINE_SURFACE ( 3, 2, ( 
 ( #22648, #22145, #15098 ),
 ( #20138, #19628, #9569 ),
 ( #27642, #19789, #4745 ),
 ( #30332, #7403, #9257 ),
 ( #11948, #254, #18448 ),
 ( #5240, #10738, #10423 ),
 ( #15599, #20287, #62 ),
 ( #13241, #2425, #33003 ),
 ( #22948, #12594, #17953 ),
 ( #25812, #22798, #28140 ) ),
 .UNSPECIFIED., .F., .F., .F. ) 
 B_SPLINE_SURFACE_WITH_KNOTS ( ( 4, 2, 2, 2, 4 ),
 ( 3, 3 ),
 ( 0.000000000000000000, 0.0003906036565455321880, 0.0007812073130910643761, 0.001171810969636596618, 0.001562414626182128752 ),
 ( 0.000000000000000000, 1.000000000000000000 ),
 .UNSPECIFIED. ) 
 GEOMETRIC_REPRESENTATION_ITEM ( )  RATIONAL_B_SPLINE_SURFACE ( (
 ( 1.000000000000000000, 0.8508761217583465930, 1.000000000000000000),
 ( 1.000000000000000000, 0.8641352639599353402, 1.000000000000000000),
 ( 1.000000000000000000, 0.8751274560303189398, 1.000000000000000000),
 ( 1.000000000000000000, 0.8893612744008715376, 1.000000000000000000),
 ( 1.000000000000000000, 0.8931697401228705369, 1.000000000000000000),
 ( 1.000000000000000000, 0.8890347101973011812, 1.000000000000000000),
 ( 1.000000000000000000, 0.8820141521041674482, 1.000000000000000000),
 ( 1.000000000000000000, 0.8603874812462587451, 1.000000000000000000),
 ( 1.000000000000000000, 0.8460710229395462800, 1.000000000000000000),
 ( 1.000000000000000000, 0.8293372616342756798, 1.000000000000000000) ) ) 
 REPRESENTATION_ITEM ( '' )  SURFACE ( )  );
#5391 = ORIENTED_EDGE ( 'NONE', *, *, #23131, .F. ) ;
#5392 = CARTESIAN_POINT ( 'NONE',  ( 107.9812534396071584, -17.79941631051923068, 4.365082084312397193 ) ) ;
#5393 = DIRECTION ( 'NONE',  ( 0.000000000000000000, 1.000000000000000000, 0.000000000000000000 ) ) ;
#5394 = ORIENTED_EDGE ( 'NONE', *, *, #4688, .T. ) ;
#5395 = CARTESIAN_POINT ( 'NONE',  ( 25.96712173632212384, 22.75279134953756355, 5.471072653610979941 ) ) ;
#5396 = AXIS2_PLACEMENT_3D ( 'NONE', #19720, #17215, #24900 ) ;
#5397 = CARTESIAN_POINT ( 'NONE',  ( 6.037141848526921706, -8.105561522824292098, -2.473100090966245279 ) ) ;
#5398 = CARTESIAN_POINT ( 'NONE',  ( 1.305960519821096844, -9.941484022874826465, -1.500000000000000444 ) ) ;
#5400 = CARTESIAN_POINT ( 'NONE',  ( 107.9481285810059887, -17.32242658709003535, 4.512007113214639986 ) ) ;
#5399 = CARTESIAN_POINT ( 'NONE',  ( 69.42401195566040428, -8.835509274236315491, 0.07017451552781736601 ) ) ;
#5401 = EDGE_CURVE ( 'NONE', #24311, #3908, #9122, .T. ) ;
#5402 = ORIENTED_EDGE ( 'NONE', *, *, #20004, .F. ) ;
#5403 = EDGE_CURVE ( 'NONE', #25459, #17821, #20927, .T. ) ;
#5404 = AXIS2_PLACEMENT_3D ( 'NONE', #25371, #14667, #12153 ) ;
#5405 = B_SPLINE_CURVE_WITH_KNOTS ( 'NONE', 3,
 ( #30930, #12842, #13182, #31098, #3027, #18390 ),
 .UNSPECIFIED., .F., .F.,
 ( 4, 2, 4 ),
 ( 0.000000000000000000, 0.0009761895969867609435, 0.001952379193973521887 ),
 .UNSPECIFIED. ) ;
#5406 = CARTESIAN_POINT ( 'NONE',  ( -40.82392219421588209, -13.09203557865092371, 5.845255965757442773 ) ) ;
#5407 = VECTOR ( 'NONE', #26866, 1000.000000000000000 ) ;
#5408 = EDGE_LOOP ( 'NONE', ( #24903, #28709, #22377, #1383 ) ) ;
#5409 = CARTESIAN_POINT ( 'NONE',  ( 2.274274201625327230, 0.000000000000000000, 0.000000000000000000 ) ) ;
#5410 = EDGE_CURVE ( 'NONE', #24839, #12213, #1316, .T. ) ;
#5412 = VERTEX_POINT ( 'NONE', #6639 ) ;
#5411 = CYLINDRICAL_SURFACE ( 'NONE', #20846, 4.000000000000001776 ) ;
#5413 = VERTEX_POINT ( 'NONE', #19023 ) ;
#5414 = CARTESIAN_POINT ( 'NONE',  ( 0.7632845268398871230, 0.000000000000000000, 0.000000000000000000 ) ) ;
#5415 = DIRECTION ( 'NONE',  ( 0.000000000000000000, 0.000000000000000000, 1.000000000000000000 ) ) ;
#5417 = ORIENTED_EDGE ( 'NONE', *, *, #8565, .T. ) ;
#5416 = CARTESIAN_POINT ( 'NONE',  ( -41.77414131929176477, -16.18685544166627821, 1.949999999999999734 ) ) ;
#5418 = ORIENTED_EDGE ( 'NONE', *, *, #22819, .F. ) ;
#5419 = CARTESIAN_POINT ( 'NONE',  ( -32.18774808610336180, -0.0003384977252905707612, 3.357274007152141415 ) ) ;
#5420 = CARTESIAN_POINT ( 'NONE',  ( 56.97280603064898941, -277.2763395528616002, -2.806473568333505586 ) ) ;
#5421 = DIRECTION ( 'NONE',  ( -1.000000000000000000, -0.000000000000000000, -0.000000000000000000 ) ) ;
#5422 = CARTESIAN_POINT ( 'NONE',  ( 5.377543748152548986, 1.391664247347228045, 7.892520144992438702 ) ) ;
#5423 = AXIS2_PLACEMENT_3D ( 'NONE', #14783, #20000, #24981 ) ;
#5424 = DIRECTION ( 'NONE',  ( -1.000000000000000000, 0.000000000000000000, 0.000000000000000000 ) ) ;
#5425 = CARTESIAN_POINT ( 'NONE',  ( 1.867159791558850035, -10.11553636635117925, 1.499999999999999334 ) ) ;
#5426 = CARTESIAN_POINT ( 'NONE',  ( 10.00000000000000178, 1.946309384392655994, -4.616489984850514539 ) ) ;
#5427 = VECTOR ( 'NONE', #18047, 1000.000000000000114 ) ;
#5428 = CIRCLE ( 'NONE', #11834, 0.4999999999999988898 ) ;
#5429 = CARTESIAN_POINT ( 'NONE',  ( 2.632061376486628301, -0.5000000000000000000, 1.500000000000000000 ) ) ;
#5430 = CARTESIAN_POINT ( 'NONE',  ( 7.249760686538667009, 0.000000000000000000, 0.000000000000000000 ) ) ;
#5431 = CARTESIAN_POINT ( 'NONE',  ( 5.377543748152549874, -2.741043480754877582, -7.530955069117540646 ) ) ;
#5432 = AXIS2_PLACEMENT_3D ( 'NONE', #25906, #10660, #21205 ) ;
#5433 = B_SPLINE_CURVE_WITH_KNOTS ( 'NONE', 3,
 ( #32840, #9911, #6891, #24605 ),
 .UNSPECIFIED., .F., .F.,
 ( 4, 4 ),
 ( 0.000000000000000000, 1.000000000000000000 ),
 .UNSPECIFIED. ) ;
#5434 = AXIS2_PLACEMENT_3D ( 'NONE', #15109, #12107, #33009 ) ;
#5435 = CARTESIAN_POINT ( 'NONE',  ( 102.5829460782277351, -0.8583298743146007270, 2.713652344655542503 ) ) ;
#5436 = DIRECTION ( 'NONE',  ( -4.917867153432966982E-17, -0.5735764363510419406, -0.8191520442889946851 ) ) ;
#5437 = ORIENTED_EDGE ( 'NONE', *, *, #14246, .F. ) ;
#5438 = CARTESIAN_POINT ( 'NONE',  ( -7.337550801365593678, 1.828967928396027176, -3.368539882008727115 ) ) ;
#5439 = AXIS2_PLACEMENT_3D ( 'NONE', #394, #10571, #28478 ) ;
#5440 = AXIS2_PLACEMENT_3D ( 'NONE', #18104, #10079, #32857 ) ;
#5441 = EDGE_CURVE ( 'NONE', #23664, #24965, #24352, .T. ) ;
#5442 = CARTESIAN_POINT ( 'NONE',  ( 25.25913793397114304, -0.3481264064496775723, 2.506178704810730018 ) ) ;
#5443 = CARTESIAN_POINT ( 'NONE',  ( 17.33093461831549931, -21.43932300456635076, -1.500000000000000000 ) ) ;
#5444 = ORIENTED_EDGE ( 'NONE', *, *, #31925, .F. ) ;
#5445 = CARTESIAN_POINT ( 'NONE',  ( -1.075551320669168254, 0.4999999999999998890, 7.404527507138928932 ) ) ;
#5446 =( LENGTH_UNIT ( ) NAMED_UNIT ( * ) SI_UNIT ( .MILLI., .METRE. ) );
#5447 = VERTEX_POINT ( 'NONE', #8959 ) ;
#5448 = CARTESIAN_POINT ( 'NONE',  ( 85.08949032934707191, -1.315411135598755665, -0.07017451552781585333 ) ) ;
#5449 = CALENDAR_DATE ( 2026, 6, 10 ) ;
#5450 = AXIS2_PLACEMENT_3D ( 'NONE', #29479, #11580, #24438 ) ;
#5452 = ORIENTED_EDGE ( 'NONE', *, *, #30008, .T. ) ;
#5451 = CARTESIAN_POINT ( 'NONE',  ( -1.921189184902703628, -10.44034746380512857, -4.522129901861166701 ) ) ;
#5453 = VERTEX_POINT ( 'NONE', #3645 ) ;
#5454 = CARTESIAN_POINT ( 'NONE',  ( 3.722706999676778317, -17.21375729507923680, 1.747812214843357692 ) ) ;
#5455 = AXIS2_PLACEMENT_3D ( 'NONE', #31871, #8939, #17315 ) ;
#5456 = CIRCLE ( 'NONE', #10788, 6.000000000000000000 ) ;
#5458 = ORIENTED_EDGE ( 'NONE', *, *, #25745, .T. ) ;
#5457 = B_SPLINE_CURVE_WITH_KNOTS ( 'NONE', 3,
 ( #5918, #11266, #8431, #6104, #26809, #21156, #5768, #16430, #925, #11102 ),
 .UNSPECIFIED., .F., .F.,
 ( 4, 2, 2, 2, 4 ),
 ( 1.968338519003748898E-07, 0.0005467926089500447324, 0.001093388384048189126, 0.001639984159146333411, 0.002186579934244477913 ),
 .UNSPECIFIED. ) ;
#5459 = CARTESIAN_POINT ( 'NONE',  ( 6.038144483126824724, 0.4487862922134418509, -8.463061282283007358 ) ) ;
#5461 = ORIENTED_EDGE ( 'NONE', *, *, #4857, .F. ) ;
#5460 = DIRECTION ( 'NONE',  ( -1.000000000000000000, 0.000000000000000000, 0.000000000000000000 ) ) ;
#5462 = CARTESIAN_POINT ( 'NONE',  ( 102.9705908278152293, -6.440317834495091098, 1.915219082070893863 ) ) ;
#5463 = DIRECTION ( 'NONE',  ( -7.023442172597914793E-17, -0.8191520442889983489, 0.5735764363510366115 ) ) ;
#5464 = CIRCLE ( 'NONE', #19346, 11.00000000000000000 ) ;
#5465 = DIRECTION ( 'NONE',  ( 0.04852105321274541305, -0.4695180821586529829, -0.8815886103626715542 ) ) ;
#5466 = CARTESIAN_POINT ( 'NONE',  ( 12.44989959798868817, 0.5174497483512729978, 13.00000000000004441 ) ) ;
#5467 = VECTOR ( 'NONE', #14067, 1000.000000000000000 ) ;
#5468 = AXIS2_PLACEMENT_3D ( 'NONE', #10348, #8168, #15505 ) ;
#5469 = ORIENTED_EDGE ( 'NONE', *, *, #17942, .F. ) ;
#5470 = CARTESIAN_POINT ( 'NONE',  ( -3.757304906975410308, -1.062355717592093463, -3.000000000000000888 ) ) ;
#5471 = LINE ( 'NONE', #15663, #2737 ) ;
#5472 = CARTESIAN_POINT ( 'NONE',  ( 3.249999999999999556, 1.239665997527021002, -9.314797388894877628 ) ) ;
#5473 = FACE_OUTER_BOUND ( 'NONE', #16920, .T. ) ;
#5474 = B_SPLINE_CURVE_WITH_KNOTS ( 'NONE', 3,
 ( #31407, #15854, #21361, #3510, #16185, #26409, #21544, #18384, #5673, #13665, #23869, #26064, #11156 ),
 .UNSPECIFIED., .F., .F.,
 ( 4, 3, 3, 3, 4 ),
 ( 0.000000000000000000, 0.0006665428069513527464, 0.001558946041704377004, 0.002451349276496870774, 0.003343752511328988881 ),
 .UNSPECIFIED. ) ;
#5475 = AXIS2_PLACEMENT_3D ( 'NONE', #12006, #4309, #27546 ) ;
#5476 = CARTESIAN_POINT ( 'NONE',  ( 0.1606232843927795639, -1.177222770084728420, 10.56438947505148462 ) ) ;
#5477 = CARTESIAN_POINT ( 'NONE',  ( 0.7632845268398871230, 0.000000000000000000, 0.000000000000000000 ) ) ;
#5479 = DIRECTION ( 'NONE',  ( -0.9896144216807899463, 0.000000000000000000, -0.1437473352845038410 ) ) ;
#5478 = UNCERTAINTY_MEASURE_WITH_UNIT (LENGTH_MEASURE( 1.000000000000000082E-05 ), #5446, 'distance_accuracy_value', 'NONE');
#5480 = VERTEX_POINT ( 'NONE', #16481 ) ;
#5481 = EDGE_CURVE ( 'NONE', #29098, #15236, #14154, .T. ) ;
#5482 = AXIS2_PLACEMENT_3D ( 'NONE', #3920, #28995, #18966 ) ;
#5483 = AXIS2_PLACEMENT_3D ( 'NONE', #21255, #19075, #24253 ) ;
#5484 = CARTESIAN_POINT ( 'NONE',  ( -3.462550801365593678, -3.521866450007987037, -0.3701630799359323931 ) ) ;
#5485 = ORIENTED_EDGE ( 'NONE', *, *, #6821, .F. ) ;
#5486 = AXIS2_PLACEMENT_3D ( 'NONE', #22130, #29656, #8902 ) ;
#5487 = CIRCLE ( 'NONE', #2286, 7.000000000000000888 ) ;
#5488 = CARTESIAN_POINT ( 'NONE',  ( -4.554531657079158080, -0.9198621039125872700, -3.105402419394638791 ) ) ;
#5489 = AXIS2_PLACEMENT_3D ( 'NONE', #29030, #26031, #18994 ) ;
#5490 = CARTESIAN_POINT ( 'NONE',  ( 107.4480426597792047, 17.91330156492432124, 4.744522527009380042 ) ) ;
#5491 = EDGE_CURVE ( 'NONE', #12355, #6855, #23860, .T. ) ;
#5492 = CARTESIAN_POINT ( 'NONE',  ( -23.54713438637982748, 2.832830518764033911, 5.958029102616976935 ) ) ;
#5493 = CARTESIAN_POINT ( 'NONE',  ( 15.81086013898917031, -14.68957282009629495, 1.499999999999169775 ) ) ;
#5494 = AXIS2_PLACEMENT_3D ( 'NONE', #23076, #30630, #14868 ) ;
#5495 = ORIENTED_EDGE ( 'NONE', *, *, #14666, .T. ) ;
#5496 = CARTESIAN_POINT ( 'NONE',  ( 2.274274201625327230, -5.222868219166924675, 9.680994141368751471 ) ) ;
#5497 = ADVANCED_FACE ( 'NONE', ( #26687 ), #16623, .T. ) ;
#5498 = AXIS2_PLACEMENT_3D ( 'NONE', #21234, #5839, #16024 ) ;
#5499 = EDGE_LOOP ( 'NONE', ( #12565, #24807, #26354 ) ) ;
#5500 = CARTESIAN_POINT ( 'NONE',  ( 3.249999999999999556, 0.000000000000000000, 0.000000000000000000 ) ) ;
#5501 = PERSON_AND_ORGANIZATION ( #6766, #25292 ) ;
#5502 = CARTESIAN_POINT ( 'NONE',  ( 85.02506012475970465, -5.029259295701730359, 4.185347070121443913 ) ) ;
#5503 = EDGE_CURVE ( 'NONE', #20196, #24740, #1806, .T. ) ;
#5504 = CARTESIAN_POINT ( 'NONE',  ( 56.97280603064898941, -277.2763395528616002, -2.334455007174283558 ) ) ;
#5505 = AXIS2_PLACEMENT_3D ( 'NONE', #26999, #1277, #24463 ) ;
#5507 = CARTESIAN_POINT ( 'NONE',  ( -7.000050800000000351, 0.000000000000000000, 0.000000000000000000 ) ) ;
#5506 = CARTESIAN_POINT ( 'NONE',  ( 25.24177585798616974, 0.08698857045690901180, 2.506775857986155209 ) ) ;
#5508 = AXIS2_PLACEMENT_3D ( 'NONE', #5725, #18584, #3556 ) ;
#5509 = ORIENTED_EDGE ( 'NONE', *, *, #24743, .F. ) ;
#5510 = VECTOR ( 'NONE', #14204, 1000.000000000000000 ) ;
#5511 = DIRECTION ( 'NONE',  ( -1.000000000000000000, 0.000000000000000000, 0.000000000000000000 ) ) ;
#5512 = CYLINDRICAL_SURFACE ( 'NONE', #20345, 4.000000000000001776 ) ;
#5513 = FACE_OUTER_BOUND ( 'NONE', #14333, .T. ) ;
#5515 = EDGE_CURVE ( 'NONE', #28105, #18235, #24498, .T. ) ;
#5514 = VECTOR ( 'NONE', #8194, 1000.000000000000114 ) ;
#5516 = DIRECTION ( 'NONE',  ( -1.000000000000000000, 0.000000000000000000, 0.000000000000000000 ) ) ;
#5518 = ORIENTED_EDGE ( 'NONE', *, *, #22001, .T. ) ;
#5517 = CYLINDRICAL_SURFACE ( 'NONE', #5886, 4.000000000000001776 ) ;
#5519 = CARTESIAN_POINT ( 'NONE',  ( -6.162550801365593856, 2.228590825266444142, 2.752080473201636845 ) ) ;
#5520 = DIRECTION ( 'NONE',  ( 8.574039729943018344E-17, 1.000000000000000000, 0.000000000000000000 ) ) ;
#5521 = CARTESIAN_POINT ( 'NONE',  ( 7.249760686538667009, 7.530955069117551304, -2.741043480754851380 ) ) ;
#5522 = AXIS2_PLACEMENT_3D ( 'NONE', #7214, #4702, #9703 ) ;
#5523 = EDGE_LOOP ( 'NONE', ( #26810, #108, #12779, #25635 ) ) ;
#5524 = EDGE_LOOP ( 'NONE', ( #30300, #12553, #11331 ) ) ;
#5525 = FACE_OUTER_BOUND ( 'NONE', #25825, .T. ) ;
#5526 = CARTESIAN_POINT ( 'NONE',  ( 1.959487840848961122E-16, 2.285372942705017341, -4.458382051008168645 ) ) ;
#5527 = ORIENTED_EDGE ( 'NONE', *, *, #22474, .T. ) ;
#5528 = CARTESIAN_POINT ( 'NONE',  ( 23.98500000136559507, -0.9349337715887247047, 3.156283516753367824 ) ) ;
#5529 = CARTESIAN_POINT ( 'NONE',  ( 19.10390797508231131, -2.015740111943978619, 0.07017451552781736601 ) ) ;
#5530 = AXIS2_PLACEMENT_3D ( 'NONE', #32736, #17842, #9816 ) ;
#5531 = DIRECTION ( 'NONE',  ( 0.000000000000000000, 1.000000000000000000, 0.000000000000000000 ) ) ;
#5532 =( BOUNDED_SURFACE ( )  B_SPLINE_SURFACE ( 3, 2, ( 
 ( #10589, #5603, #560 ),
 ( #10751, #18460, #23626 ),
 ( #28653, #751, #10933 ),
 ( #21136, #16084, #3427 ),
 ( #13587, #23793, #7774 ),
 ( #17965, #28153, #25640 ),
 ( #5255, #15429, #3727 ),
 ( #29292, #6230, #3906 ),
 ( #1398, #31823, #13739 ),
 ( #21933, #26965, #14083 ),
 ( #11919, #6081, #1050 ),
 ( #31978, #19264, #4068 ),
 ( #8564, #18953, #26622 ),
 ( #19104, #8894, #21769 ),
 ( #6378, #16575, #31482 ),
 ( #1720, #31663, #26787 ),
 ( #13893, #16267, #6567 ),
 ( #14235, #24283, #9045 ),
 ( #18774, #23941, #16415 ),
 ( #3579, #21619, #16918 ),
 ( #24431, #1549, #11242 ),
 ( #11571, #21447, #8748 ),
 ( #29648, #29143, #11729 ),
 ( #32153, #27112, #9227 ),
 ( #24105, #29468, #16766 ),
 ( #28982, #19455, #26480 ),
 ( #1232, #11424, #6728 ),
 ( #4212, #14382, #24593 ),
 ( #14581, #4883, #15240 ),
 ( #27959, #15064, #32484 ),
 ( #17749, #17267, #7054 ),
 ( #9545, #7381, #14741 ),
 ( #25093, #5064, #17066 ),
 ( #20263, #22775, #22616 ),
 ( #27465, #32826, #22274 ),
 ( #4397, #19950, #12224 ),
 ( #17569, #4720, #2211 ),
 ( #6877, #25444, #27769 ) ),
 .UNSPECIFIED., .F., .F., .F. ) 
 B_SPLINE_SURFACE_WITH_KNOTS ( ( 4, 2, 2, 2, 2, 2, 2, 2, 2, 2, 2, 2, 2, 2, 2, 2, 2, 2, 4 ),
 ( 3, 3 ),
 ( 0.01025725344258870617, 0.01409333659602720994, 0.01792941974946571371, 0.02176550290290421921, 0.02368354447962347370, 0.02560158605634272472, 0.02656060684470235023, 0.02751962763306197574, 0.02847864842142160124, 0.02943766920978123022, 0.03135571078650048471, 0.03231473157486011022, 0.03327375236321973573, 0.03423277315157936124, 0.03519179393993898675, 0.03710983551665823776, 0.03902787709337748878, 0.03998689788173712123, 0.04094591867009674674 ),
 ( 0.000000000000000000, 1.000000000000000000 ),
 .UNSPECIFIED. ) 
 GEOMETRIC_REPRESENTATION_ITEM ( )  RATIONAL_B_SPLINE_SURFACE ( (
 ( 1.000000000000000000, 0.7071067811865475727, 1.000000000000000000),
 ( 1.000000000000000000, 0.7071067811865475727, 1.000000000000000000),
 ( 1.000000000000000000, 0.7071067811865473507, 1.000000000000000000),
 ( 1.000000000000000000, 0.7071067811865473507, 1.000000000000000000),
 ( 1.000000000000000000, 0.7071067811865475727, 1.000000000000000000),
 ( 1.000000000000000000, 0.7071067811865475727, 1.000000000000000000),
 ( 1.000000000000000000, 0.7071067811865487940, 1.000000000000000000),
 ( 1.000000000000000000, 0.7071067811865487940, 1.000000000000000000),
 ( 1.000000000000000000, 0.7071067811865475727, 1.000000000000000000),
 ( 1.000000000000000000, 0.7071067811865475727, 1.000000000000000000),
 ( 1.000000000000000000, 0.7071067811865475727, 1.000000000000000000),
 ( 1.000000000000000000, 0.7071067811865475727, 1.000000000000000000),
 ( 1.000000000000000000, 0.7071067811865475727, 1.000000000000000000),
 ( 1.000000000000000000, 0.7071067811865475727, 1.000000000000000000),
 ( 1.000000000000000000, 0.7071067811865475727, 1.000000000000000000),
 ( 1.000000000000000000, 0.7071067811865475727, 1.000000000000000000),
 ( 1.000000000000000000, 0.7071067811865475727, 1.000000000000000000),
 ( 1.000000000000000000, 0.7071067811865475727, 1.000000000000000000),
 ( 1.000000000000000000, 0.7071067811865475727, 1.000000000000000000),
 ( 1.000000000000000000, 0.7071067811865475727, 1.000000000000000000),
 ( 1.000000000000000000, 0.7071067811865475727, 1.000000000000000000),
 ( 1.000000000000000000, 0.7071067811865475727, 1.000000000000000000),
 ( 1.000000000000000000, 0.7071067811865475727, 1.000000000000000000),
 ( 1.000000000000000000, 0.7071067811865475727, 1.000000000000000000),
 ( 1.000000000000000000, 0.7071067811865475727, 1.000000000000000000),
 ( 1.000000000000000000, 0.7071067811865475727, 1.000000000000000000),
 ( 1.000000000000000000, 0.7071067811865475727, 1.000000000000000000),
 ( 1.000000000000000000, 0.7071067811865475727, 1.000000000000000000),
 ( 1.000000000000000000, 0.7071067811865475727, 1.000000000000000000),
 ( 1.000000000000000000, 0.7071067811865475727, 1.000000000000000000),
 ( 1.000000000000000000, 0.7071067811865469066, 1.000000000000000000),
 ( 1.000000000000000000, 0.7071067811865469066, 1.000000000000000000),
 ( 1.000000000000000000, 0.7071067811865475727, 1.000000000000000000),
 ( 1.000000000000000000, 0.7071067811865475727, 1.000000000000000000),
 ( 1.000000000000000000, 0.7071067811865475727, 1.000000000000000000),
 ( 1.000000000000000000, 0.7071067811865475727, 1.000000000000000000),
 ( 1.000000000000000000, 0.7071067811865475727, 1.000000000000000000),
 ( 1.000000000000000000, 0.7071067811865475727, 1.000000000000000000) ) ) 
 REPRESENTATION_ITEM ( '' )  SURFACE ( )  );
#5533 = VECTOR ( 'NONE', #28061, 1000.000000000000000 ) ;
#5534 = ADVANCED_FACE ( 'NONE', ( #25179 ), #32553, .T. ) ;
#5535 = AXIS2_PLACEMENT_3D ( 'NONE', #25890, #2830, #12510 ) ;
#5536 = DIRECTION ( 'NONE',  ( -0.000000000000000000, -0.000000000000000000, -1.000000000000000000 ) ) ;
#5537 = CARTESIAN_POINT ( 'NONE',  ( 47.95695783165739101, -8.278479088713725176, 1.169950612927739941 ) ) ;
#5538 = ORIENTED_EDGE ( 'NONE', *, *, #16499, .F. ) ;
#5539 = CARTESIAN_POINT ( 'NONE',  ( 5.377543748152549874, -2.741043480754977946, 7.530955069117504230 ) ) ;
#5540 = EDGE_CURVE ( 'NONE', #9701, #14768, #13892, .T. ) ;
#5541 = AXIS2_PLACEMENT_3D ( 'NONE', #24526, #11839, #26717 ) ;
#5542 = APPROVAL_STATUS ( 'not_yet_approved' ) ;
#5544 = CARTESIAN_POINT ( 'NONE',  ( -30.51827900900859447, 4.402097243136374516, 5.049999999999999822 ) ) ;
#5543 = LOCAL_TIME ( 16, 7, 10.00000000000000000, #2533 ) ;
#5545 = ORIENTED_EDGE ( 'NONE', *, *, #11325, .F. ) ;
#5546 = CARTESIAN_POINT ( 'NONE',  ( 25.43628654896337693, -17.54453578616444176, -1.000000000000000000 ) ) ;
#5547 = ORIENTED_EDGE ( 'NONE', *, *, #25035, .F. ) ;
#5548 = CARTESIAN_POINT ( 'NONE',  ( -18.46086643607116073, 15.89617442677120707, 1.835203429153471344 ) ) ;
#5550 = ORIENTED_EDGE ( 'NONE', *, *, #32952, .T. ) ;
#5549 = CARTESIAN_POINT ( 'NONE',  ( 69.01610696340840434, -5.027975611445920201, -4.073742241459672897 ) ) ;
#5551 = ORIENTED_EDGE ( 'NONE', *, *, #28395, .F. ) ;
#5552 = CARTESIAN_POINT ( 'NONE',  ( 111.3844470440328251, -20.20075132222358505, -1.500000000000000000 ) ) ;
#5553 = DIRECTION ( 'NONE',  ( -7.023442172597867955E-17, -0.8191520442889927978, 0.5735764363510447161 ) ) ;
#5554 = CARTESIAN_POINT ( 'NONE',  ( 6.645633185707463753, -7.177124861699095248, 1.500000000000000000 ) ) ;
#5555 = EDGE_CURVE ( 'NONE', #4411, #24998, #6952, .T. ) ;
#5556 = CARTESIAN_POINT ( 'NONE',  ( 107.6503521880969885, -20.25877567811641811, -1.908490231610645793 ) ) ;
#5558 = ORIENTED_EDGE ( 'NONE', *, *, #17254, .F. ) ;
#5557 = CARTESIAN_POINT ( 'NONE',  ( 16.64984788795954884, 12.68590369525696993, -1.499999999999999778 ) ) ;
#5559 = AXIS2_PLACEMENT_3D ( 'NONE', #16450, #26655, #3469 ) ;
#5560 = VECTOR ( 'NONE', #4292, 1000.000000000000000 ) ;
#5561 = CARTESIAN_POINT ( 'NONE',  ( 3.249999999999999556, -6.478011392632841314, -6.807171995660652009 ) ) ;
#5562 = DIRECTION ( 'NONE',  ( -0.1413077769430314268, 0.9899657126261587337, 0.000000000000000000 ) ) ;
#5563 = CARTESIAN_POINT ( 'NONE',  ( 0.8026073492607572746, -15.44636574315928890, 1.746109330076501820 ) ) ;
#5564 = DIRECTION ( 'NONE',  ( -0.000000000000000000, -1.000000000000000000, -0.000000000000000000 ) ) ;
#5565 = VECTOR ( 'NONE', #5082, 1000.000000000000000 ) ;
#5566 = CARTESIAN_POINT ( 'NONE',  ( 3.381541507458993845, -0.06919447570412246007, 1.261810069052565986 ) ) ;
#5568 = ORIENTED_EDGE ( 'NONE', *, *, #17083, .T. ) ;
#5567 = DIRECTION ( 'NONE',  ( 1.000000000000000000, 0.000000000000000000, 0.000000000000000000 ) ) ;
#5569 = CARTESIAN_POINT ( 'NONE',  ( -15.12340757463330654, -21.43932300455815465, -1.500000000000000000 ) ) ;
#5570 = VECTOR ( 'NONE', #28747, 999.9999999999998863 ) ;
#5571 = CARTESIAN_POINT ( 'NONE',  ( -31.09064165252238965, -25.43932300454937945, 1.500000000000000000 ) ) ;
#5572 = CARTESIAN_POINT ( 'NONE',  ( 22.17250000136559507, -2.363507492473152283, -1.913930629741525280 ) ) ;
#5573 = APPROVAL_PERSON_ORGANIZATION ( #15496, #19229, #2148 ) ;
#5574 = EDGE_CURVE ( 'NONE', #27553, #24839, #31913, .T. ) ;
#5575 = DIRECTION ( 'NONE',  ( 1.000000000000000000, 0.000000000000000000, 0.000000000000000000 ) ) ;
#5576 = CYLINDRICAL_SURFACE ( 'NONE', #29443, 297.9387600756452912 ) ;
#5577 = CARTESIAN_POINT ( 'NONE',  ( -2.799189356625064296, 0.2797963115108609289, -0.9035254090732194321 ) ) ;
#5578 = VERTEX_POINT ( 'NONE', #9809 ) ;
#5579 = DIRECTION ( 'NONE',  ( -0.4999999999999954481, -0.8660254037844412611, -0.000000000000000000 ) ) ;
#5580 = CARTESIAN_POINT ( 'NONE',  ( -31.59999999999986997, -21.43932300455407969, 1.500000000000000000 ) ) ;
#5581 = VERTEX_POINT ( 'NONE', #20029 ) ;
#5582 = AXIS2_PLACEMENT_3D ( 'NONE', #31305, #9317, #29221 ) ;
#5583 = LINE ( 'NONE', #7569, #16200 ) ;
#5584 = CARTESIAN_POINT ( 'NONE',  ( 0.000000000000000000, 6.704570150426983233, 2.172265885002680808 ) ) ;
#5585 = CARTESIAN_POINT ( 'NONE',  ( 5.377543748152548986, -8.014274990069656823, 8.669741416787380218E-17 ) ) ;
#5587 = CARTESIAN_POINT ( 'NONE',  ( 108.0183845395928302, -18.33409491325710050, 4.565968059339312823 ) ) ;
#5586 = CARTESIAN_POINT ( 'NONE',  ( 7.990320970379346299, -10.02608796048407314, 1.000000000000000000 ) ) ;
#5588 = ORIENTED_EDGE ( 'NONE', *, *, #5719, .F. ) ;
#5589 = CARTESIAN_POINT ( 'NONE',  ( 9.282537329959740902, 0.2172754300396697036, -1.050000000000000044 ) ) ;
#5590 = EDGE_LOOP ( 'NONE', ( #2168, #22912, #27092, #22642 ) ) ;
#5591 = CARTESIAN_POINT ( 'NONE',  ( -5.304000690461529555E-12, -21.43932300456189566, 1.000000000000000000 ) ) ;
#5593 = ORIENTED_EDGE ( 'NONE', *, *, #25518, .F. ) ;
#5592 = SPHERICAL_SURFACE ( 'NONE', #26696, 0.4500000000000000111 ) ;
#5594 = ORIENTED_EDGE ( 'NONE', *, *, #22905, .T. ) ;
#5595 = LINE ( 'NONE', #13883, #16631 ) ;
#5596 = CARTESIAN_POINT ( 'NONE',  ( 3.558065962460099652, -17.13340427766722485, -1.747754039643054425 ) ) ;
#5597 = CARTESIAN_POINT ( 'NONE',  ( 26.13024263984378592, 21.17433810686643980, -4.621439243524461560 ) ) ;
#5599 = ORIENTED_EDGE ( 'NONE', *, *, #3047, .T. ) ;
#5598 = DIRECTION ( 'NONE',  ( -0.7821988420038089584, 0.6230288689682847991, 0.000000000000000000 ) ) ;
#5600 = ORIENTED_EDGE ( 'NONE', *, *, #25073, .F. ) ;
#5601 = CARTESIAN_POINT ( 'NONE',  ( 0.4198231981512192679, -4.496089151576069476, -1.766557846874257764 ) ) ;
#5602 = CARTESIAN_POINT ( 'NONE',  ( 21.31323116099696691, -21.82417724537293324, -1.319197765239386699 ) ) ;
#5603 = CARTESIAN_POINT ( 'NONE',  ( 25.61042644976673088, -17.59778802277001475, -1.500000000000000000 ) ) ;
#5604 = DIRECTION ( 'NONE',  ( 1.000000000000000000, -0.000000000000000000, -0.000000000000000000 ) ) ;
#5605 = CARTESIAN_POINT ( 'NONE',  ( 2.592584690691857485, 4.120115534666347834, 9.468199583002062880 ) ) ;
#5606 = SHAPE_REPRESENTATION ( 'Part1_handle1', ( #2865 ), #179 ) ;
#5607 = VECTOR ( 'NONE', #31230, 1000.000000000000000 ) ;
#5608 = CARTESIAN_POINT ( 'NONE',  ( -6.600050800000000883, 1.887961173149511618, 2.331437884370912705 ) ) ;
#5609 = LINE ( 'NONE', #17969, #21975 ) ;
#5610 = CARTESIAN_POINT ( 'NONE',  ( 0.000000000000000000, 0.000000000000000000, 1.500000000000000000 ) ) ;
#5611 = ADVANCED_FACE ( 'NONE', ( #30223 ), #32398, .T. ) ;
#5612 = ADVANCED_FACE ( 'NONE', ( #24852 ), #7295, .F. ) ;
#5613 = CARTESIAN_POINT ( 'NONE',  ( 11.04311965146451158, 15.00000000000000178, 1.508259000770581615 ) ) ;
#5614 = CARTESIAN_POINT ( 'NONE',  ( 2.454674724652329498, -0.02938977324473661737, 1.729574810602310775 ) ) ;
#5615 = VERTEX_POINT ( 'NONE', #12486 ) ;
#5616 = CARTESIAN_POINT ( 'NONE',  ( -9.560873106161779341E-17, -1.115095498423275266, -4.884328206559847452 ) ) ;
#5617 = ADVANCED_FACE ( 'NONE', ( #4788 ), #1970, .T. ) ;
#5618 = DIRECTION ( 'NONE',  ( 0.000000000000000000, 0.000000000000000000, 1.000000000000000000 ) ) ;
#5619 = CARTESIAN_POINT ( 'NONE',  ( 13.17798765760825574, 21.79280053074250389, -1.386497237026226959 ) ) ;
#5620 = VERTEX_POINT ( 'NONE', #7446 ) ;
#5621 = CARTESIAN_POINT ( 'NONE',  ( 3.249999999999999556, -8.734705317681630277, 0.4999240074894127361 ) ) ;
#5622 = CARTESIAN_POINT ( 'NONE',  ( 18.00753636103138078, -21.49658694930015557, -1.499999999999980682 ) ) ;
#5623 = VERTEX_POINT ( 'NONE', #11991 ) ;
#5624 = CARTESIAN_POINT ( 'NONE',  ( -2.767073886773233848, -0.6621507858625382825, -1.748408842879326075 ) ) ;
#5625 = ORIENTED_EDGE ( 'NONE', *, *, #7930, .T. ) ;
#5626 = CARTESIAN_POINT ( 'NONE',  ( 69.09268213438589612, -2.232183665269760198, -0.07017451552781585333 ) ) ;
#5627 = APPROVAL_ROLE ( '' ) ;
#5629 = VERTEX_POINT ( 'NONE', #1618 ) ;
#5628 = CARTESIAN_POINT ( 'NONE',  ( 3.568565220189176213, -17.77020640689091024, -0.9788672205760856615 ) ) ;
#5630 = VERTEX_POINT ( 'NONE', #27855 ) ;
#5631 = DIRECTION ( 'NONE',  ( -8.281886410780525818E-17, -0.9659258262890700886, 0.2588190451025141336 ) ) ;
#5632 = ORIENTED_EDGE ( 'NONE', *, *, #11934, .T. ) ;
#5633 = CARTESIAN_POINT ( 'NONE',  ( 7.249760686538667009, 0.7071067811866343922, -8.721381771256197624 ) ) ;
#5634 = ORIENTED_EDGE ( 'NONE', *, *, #18015, .T. ) ;
#5635 = CARTESIAN_POINT ( 'NONE',  ( 69.41104820195521086, -8.577144703210713317, 1.915219082070893863 ) ) ;
#5636 = CARTESIAN_POINT ( 'NONE',  ( 102.5829460782277351, -0.8583298743145996168, -2.713652344655541615 ) ) ;
#5637 = CLOSED_SHELL ( 'NONE', ( #3180, #4186, #13472, #2775, #15268, #6455, #28005, #4216, #25217, #14351, #2850, #28656, #16459, #31166, #30218, #9999, #10671, #24046, #2019, #7520, #30745, #15080, #16719, #31941, #17002, #29711, #28618, #12670, #5777, #3650, #2872, #7373, #3453, #2616, #790, #26572, #29192, #5038, #15690, #9585, #5534, #21526, #577, #20590, #21388, #14893, #13032, #30471, #8676, #22583, #28385, #976, #24336, #3233, #9997, #414, #16082, #26635, #32968, #27102, #16902, #9777, #16353, #23392, #13708, #18540, #32727, #13938, #19814, #15162, #8503, #6719, #1203, #11843, #23250, #2652, #26346, #5260, #10407, #17129, #19885, #224, #4153, #1857, #9338, #31907, #4792, #25475, #28266, #20231, #6307, #13053, #28159, #18965, #5807, #20065, #14346, #15062, #21522, #21735, #30863, #14239, #12459, #30092, #10712, #9455, #21562, #9727, #26906, #6478, #17088, #30227, #26005, #32485, #21631, #29819, #30722, #5267, #4048, #5357, #25717, #28867, #14419, #23671 ) ) ;
#5638 = DIRECTION ( 'NONE',  ( 0.000000000000000000, 0.000000000000000000, -1.000000000000000000 ) ) ;
#5639 = DIRECTION ( 'NONE',  ( 0.000000000000000000, 0.9510565162951544194, -0.3090169943749448977 ) ) ;
#5640 = ORIENTED_EDGE ( 'NONE', *, *, #20703, .T. ) ;
#5641 = DIRECTION ( 'NONE',  ( 0.000000000000000000, -0.9659258262890646485, -0.2588190451025343397 ) ) ;
#5642 = FACE_OUTER_BOUND ( 'NONE', #3006, .T. ) ;
#5643 = LINE ( 'NONE', #3474, #5607 ) ;
#5644 = ADVANCED_FACE ( 'NONE', ( #4972 ), #27364, .F. ) ;
#5645 = ADVANCED_FACE ( 'NONE', ( #29716 ), #7144, .F. ) ;
#5646 = CARTESIAN_POINT ( 'NONE',  ( 23.15209937164893006, -21.93517043476721895, 1.064739154212363648 ) ) ;
#5647 = CARTESIAN_POINT ( 'NONE',  ( 23.27353278736383047, -21.94187821002794436, 1.030224497836262687 ) ) ;
#5648 = LINE ( 'NONE', #15828, #8656 ) ;
#5649 = CARTESIAN_POINT ( 'NONE',  ( -8.000050800000000351, 0.000000000000000000, -3.000000000000000444 ) ) ;
#5650 = CARTESIAN_POINT ( 'NONE',  ( -4.162550801365592967, -2.228590825266444586, -2.752080473201636401 ) ) ;
#5651 = ORIENTED_EDGE ( 'NONE', *, *, #387, .F. ) ;
#5652 = CARTESIAN_POINT ( 'NONE',  ( -3.904531657079157725, -2.975847129947406522, -0.3127741368606805072 ) ) ;
#5653 = CARTESIAN_POINT ( 'NONE',  ( 16.10106094948406863, 19.71584668020014419, -5.396302277755718357 ) ) ;
#5654 = DIRECTION ( 'NONE',  ( -0.4851627901281766464, 0.000000000000000000, 0.8744238486426606505 ) ) ;
#5655 = CARTESIAN_POINT ( 'NONE',  ( 19.46384663066884357, -15.80031286499706056, 1.000000000000000000 ) ) ;
#5656 = ORIENTED_EDGE ( 'NONE', *, *, #18670, .T. ) ;
#5657 = FACE_OUTER_BOUND ( 'NONE', #32989, .T. ) ;
#5658 = ORIENTED_EDGE ( 'NONE', *, *, #20956, .F. ) ;
#5659 = CARTESIAN_POINT ( 'NONE',  ( 1.947468252185016624, -0.8602631160122127252, 1.758031951640323554 ) ) ;
#5660 = PERSON_AND_ORGANIZATION ( #6766, #25292 ) ;
#5661 = CARTESIAN_POINT ( 'NONE',  ( 18.76070088238846267, -5.852106601039503531, 4.033870043642440173 ) ) ;
#5663 = DIRECTION ( 'NONE',  ( 0.000000000000000000, 0.7431448254773954654, -0.6691306063588569053 ) ) ;
#5662 = DIRECTION ( 'NONE',  ( 0.000000000000000000, 0.8191520442889912434, -0.5735764363510469366 ) ) ;
#5664 = EDGE_CURVE ( 'NONE', #32100, #32058, #14655, .T. ) ;
#5665 = ORIENTED_EDGE ( 'NONE', *, *, #25084, .F. ) ;
#5666 = DIRECTION ( 'NONE',  ( -0.000000000000000000, -0.000000000000000000, -1.000000000000000000 ) ) ;
#5667 = LINE ( 'NONE', #26218, #17678 ) ;
#5668 = CARTESIAN_POINT ( 'NONE',  ( 2.864531314636031389, -7.330015575757862223, -6.140839842381257796 ) ) ;
#5669 = EDGE_CURVE ( 'NONE', #32661, #17424, #17340, .T. ) ;
#5671 = ORIENTED_EDGE ( 'NONE', *, *, #18274, .F. ) ;
#5670 = DIRECTION ( 'NONE',  ( -1.000000000000000000, -0.000000000000000000, -0.000000000000000000 ) ) ;
#5672 = CARTESIAN_POINT ( 'NONE',  ( -5.262550801365593500, -0.3701630799359326152, 3.521866450007987037 ) ) ;
#5673 = CARTESIAN_POINT ( 'NONE',  ( 108.2060071697601558, 19.32528913265312198, 3.339987910135337579 ) ) ;
#5674 = DIRECTION ( 'NONE',  ( -0.9151824489413827868, 0.4030398059120878229, 0.000000000000000000 ) ) ;
#5675 = ORIENTED_EDGE ( 'NONE', *, *, #4340, .T. ) ;
#5676 = ORIENTED_EDGE ( 'NONE', *, *, #20033, .F. ) ;
#5677 = CARTESIAN_POINT ( 'NONE',  ( 22.99325939039678701, -17.14855239172946710, -1.466877076793135837 ) ) ;
#5678 = CARTESIAN_POINT ( 'NONE',  ( -31.57659242536668032, 0.000000000000000000, -1.000000000000000000 ) ) ;
#5679 = EDGE_CURVE ( 'NONE', #2042, #10135, #5385, .T. ) ;
#5680 = CARTESIAN_POINT ( 'NONE',  ( 3.499999999999999556, 6.745408891279539354, 5.171987904998129437 ) ) ;
#5681 = CARTESIAN_POINT ( 'NONE',  ( 0.1606232872998192840, 2.144970499002737174, 10.41111328664649527 ) ) ;
#5682 = B_SPLINE_CURVE_WITH_KNOTS ( 'NONE', 3,
 ( #32401, #24854, #1972, #11493, #21689, #29365, #6456, #20340, #14809, #32555, #5138, #18003 ),
 .UNSPECIFIED., .F., .F.,
 ( 4, 2, 2, 2, 2, 4 ),
 ( 3.252606517456513302E-18, 8.901442616029611027E-05, 0.0001780288523205889679, 0.0003560577046411746833, 0.0007121154092823457887, 0.001424230818564688325 ),
 .UNSPECIFIED. ) ;
#5683 = DIRECTION ( 'NONE',  ( -1.000000000000000000, -0.000000000000000000, -0.000000000000000000 ) ) ;
#5684 = EDGE_CURVE ( 'NONE', #10113, #25309, #22844, .T. ) ;
#5685 = CARTESIAN_POINT ( 'NONE',  ( 10.00000000000000000, 3.055657119358800244, 3.641590349731939735 ) ) ;
#5686 = CARTESIAN_POINT ( 'NONE',  ( 69.15727116336863389, -7.845927800133498664, 0.07017451552781883706 ) ) ;
#5687 = ORIENTED_EDGE ( 'NONE', *, *, #2251, .F. ) ;
#5688 = CARTESIAN_POINT ( 'NONE',  ( 2.440333830125739567, -9.290196408096495162, -5.258796312403343443 ) ) ;
#5689 = ORIENTED_EDGE ( 'NONE', *, *, #11618, .F. ) ;
#5690 = PERSON_AND_ORGANIZATION_ROLE ( 'creator' ) ;
#5691 = CARTESIAN_POINT ( 'NONE',  ( 0.000000000000000000, -7.944914065997164876, 7.533794289458026761 ) ) ;
#5692 = ORIENTED_EDGE ( 'NONE', *, *, #27160, .F. ) ;
#5693 = EDGE_CURVE ( 'NONE', #8757, #15269, #30317, .T. ) ;
#5694 = DIRECTION ( 'NONE',  ( -0.000000000000000000, -0.000000000000000000, -1.000000000000000000 ) ) ;
#5695 = ORIENTED_EDGE ( 'NONE', *, *, #15869, .F. ) ;
#5696 = CARTESIAN_POINT ( 'NONE',  ( -2.617344628312510135, 0.000000000000000000, -1.468739241856748867 ) ) ;
#5697 = EDGE_CURVE ( 'NONE', #27222, #18387, #20684, .T. ) ;
#5699 = VERTEX_POINT ( 'NONE', #5636 ) ;
#5698 = CARTESIAN_POINT ( 'NONE',  ( 18.84490165312532284, -4.910910973167541549, -4.185347664746176477 ) ) ;
#5700 = EDGE_LOOP ( 'NONE', ( #8199, #3042, #17537, #6401 ) ) ;
#5701 = CARTESIAN_POINT ( 'NONE',  ( -1.047937531484008478, -4.989690239015235562, -4.522129901861164925 ) ) ;
#5702 = CARTESIAN_POINT ( 'NONE',  ( -4.162550801365592967, -2.228590825266444586, -2.752080473201636401 ) ) ;
#5703 = CARTESIAN_POINT ( 'NONE',  ( -1.082681991931092158, 0.000000000000000000, -4.612695725900422872 ) ) ;
#5704 = FACE_OUTER_BOUND ( 'NONE', #28233, .T. ) ;
#5706 = ORIENTED_EDGE ( 'NONE', *, *, #13683, .T. ) ;
#5705 = CARTESIAN_POINT ( 'NONE',  ( 0.3045634274093889649, -5.217683548413573291, 8.853895822767199775 ) ) ;
#5707 = CARTESIAN_POINT ( 'NONE',  ( -5.427698642335591239E-12, -21.93932300456189566, -1.000000000000000000 ) ) ;
#5708 = CARTESIAN_POINT ( 'NONE',  ( 15.58693300068916088, 10.49296960295601089, 1.500000000000000000 ) ) ;
#5709 = CARTESIAN_POINT ( 'NONE',  ( -3.562905260966561904, -10.36268085599621891, 1.499999999999999334 ) ) ;
#5711 = ADVANCED_FACE ( 'NONE', ( #30887 ), #15815, .F. ) ;
#5710 = CARTESIAN_POINT ( 'NONE',  ( 26.13024263984371842, 21.17433810686647533, 4.621439243524390506 ) ) ;
#5712 = CARTESIAN_POINT ( 'NONE',  ( 10.00000000000000178, -8.574039729943018837E-16, 0.000000000000000000 ) ) ;
#5714 = VERTEX_POINT ( 'NONE', #17839 ) ;
#5713 = CARTESIAN_POINT ( 'NONE',  ( 24.26973362692717018, -17.42849669161154225, 1.479847483350004156 ) ) ;
#5715 = ADVANCED_FACE ( 'NONE', ( #18148 ), #10119, .T. ) ;
#5716 = CARTESIAN_POINT ( 'NONE',  ( -32.07659242536668387, -21.93932300455396245, -1.000000000000000000 ) ) ;
#5717 = DIRECTION ( 'NONE',  ( -1.000000000000000000, 0.000000000000000000, -0.000000000000000000 ) ) ;
#5718 = CARTESIAN_POINT ( 'NONE',  ( 24.92250000273118360, -1.291182301015472378, -2.378061970571982098 ) ) ;
#5719 = EDGE_CURVE ( 'NONE', #19481, #6111, #2471, .T. ) ;
#5720 = LINE ( 'NONE', #16540, #20989 ) ;
#5721 = FACE_OUTER_BOUND ( 'NONE', #6661, .T. ) ;
#5722 = CARTESIAN_POINT ( 'NONE',  ( -2.989861291979289071, -0.09348435554434110506, -1.299029471086388998 ) ) ;
#5723 = CARTESIAN_POINT ( 'NONE',  ( 108.0241571341765621, -18.41721883922283354, 4.475799714874606039 ) ) ;
#5724 = B_SPLINE_SURFACE_WITH_KNOTS ( 'NONE', 1, 3, ( 
 ( #15436, #570, #25647, #28010, #2764, #22814, #25333, #10760, #4939, #33019, #10445, #12613, #10091, #20309, #30519, #7603 ),
 ( #5107, #22966, #12945, #15285, #23162, #25487, #274, #2595, #31342, #26795, #11430, #6235, #13418, #23799, #11090, #8901 ),
 ( #10941, #8572, #8420, #16420, #13594, #29299, #23947, #24291, #24114, #31192, #6386, #28990, #8754, #26484, #19110, #21142 ) ),
 .UNSPECIFIED., .F., .F., .F.,
 ( 2, 1, 2 ),
 ( 4, 2, 2, 2, 2, 2, 2, 4 ),
 ( -0.1724389077687537020, 0.000000000000000000, 1.000000000000000000 ),
 ( 0.000000000000000000, 0.5000000000000000000, 0.6250000000000000000, 0.7500000000000000000, 0.8125000000000000000, 0.8750000000000000000, 0.9375000000000000000, 1.000000000000000000 ),
 .UNSPECIFIED. ) ;
#5725 = CARTESIAN_POINT ( 'NONE',  ( 26.27358061090008690, 19.78731608622338101, -0.4463807625373608645 ) ) ;
#5726 = ORIENTED_EDGE ( 'NONE', *, *, #16466, .F. ) ;
#5727 = EDGE_CURVE ( 'NONE', #21443, #21158, #20830, .T. ) ;
#5728 = DIRECTION ( 'NONE',  ( 7.023442172597789069E-17, 0.8191520442889833609, 0.5735764363510581498 ) ) ;
#5729 = CARTESIAN_POINT ( 'NONE',  ( -2.998975125317107082, -0.2822817718606283055, -1.451460369366592618 ) ) ;
#5730 = CARTESIAN_POINT ( 'NONE',  ( 6.356381935169121533, 8.357622142800114062, -2.055898738447909047 ) ) ;
#5732 = CARTESIAN_POINT ( 'NONE',  ( 107.5142031382969492, -18.29244943398689927, 5.137641827787525095 ) ) ;
#5731 = CARTESIAN_POINT ( 'NONE',  ( 16.36487458112951643, 19.37645981759113312, 4.629213727441584325 ) ) ;
#5733 = ORIENTED_EDGE ( 'NONE', *, *, #23776, .F. ) ;
#5734 = DIRECTION ( 'NONE',  ( 0.000000000000000000, 1.000000000000000000, -0.000000000000000000 ) ) ;
#5735 = EDGE_LOOP ( 'NONE', ( #10219, #65, #27139, #3148 ) ) ;
#5736 = DIRECTION ( 'NONE',  ( -2.473959037481232675E-13, -1.000000000000000000, 0.000000000000000000 ) ) ;
#5738 = EDGE_LOOP ( 'NONE', ( #17736, #22892, #21302, #2728 ) ) ;
#5737 = DIRECTION ( 'NONE',  ( -0.000000000000000000, -0.000000000000000000, -1.000000000000000000 ) ) ;
#5739 = ORIENTED_EDGE ( 'NONE', *, *, #21114, .F. ) ;
#5740 = CARTESIAN_POINT ( 'NONE',  ( 10.00000000000000178, -8.574039729943018837E-16, 0.000000000000000000 ) ) ;
#5741 = EDGE_CURVE ( 'NONE', #13056, #2105, #28347, .T. ) ;
#5742 = CARTESIAN_POINT ( 'NONE',  ( 7.064423659272771161, -7.199384779417533409, 4.973063321325270181 ) ) ;
#5744 = VERTEX_POINT ( 'NONE', #12639 ) ;
#5743 = CYLINDRICAL_SURFACE ( 'NONE', #1106, 0.5000000000000000000 ) ;
#5745 = ORIENTED_EDGE ( 'NONE', *, *, #22060, .F. ) ;
#5746 = FACE_OUTER_BOUND ( 'NONE', #29191, .T. ) ;
#5747 = DIRECTION ( 'NONE',  ( 0.1995114832788637271, -0.000000000000000000, -0.9798954883250904357 ) ) ;
#5748 = ADVANCED_FACE ( 'NONE', ( #10795 ), #28188, .T. ) ;
#5749 = CARTESIAN_POINT ( 'NONE',  ( 0.6708088701982989344, 0.000000000000000000, -4.612695725900422872 ) ) ;
#5750 = CARTESIAN_POINT ( 'NONE',  ( 107.9011023225883861, -16.64526016453799073, -1.988803970548091993 ) ) ;
#5751 = CARTESIAN_POINT ( 'NONE',  ( 2.970200448035948959, 3.362738345043210675, 8.521880193026261097 ) ) ;
#5752 = DIRECTION ( 'NONE',  ( -1.000000000000000000, 0.000000000000000000, 0.000000000000000000 ) ) ;
#5753 = CARTESIAN_POINT ( 'NONE',  ( 10.97394597854683340, -14.84299795458939819, 1.500000000000000000 ) ) ;
#5754 = CARTESIAN_POINT ( 'NONE',  ( 10.57125986779756843, 1.115095498423307463, 4.884328206559839458 ) ) ;
#5755 = DIRECTION ( 'NONE',  ( 0.000000000000000000, 0.5877852522924743583, -0.8090169943749467851 ) ) ;
#5756 = CARTESIAN_POINT ( 'NONE',  ( 3.094741023239449884, -0.1906005183311319795, 1.397910568869148440 ) ) ;
#5757 = ORIENTED_EDGE ( 'NONE', *, *, #6143, .F. ) ;
#5758 = LINE ( 'NONE', #15937, #13476 ) ;
#5759 = DIRECTION ( 'NONE',  ( -1.387778780781445676E-14, 0.000000000000000000, 1.000000000000000000 ) ) ;
#5760 = DIRECTION ( 'NONE',  ( 0.000000000000000000, 0.8191520442889946851, -0.5735764363510419406 ) ) ;
#5761 = ORIENTED_EDGE ( 'NONE', *, *, #1015, .F. ) ;
#5762 = CARTESIAN_POINT ( 'NONE',  ( 21.92250000136559507, 0.3178988483021036315, 3.024605502323848949 ) ) ;
#5763 = ADVANCED_FACE ( 'NONE', ( #7637 ), #5136, .F. ) ;
#5764 = APPROVAL ( #5542, 'UNSPECIFIED' ) ;
#5765 = DIRECTION ( 'NONE',  ( 0.000000000000000000, 0.000000000000000000, 1.000000000000000000 ) ) ;
#5766 = DIRECTION ( 'NONE',  ( 0.000000000000000000, 0.000000000000000000, 1.000000000000000000 ) ) ;
#5767 = EDGE_LOOP ( 'NONE', ( #27140, #24786, #20434, #27598, #4813, #28605, #21113, #25533, #16939, #29415, #5246, #4923, #323, #31814, #4747, #24771, #23140, #2745, #13440, #5856, #24180, #16586, #15846, #18758, #7175, #5962, #2881, #10599, #9404, #23031, #19094, #19016, #29871, #28078, #6141, #14718, #12063, #7557, #20246, #21492, #7609, #30871, #27311, #21133, #19489, #25579, #4467, #27603, #22259, #10768, #1033, #16040, #27514, #6694, #10737, #8045, #29064, #27229, #23299, #25846, #19590, #26304, #11643, #1276 ) ) ;
#5768 = CARTESIAN_POINT ( 'NONE',  ( 5.887530252753768067, 6.663910820542653823, -5.105578361685848776 ) ) ;
#5769 =( NAMED_UNIT ( * ) PLANE_ANGLE_UNIT ( ) SI_UNIT ( $, .RADIAN. ) );
#5770 = ORIENTED_EDGE ( 'NONE', *, *, #29412, .F. ) ;
#5771 = CARTESIAN_POINT ( 'NONE',  ( 47.99002579013004777, -3.080023785605704667, -1.915219082070890755 ) ) ;
#5772 = DATE_AND_TIME ( #20328, #30693 ) ;
#5774 = VERTEX_POINT ( 'NONE', #5290 ) ;
#5773 = CARTESIAN_POINT ( 'NONE',  ( 18.96091535642496240, -3.614110606601104614, -2.184956778830005053 ) ) ;
#5775 = ORIENTED_EDGE ( 'NONE', *, *, #31346, .T. ) ;
#5776 = DIRECTION ( 'NONE',  ( 1.000000000000000000, -0.000000000000000000, -0.000000000000000000 ) ) ;
#5777 = ADVANCED_FACE ( 'NONE', ( #8125 ), #22997, .F. ) ;
#5778 = VERTEX_POINT ( 'NONE', #10307 ) ;
#5779 = CARTESIAN_POINT ( 'NONE',  ( 6.530491241813344061, 0.6236753264481750270, -8.637950316517738258 ) ) ;
#5781 = ORIENTED_EDGE ( 'NONE', *, *, #10179, .T. ) ;
#5780 = CARTESIAN_POINT ( 'NONE',  ( 35.33972979714662443, -3.946928302550533729, -1.169950777403906406 ) ) ;
#5782 = CARTESIAN_POINT ( 'NONE',  ( 7.064423600674403225, 0.8180878109954562438, -8.711672189282621659 ) ) ;
#5783 = EDGE_CURVE ( 'NONE', #19432, #15936, #3130, .T. ) ;
#5784 = FACE_OUTER_BOUND ( 'NONE', #22974, .T. ) ;
#5785 = CARTESIAN_POINT ( 'NONE',  ( -45.60000000000000142, -10.96966150227468972, 6.999999999999999112 ) ) ;
#5786 = EDGE_LOOP ( 'NONE', ( #18692, #15602, #15292, #31182, #29945 ) ) ;
#5787 = CARTESIAN_POINT ( 'NONE',  ( -4.100050799999999995, -0.3135853898029607456, 2.983565686104819648 ) ) ;
#5788 = DIRECTION ( 'NONE',  ( 1.000000000000000000, -0.000000000000000000, -0.000000000000000000 ) ) ;
#5789 = CARTESIAN_POINT ( 'NONE',  ( 102.5259499419699125, -5.470455821997665780, -1.529339870041445781 ) ) ;
#5790 = CARTESIAN_POINT ( 'NONE',  ( -50.60000000000000142, -21.93932300454937945, -1.000000000000000000 ) ) ;
#5791 = CARTESIAN_POINT ( 'NONE',  ( -8.000050800000003903, -1.538925392562835892, 2.674518376515694129 ) ) ;
#5792 = CARTESIAN_POINT ( 'NONE',  ( 22.91474812097366254, -21.90304135545737552, 1.273718610094523918 ) ) ;
#5793 = CARTESIAN_POINT ( 'NONE',  ( 24.25111450864415730, -3.256483526998273983E-15, 2.499999999999998668 ) ) ;
#5794 = CARTESIAN_POINT ( 'NONE',  ( 33.81874022276151237, 20.00000000000000000, -2.395703997917895123 ) ) ;
#5795 = DIRECTION ( 'NONE',  ( -0.000000000000000000, -0.000000000000000000, 1.000000000000000000 ) ) ;
#5796 = CARTESIAN_POINT ( 'NONE',  ( -4.012550801365593500, 1.828967928396027176, -3.368539882008727115 ) ) ;
#5797 = ORIENTED_EDGE ( 'NONE', *, *, #2293, .T. ) ;
#5798 = CARTESIAN_POINT ( 'NONE',  ( -5.104531657079157014, 2.975847129947406522, 0.3127741368606808403 ) ) ;
#5799 = CARTESIAN_POINT ( 'NONE',  ( 4.749760686538667009, -2.741043480754877582, -7.530955069117540646 ) ) ;
#5800 = CARTESIAN_POINT ( 'NONE',  ( -5.300050800000001061, 0.3135853898029611342, -2.983565686104819648 ) ) ;
#5801 = CARTESIAN_POINT ( 'NONE',  ( 17.02282544802756448, -15.06900748016092528, 1.500000000000000000 ) ) ;
#5802 = ORIENTED_EDGE ( 'NONE', *, *, #5832, .F. ) ;
#5803 = CARTESIAN_POINT ( 'NONE',  ( 23.50111451137534857, -3.256483526998273983E-15, 2.499999999999998668 ) ) ;
#5804 = ORIENTED_EDGE ( 'NONE', *, *, #22651, .F. ) ;
#5805 = MECHANICAL_CONTEXT ( 'NONE', #30225, 'mechanical' ) ;
#5806 = CARTESIAN_POINT ( 'NONE',  ( 18.80941384712607700, -5.307593421058961702, 4.312042181584448741 ) ) ;
#5807 = ADVANCED_FACE ( 'NONE', ( #18002 ), #15468, .T. ) ;
#5808 = EDGE_CURVE ( 'NONE', #23747, #8809, #7560, .T. ) ;
#5809 = DIRECTION ( 'NONE',  ( 0.000000000000000000, -0.9063077870366526012, 0.4226182617406938902 ) ) ;
#5810 = CYLINDRICAL_SURFACE ( 'NONE', #4390, 4.000000000000001776 ) ;
#5811 = ORIENTED_EDGE ( 'NONE', *, *, #28212, .F. ) ;
#5812 = CARTESIAN_POINT ( 'NONE',  ( 5.377543748152549874, -7.892520144992443143, 1.391664247347202288 ) ) ;
#5813 = CARTESIAN_POINT ( 'NONE',  ( -34.71268046341646141, -0.06979899340500209104, 1.021976849372826290 ) ) ;
#5814 = CARTESIAN_POINT ( 'NONE',  ( 3.500000000000000000, 0.000000000000000000, 0.000000000000000000 ) ) ;
#5816 = ORIENTED_EDGE ( 'NONE', *, *, #11427, .F. ) ;
#5815 = DIRECTION ( 'NONE',  ( 0.000000000000000000, 0.000000000000000000, 1.000000000000000000 ) ) ;
#5817 = DIRECTION ( 'NONE',  ( 1.049727191138617956E-16, 0.6018150231520437154, 0.7986355100472962709 ) ) ;
#5818 = CARTESIAN_POINT ( 'NONE',  ( -2.593512329575665296E-16, -3.024842911000718448, 3.993798362933297597 ) ) ;
#5819 = CARTESIAN_POINT ( 'NONE',  ( 69.08947486655604564, -6.491576118621911640, -3.390608973715747876 ) ) ;
#5820 = ORIENTED_EDGE ( 'NONE', *, *, #31243, .F. ) ;
#5821 = ORIENTED_EDGE ( 'NONE', *, *, #30324, .T. ) ;
#5822 = CARTESIAN_POINT ( 'NONE',  ( 1.615481217893400349E-16, -4.709950686174685153, 9.884132761439042625 ) ) ;
#5823 = FACE_OUTER_BOUND ( 'NONE', #32593, .T. ) ;
#5824 = CARTESIAN_POINT ( 'NONE',  ( 25.43628654896178176, -17.54453578616395149, 1.000000000000000000 ) ) ;
#5825 = DIRECTION ( 'NONE',  ( 1.000000000000000000, 0.000000000000000000, 0.000000000000000000 ) ) ;
#5826 = CARTESIAN_POINT ( 'NONE',  ( -57.16979796353925991, -2.912899199960345964, 5.499999999999999112 ) ) ;
#5827 = CARTESIAN_POINT ( 'NONE',  ( 107.4817635328069514, -17.82060337710651154, -5.060121585732545668 ) ) ;
#5828 = CARTESIAN_POINT ( 'NONE',  ( 107.7139893852324803, -17.39210339641074654, -4.500752875105683337 ) ) ;
#5829 = CARTESIAN_POINT ( 'NONE',  ( 102.5259499419701683, -5.470455822000431567, 1.529339870033843196 ) ) ;
#5830 = ORIENTED_EDGE ( 'NONE', *, *, #21647, .F. ) ;
#5831 = CARTESIAN_POINT ( 'NONE',  ( 0.7632845268398871230, 0.4999240074894433228, 8.734705317681628500 ) ) ;
#5832 = EDGE_CURVE ( 'NONE', #27447, #28234, #13623, .T. ) ;
#5833 = EDGE_LOOP ( 'NONE', ( #1753, #6937, #2191 ) ) ;
#5834 = DATE_AND_TIME ( #21384, #1271 ) ;
#5835 = DIRECTION ( 'NONE',  ( 0.000000000000000000, -1.000000000000000000, 0.000000000000000000 ) ) ;
#5836 = CARTESIAN_POINT ( 'NONE',  ( 23.08530182711102796, -16.84224482508541243, -0.9999999999999997780 ) ) ;
#5837 = AXIS2_PLACEMENT_3D ( 'NONE', #14216, #1531, #30401 ) ;
#5838 = EDGE_LOOP ( 'NONE', ( #15131, #10010, #11034 ) ) ;
#5839 = DIRECTION ( 'NONE',  ( 1.000000000000000000, -0.000000000000000000, -0.000000000000000000 ) ) ;
#5840 = VERTEX_POINT ( 'NONE', #31860 ) ;
#5841 = ORIENTED_EDGE ( 'NONE', *, *, #2609, .F. ) ;
#5842 = DIRECTION ( 'NONE',  ( 1.000000000000000000, 0.000000000000000000, 0.000000000000000000 ) ) ;
#5843 = CARTESIAN_POINT ( 'NONE',  ( -5.862550801365593145, -3.521866450007987037, -0.3701630799359323931 ) ) ;
#5844 = CARTESIAN_POINT ( 'NONE',  ( 8.037025183208486467, -10.89872694351444871, 1.500000000000000666 ) ) ;
#5845 = DIRECTION ( 'NONE',  ( 1.000000000000000000, 0.000000000000000000, 0.000000000000000000 ) ) ;
#5846 = AXIS2_PLACEMENT_3D ( 'NONE', #18821, #13929, #24152 ) ;
#5848 = ORIENTED_EDGE ( 'NONE', *, *, #21813, .T. ) ;
#5847 = CARTESIAN_POINT ( 'NONE',  ( 21.03177542174473658, -17.18603084754145982, -1.753176640694677380 ) ) ;
#5849 = CARTESIAN_POINT ( 'NONE',  ( -5.787550801365593856, 0.3701630799359330593, -3.521866450007987037 ) ) ;
#5850 = CARTESIAN_POINT ( 'NONE',  ( 12.22374906632087743, 4.895420474198960648, 1.050000000000000044 ) ) ;
#5851 = EDGE_CURVE ( 'NONE', #20387, #22777, #19108, .T. ) ;
#5852 = CARTESIAN_POINT ( 'NONE',  ( 8.273188133893770058, -18.97010227097647928, 1.749556775333751313 ) ) ;
#5853 = CARTESIAN_POINT ( 'NONE',  ( 21.42250000136559507, 1.913930629741522838, -2.363507492473150062 ) ) ;
#5854 = CARTESIAN_POINT ( 'NONE',  ( -48.50000000000000000, -10.96966150227468972, 7.074999999999997513 ) ) ;
#5856 = ORIENTED_EDGE ( 'NONE', *, *, #28624, .F. ) ;
#5855 = CARTESIAN_POINT ( 'NONE',  ( 3.499999999999999556, 0.000000000000000000, 0.000000000000000000 ) ) ;
#5857 = CARTESIAN_POINT ( 'NONE',  ( -29.86094048198892281, 8.975184657953134248, 2.011338252942258986 ) ) ;
#5858 = CARTESIAN_POINT ( 'NONE',  ( 22.73500000273118715, -2.486304738420683780, 0.2613211581691335383 ) ) ;
#5859 = EDGE_CURVE ( 'NONE', #23691, #32336, #23827, .T. ) ;
#5860 = CARTESIAN_POINT ( 'NONE',  ( 25.09407003920303225, -17.52096212029302436, 1.402054218073202518 ) ) ;
#5861 = AXIS2_PLACEMENT_3D ( 'NONE', #9446, #9607, #31024 ) ;
#5862 = CARTESIAN_POINT ( 'NONE',  ( 47.62814091865205768, 23.65599663307499512, 4.629213727441585213 ) ) ;
#5863 = CARTESIAN_POINT ( 'NONE',  ( -8.000050800000000351, 0.000000000000000000, 0.000000000000000000 ) ) ;
#5864 = FACE_OUTER_BOUND ( 'NONE', #26985, .T. ) ;
#5865 = AXIS2_PLACEMENT_3D ( 'NONE', #7763, #28141, #5091 ) ;
#5866 = ADVANCED_FACE ( 'NONE', ( #21314 ), #11192, .T. ) ;
#5867 = DIRECTION ( 'NONE',  ( -0.000000000000000000, -1.000000000000000000, -0.000000000000000000 ) ) ;
#5868 = ORIENTED_EDGE ( 'NONE', *, *, #18571, .F. ) ;
#5869 = AXIS2_PLACEMENT_3D ( 'NONE', #22809, #27652, #17609 ) ;
#5870 = CARTESIAN_POINT ( 'NONE',  ( 18.02407935480700374, -21.25192265501668842, 1.530583967973806470 ) ) ;
#5871 = CARTESIAN_POINT ( 'NONE',  ( -2.619932554246580731E-16, -3.055657119358825557, 3.641590349731918863 ) ) ;
#5872 = EDGE_CURVE ( 'NONE', #14230, #1418, #24521, .T. ) ;
#5873 = FACE_OUTER_BOUND ( 'NONE', #8697, .T. ) ;
#5875 = CARTESIAN_POINT ( 'NONE',  ( 107.4897528024014974, -17.93676709507456479, 5.108846369746858684 ) ) ;
#5874 = DIRECTION ( 'NONE',  ( -1.000000000000000000, 0.000000000000000000, 0.000000000000000000 ) ) ;
#5876 = ADVANCED_FACE ( 'NONE', ( #11459 ), #16503, .T. ) ;
#5877 = ORIENTED_EDGE ( 'NONE', *, *, #32540, .T. ) ;
#5878 = CARTESIAN_POINT ( 'NONE',  ( -4.912942406915327354, -5.022711880624455567E-15, 2.999999999999999556 ) ) ;
#5879 = ORIENTED_EDGE ( 'NONE', *, *, #16302, .T. ) ;
#5880 = DIRECTION ( 'NONE',  ( 1.000000000000000000, 0.000000000000000000, 0.000000000000000000 ) ) ;
#5882 = ORIENTED_EDGE ( 'NONE', *, *, #4910, .F. ) ;
#5881 = DIRECTION ( 'NONE',  ( -1.000000000000000000, 0.000000000000000000, -0.000000000000000000 ) ) ;
#5883 = ORIENTED_EDGE ( 'NONE', *, *, #14674, .F. ) ;
#5884 = CARTESIAN_POINT ( 'NONE',  ( 23.68064580653238949, -7.171681651382474598, -4.522129901861164036 ) ) ;
#5885 = CONICAL_SURFACE ( 'NONE', #24559, 300.7453860596896789, 0.4915790642873871796 ) ;
#5886 = AXIS2_PLACEMENT_3D ( 'NONE', #480, #31404, #5815 ) ;
#5887 = CARTESIAN_POINT ( 'NONE',  ( -5.807304909706597407, 1.062355717592095683, 2.999999999999999112 ) ) ;
#5889 = ORIENTED_EDGE ( 'NONE', *, *, #8715, .T. ) ;
#5888 = CARTESIAN_POINT ( 'NONE',  ( 0.000000000000000000, -2.417132211460010005, -8.149077976821821778 ) ) ;
#5890 = EDGE_LOOP ( 'NONE', ( #27128, #3340, #4895, #12730 ) ) ;
#5891 = VECTOR ( 'NONE', #24240, 1000.000000000000000 ) ;
#5892 = CARTESIAN_POINT ( 'NONE',  ( 16.00008021400722669, -20.81650718949249779, -1.751028325393708673 ) ) ;
#5893 = CARTESIAN_POINT ( 'NONE',  ( 108.0827968514280144, -19.26161617991734332, -2.743108981515642419 ) ) ;
#5894 = DIRECTION ( 'NONE',  ( 1.000000000000000000, 0.000000000000000000, 0.000000000000000000 ) ) ;
#5895 = CARTESIAN_POINT ( 'NONE',  ( 107.9443384504777868, -17.26784965035007247, -3.265388143050863334 ) ) ;
#5896 = CARTESIAN_POINT ( 'NONE',  ( 3.499999999999999556, 0.000000000000000000, 0.000000000000000000 ) ) ;
#5897 = EDGE_CURVE ( 'NONE', #25215, #21865, #28838, .T. ) ;
#5898 = AXIS2_PLACEMENT_3D ( 'NONE', #15412, #25624, #19088 ) ;
#5899 = CARTESIAN_POINT ( 'NONE',  ( 107.5617797207334689, -18.98359842993772517, -4.522129901861166701 ) ) ;
#5900 = CARTESIAN_POINT ( 'NONE',  ( 2.303719037931331037, -1.057379009928627545, 1.500000000000000000 ) ) ;
#5901 = CARTESIAN_POINT ( 'NONE',  ( 102.5016417986337274, -5.123484090875773944, 2.184956770154327543 ) ) ;
#5902 = CARTESIAN_POINT ( 'NONE',  ( -29.24402871571405882, -27.93932300454937590, 11.50000000000000000 ) ) ;
#5903 = VERTEX_POINT ( 'NONE', #3764 ) ;
#5904 = CARTESIAN_POINT ( 'NONE',  ( 47.68482864957436362, -3.825617316378707944, 0.07017451552782597024 ) ) ;
#5905 = CIRCLE ( 'NONE', #19805, 4.000000000000001776 ) ;
#5906 = CIRCLE ( 'NONE', #24061, 2.999999999999999556 ) ;
#5907 = CARTESIAN_POINT ( 'NONE',  ( 107.6659035224683407, 16.31777890981063805, 1.506649871266091401 ) ) ;
#5908 = EDGE_CURVE ( 'NONE', #25215, #12125, #15983, .T. ) ;
#5909 = LINE ( 'NONE', #18790, #27929 ) ;
#5910 = ORIENTED_EDGE ( 'NONE', *, *, #22660, .F. ) ;
#5911 = CARTESIAN_POINT ( 'NONE',  ( 24.23500000136559507, -3.156283516753370044, -0.9349337715887220401 ) ) ;
#5912 = TOROIDAL_SURFACE ( 'NONE', #27270, 8.000000000000000000, 0.5000000000000000000 ) ;
#5913 = AXIS2_PLACEMENT_3D ( 'NONE', #22511, #16982, #15157 ) ;
#5914 = CARTESIAN_POINT ( 'NONE',  ( 25.37609862591745369, -2.542614276119973038, 0.7358597233275829819 ) ) ;
#5915 = EDGE_CURVE ( 'NONE', #27064, #7973, #29326, .T. ) ;
#5916 = CARTESIAN_POINT ( 'NONE',  ( 21.24324854073032043, -21.72960979489735323, -1.457811124649064594 ) ) ;
#5917 = VERTEX_POINT ( 'NONE', #26512 ) ;
#5918 = CARTESIAN_POINT ( 'NONE',  ( 7.249760686538667009, 7.135485519862069914, -5.064320921489747995 ) ) ;
#5919 = EDGE_CURVE ( 'NONE', #17341, #19305, #1278, .T. ) ;
#5920 = ORIENTED_EDGE ( 'NONE', *, *, #24908, .T. ) ;
#5921 = VECTOR ( 'NONE', #26299, 1000.000000000000227 ) ;
#5922 = ORIENTED_EDGE ( 'NONE', *, *, #25842, .F. ) ;
#5923 = CARTESIAN_POINT ( 'NONE',  ( 25.43628628520272272, -17.54453570558254327, -1.030327512441486570 ) ) ;
#5924 = APPROVAL_STATUS ( 'not_yet_approved' ) ;
#5926 = VERTEX_POINT ( 'NONE', #3613 ) ;
#5925 = CARTESIAN_POINT ( 'NONE',  ( -4.637780547558303823, -6.332425682051282756, -0.9788672205760856615 ) ) ;
#5927 = ORIENTED_EDGE ( 'NONE', *, *, #30261, .T. ) ;
#5928 = FACE_OUTER_BOUND ( 'NONE', #19450, .T. ) ;
#5929 = VERTEX_POINT ( 'NONE', #23974 ) ;
#5930 = CARTESIAN_POINT ( 'NONE',  ( -7.312942406915325044, -8.831141768130910875E-16, 2.999999999999999556 ) ) ;
#5932 = ORIENTED_EDGE ( 'NONE', *, *, #6930, .F. ) ;
#5931 = CARTESIAN_POINT ( 'NONE',  ( 47.88260332741746339, -3.822977517009003456, -0.07017451552773958101 ) ) ;
#5933 = CARTESIAN_POINT ( 'NONE',  ( 22.85793996273714868, -21.91835824163867130, 1.144021738967093471 ) ) ;
#5934 = CARTESIAN_POINT ( 'NONE',  ( 6.357667408475527360, -0.5738000813810182343, 8.588075071450647968 ) ) ;
#5935 = CARTESIAN_POINT ( 'NONE',  ( 10.00000000000000178, -3.993798362933331791, 3.024842911000678924 ) ) ;
#5936 = DIRECTION ( 'NONE',  ( 1.145146108979476986E-14, -3.498552684802598930E-15, 1.000000000000000000 ) ) ;
#5937 = AXIS2_PLACEMENT_3D ( 'NONE', #12358, #6846, #15023 ) ;
#5938 = CARTESIAN_POINT ( 'NONE',  ( 108.0572798301028996, -18.89417742067558237, 4.649361883339969914 ) ) ;
#5940 = EDGE_CURVE ( 'NONE', #23664, #5629, #29330, .T. ) ;
#5939 = CIRCLE ( 'NONE', #6448, 0.5000000000000000000 ) ;
#5941 = PRODUCT_RELATED_PRODUCT_CATEGORY ( 'detail', '', ( #22028 ) ) ;
#5942 = CIRCLE ( 'NONE', #19313, 8.750000000000000000 ) ;
#5943 = FACE_OUTER_BOUND ( 'NONE', #3839, .T. ) ;
#5944 = CARTESIAN_POINT ( 'NONE',  ( 25.75999999999999801, -2.208672634433321348E-15, 0.000000000000000000 ) ) ;
#5945 = LINE ( 'NONE', #23201, #12848 ) ;
#5946 = VECTOR ( 'NONE', #28493, 1000.000000000000000 ) ;
#5947 = AXIS2_PLACEMENT_3D ( 'NONE', #11403, #8394, #21601 ) ;
#5948 = CIRCLE ( 'NONE', #9660, 0.4500000000000008993 ) ;
#5949 = CARTESIAN_POINT ( 'NONE',  ( -45.60000000000000142, -10.96966150227468972, 7.500000000000000000 ) ) ;
#5950 = DIRECTION ( 'NONE',  ( 1.000000000000000000, 0.000000000000000000, 0.000000000000000000 ) ) ;
#5951 = CARTESIAN_POINT ( 'NONE',  ( 3.250000000000000000, 0.000000000000000000, 0.000000000000000000 ) ) ;
#5952 = CARTESIAN_POINT ( 'NONE',  ( 6.880159329304569304, -7.110803091624023686, -5.066480354149003773 ) ) ;
#5953 = CARTESIAN_POINT ( 'NONE',  ( 108.0492846245400926, 18.45259616110433498, 4.648328607135879587 ) ) ;
#5954 = CARTESIAN_POINT ( 'NONE',  ( -3.512550801365593944, -3.675193018007246071, 1.088641768524163167 ) ) ;
#5955 = ORIENTED_EDGE ( 'NONE', *, *, #22241, .F. ) ;
#5956 = EDGE_CURVE ( 'NONE', #15425, #3908, #16321, .T. ) ;
#5957 = CARTESIAN_POINT ( 'NONE',  ( -6.800050800000000173, 2.331437884370912705, -1.887961173149511618 ) ) ;
#5958 = AXIS2_PLACEMENT_3D ( 'NONE', #27472, #4574, #12728 ) ;
#5959 = DIRECTION ( 'NONE',  ( 0.000000000000000000, 0.000000000000000000, 1.000000000000000000 ) ) ;
#5960 = DIRECTION ( 'NONE',  ( 0.000000000000000000, 0.000000000000000000, -1.000000000000000000 ) ) ;
#5961 = CARTESIAN_POINT ( 'NONE',  ( 7.289999265597088218, -8.244573099840453168, 1.499999999999714673 ) ) ;
#5962 = ORIENTED_EDGE ( 'NONE', *, *, #20640, .F. ) ;
#5963 = CARTESIAN_POINT ( 'NONE',  ( 20.48500000273118715, 0.2613211581691317065, 2.486304738420681559 ) ) ;
#5964 = CIRCLE ( 'NONE', #15022, 5.010000000000000675 ) ;
#5965 =( BOUNDED_SURFACE ( )  B_SPLINE_SURFACE ( 3, 2, ( 
 ( #22783, #44, #2061 ),
 ( #12233, #32988, #5073 ),
 ( #15250, #532, #23592 ),
 ( #18436, #11056, #18086 ),
 ( #8240, #28468, #23424 ),
 ( #28628, #28772, #5722 ),
 ( #26279, #31310, #3395 ),
 ( #6050, #15902, #30971 ),
 ( #5577, #716, #8386 ),
 ( #15758, #21257, #13082 ) ),
 .UNSPECIFIED., .F., .F., .F. ) 
 B_SPLINE_SURFACE_WITH_KNOTS ( ( 4, 2, 2, 2, 4 ),
 ( 3, 3 ),
 ( 0.000000000000000000, 0.0003906036565455327301, 0.0007812073130910654603, 0.001171810969636598136, 0.001562414626182130921 ),
 ( 0.000000000000000000, 1.000000000000000000 ),
 .UNSPECIFIED. ) 
 GEOMETRIC_REPRESENTATION_ITEM ( )  RATIONAL_B_SPLINE_SURFACE ( (
 ( 1.000000000000000000, 0.8508761217583471481, 1.000000000000000000),
 ( 1.000000000000000000, 0.8641352639599342300, 1.000000000000000000),
 ( 1.000000000000000000, 0.8751274560303193839, 1.000000000000000000),
 ( 1.000000000000000000, 0.8893612744008719817, 1.000000000000000000),
 ( 1.000000000000000000, 0.8931697401227335353, 1.000000000000000000),
 ( 1.000000000000000000, 0.8890347101974386268, 1.000000000000000000),
 ( 1.000000000000000000, 0.8820141521043950439, 1.000000000000000000),
 ( 1.000000000000000000, 0.8603874812460335919, 1.000000000000000000),
 ( 1.000000000000000000, 0.8460710229397098159, 1.000000000000000000),
 ( 1.000000000000000000, 0.8293372616342803427, 1.000000000000000000) ) ) 
 REPRESENTATION_ITEM ( '' )  SURFACE ( )  );
#5966 = AXIS2_PLACEMENT_3D ( 'NONE', #25406, #2516, #15518 ) ;
#5967 = VERTEX_POINT ( 'NONE', #14774 ) ;
#5968 = CARTESIAN_POINT ( 'NONE',  ( 0.5135429646647714508, -4.169291690411378148, 1.765415482494630428 ) ) ;
#5969 = PERSON_AND_ORGANIZATION ( #6766, #25292 ) ;
#5970 = CARTESIAN_POINT ( 'NONE',  ( 69.01948419709430027, -5.095663605514894279, 4.155405370688038502 ) ) ;
#5971 = VECTOR ( 'NONE', #26093, 1000.000000000000000 ) ;
#5972 = AXIS2_PLACEMENT_3D ( 'NONE', #16394, #28779, #26607 ) ;
#5973 = AXIS2_PLACEMENT_3D ( 'NONE', #28220, #10504, #10834 ) ;
#5974 = CARTESIAN_POINT ( 'NONE',  ( 7.249760686538667009, -8.466096581343467875, -2.210816291636301223 ) ) ;
#5975 = CARTESIAN_POINT ( 'NONE',  ( 2.589202797589355232, -1.003524335601107209, 10.26630467377260914 ) ) ;
#5976 = CARTESIAN_POINT ( 'NONE',  ( 10.00000000000000000, -0.8254815157535566605, 4.681538312723513506 ) ) ;
#5977 = ORIENTED_EDGE ( 'NONE', *, *, #11976, .T. ) ;
#5978 = CARTESIAN_POINT ( 'NONE',  ( -23.35000000000000142, -10.96966150227469505, -11.00000000000000000 ) ) ;
#5979 = EDGE_CURVE ( 'NONE', #16174, #7245, #21341, .T. ) ;
#5980 = PLANE ( 'NONE',  #3829 ) ;
#5981 = CARTESIAN_POINT ( 'NONE',  ( 21.29750000136559507, -2.363507492473152283, -1.913930629741525280 ) ) ;
#5983 = ORIENTED_EDGE ( 'NONE', *, *, #1877, .T. ) ;
#5982 = CARTESIAN_POINT ( 'NONE',  ( 108.2060074055500394, 19.32529044562417653, -3.323467105140293310 ) ) ;
#5984 = AXIS2_PLACEMENT_3D ( 'NONE', #11656, #1143, #16846 ) ;
#5985 = CARTESIAN_POINT ( 'NONE',  ( -4.362550801365593145, -2.752080473201636845, 2.228590825266444586 ) ) ;
#5986 = AXIS2_PLACEMENT_3D ( 'NONE', #20315, #31200, #5618 ) ;
#5987 = CARTESIAN_POINT ( 'NONE',  ( 10.00000000000000000, -4.458382051008177527, -2.285372942705001797 ) ) ;
#5988 = CARTESIAN_POINT ( 'NONE',  ( 23.64679384717729960, -7.447389048086114016, -2.184956778833867297 ) ) ;
#5989 = VECTOR ( 'NONE', #1482, 1000.000000000000000 ) ;
#5990 = EDGE_LOOP ( 'NONE', ( #32628, #24341, #12044, #26861, #16382, #14656, #27783, #26303, #10189, #21802, #29947 ) ) ;
#5991 = ORIENTED_EDGE ( 'NONE', *, *, #3260, .F. ) ;
#5992 = VECTOR ( 'NONE', #1541, 999.9999999999998863 ) ;
#5993 = CIRCLE ( 'NONE', #15585, 0.5000000000000004441 ) ;
#5994 = DIRECTION ( 'NONE',  ( -1.000000000000000000, 8.574039729943017111E-17, -0.000000000000000000 ) ) ;
#5996 = AXIS2_PLACEMENT_3D ( 'NONE', #22350, #8970, #29374 ) ;
#5995 = CARTESIAN_POINT ( 'NONE',  ( -9.288857950784214168, 3.520075575296779835, 1.500000000000000222 ) ) ;
#5997 = DIRECTION ( 'NONE',  ( -1.000000000000000000, 8.574039729943018344E-17, -0.000000000000000000 ) ) ;
#5998 = CARTESIAN_POINT ( 'NONE',  ( 17.36028307725516839, -18.11957666780532250, 4.522129901861156931 ) ) ;
#5999 = EDGE_CURVE ( 'NONE', #30211, #22618, #32519, .T. ) ;
#6000 = CARTESIAN_POINT ( 'NONE',  ( -23.54713438637982748, 13.45615422372499914, 10.69317089570273360 ) ) ;
#6001 = EDGE_CURVE ( 'NONE', #11582, #7955, #1587, .T. ) ;
#6002 = CIRCLE ( 'NONE', #24676, 6.248999999999998778 ) ;
#6003 = CARTESIAN_POINT ( 'NONE',  ( 7.249760686538667009, 2.318425219014346172, -8.437262856154140067 ) ) ;
#6004 = CARTESIAN_POINT ( 'NONE',  ( -1.773875666770781789, -0.3178988483021056854, 3.024605502323848949 ) ) ;
#6005 = EDGE_CURVE ( 'NONE', #18566, #2513, #27734, .T. ) ;
#6006 = CARTESIAN_POINT ( 'NONE',  ( -3.237550801365593145, 3.675193018007246959, -1.088641768524161391 ) ) ;
#6007 = FACE_OUTER_BOUND ( 'NONE', #8856, .T. ) ;
#6008 = CARTESIAN_POINT ( 'NONE',  ( 85.13336101766876141, -6.778540831290548851, 1.169950242236417415 ) ) ;
#6009 = ORIENTED_EDGE ( 'NONE', *, *, #9139, .T. ) ;
#6010 = DIRECTION ( 'NONE',  ( 0.000000000000000000, -0.9271838545667856479, -0.3746065934159163446 ) ) ;
#6011 = VECTOR ( 'NONE', #7372, 1000.000000000000000 ) ;
#6012 = ORIENTED_EDGE ( 'NONE', *, *, #4011, .T. ) ;
#6014 = AXIS2_PLACEMENT_3D ( 'NONE', #8718, #31630, #16244 ) ;
#6013 = COORDINATED_UNIVERSAL_TIME_OFFSET ( 0, 0, .AHEAD. ) ;
#6015 = LINE ( 'NONE', #21230, #12337 ) ;
#6016 = AXIS2_PLACEMENT_3D ( 'NONE', #27968, #22929, #5386 ) ;
#6017 = AXIS2_PLACEMENT_3D ( 'NONE', #11548, #21416, #14207 ) ;
#6018 = AXIS2_PLACEMENT_3D ( 'NONE', #13085, #47, #25798 ) ;
#6019 = CARTESIAN_POINT ( 'NONE',  ( 107.9622325421415212, 20.81773585569407459, 1.508259000770582059 ) ) ;
#6020 = VERTEX_POINT ( 'NONE', #19801 ) ;
#6021 = CARTESIAN_POINT ( 'NONE',  ( 101.7221769401408409, -2.897900707892763439, -3.993434276071010203 ) ) ;
#6022 = ORIENTED_EDGE ( 'NONE', *, *, #1125, .T. ) ;
#6023 = ORIENTED_EDGE ( 'NONE', *, *, #19387, .F. ) ;
#6024 = CARTESIAN_POINT ( 'NONE',  ( 71.38866214474374772, -19.82505015907488755, -4.522129901861164925 ) ) ;
#6025 = CARTESIAN_POINT ( 'NONE',  ( -4.262550801365594388, -3.521866450007987037, -0.3701630799359323931 ) ) ;
#6026 = CARTESIAN_POINT ( 'NONE',  ( 7.106060642427830309, -3.992384276486468320, 1.500000000000000444 ) ) ;
#6027 = AXIS2_PLACEMENT_3D ( 'NONE', #9213, #1537, #7039 ) ;
#6028 = CARTESIAN_POINT ( 'NONE',  ( 2.632061376486627857, -0.5000000000000015543, -1.499999999999999112 ) ) ;
#6030 = VERTEX_POINT ( 'NONE', #4103 ) ;
#6029 = CARTESIAN_POINT ( 'NONE',  ( 21.15383509118241889, 16.85013971177662384, -1.500000000000000222 ) ) ;
#6031 = CARTESIAN_POINT ( 'NONE',  ( -6.437550801365593323, 3.675193018007247403, -1.088641768524161391 ) ) ;
#6032 = DIRECTION ( 'NONE',  ( 0.000000000000000000, 0.000000000000000000, 1.000000000000000000 ) ) ;
#6033 = B_SPLINE_CURVE_WITH_KNOTS ( 'NONE', 3,
 ( #22050, #27208, #9149, #21710, #4507, #24881 ),
 .UNSPECIFIED., .F., .F.,
 ( 4, 2, 4 ),
 ( 3.736708725176135323E-17, 0.001196153005899993748, 0.002392306011799950199 ),
 .UNSPECIFIED. ) ;
#6034 = DIRECTION ( 'NONE',  ( -2.473959037481232675E-13, -1.000000000000000000, 0.000000000000000000 ) ) ;
#6035 = CARTESIAN_POINT ( 'NONE',  ( 0.000000000000000000, 6.704570150426983233, 2.172265885002680808 ) ) ;
#6037 = EDGE_LOOP ( 'NONE', ( #20454, #15710, #10776, #8020 ) ) ;
#6036 = DIRECTION ( 'NONE',  ( -0.000000000000000000, -0.3746065934159164001, 0.9271838545667856479 ) ) ;
#6038 = EDGE_CURVE ( 'NONE', #28338, #7332, #6762, .T. ) ;
#6039 = VECTOR ( 'NONE', #19525, 1000.000000000000000 ) ;
#6040 = VECTOR ( 'NONE', #23734, 1000.000000000000000 ) ;
#6041 = DIRECTION ( 'NONE',  ( -0.4999999999999981681, -0.8660254037844395958, 0.000000000000000000 ) ) ;
#6042 = LINE ( 'NONE', #16538, #14670 ) ;
#6043 = CIRCLE ( 'NONE', #24721, 9.500000000000003553 ) ;
#6044 = EDGE_CURVE ( 'NONE', #22148, #32347, #9581, .T. ) ;
#6045 = AXIS2_PLACEMENT_3D ( 'NONE', #30581, #7664, #9651 ) ;
#6046 = CARTESIAN_POINT ( 'NONE',  ( 6.357667697713671018, -0.9262207444595329520, -8.557242355892498153 ) ) ;
#6048 = EDGE_CURVE ( 'NONE', #9165, #9138, #7447, .T. ) ;
#6047 = CIRCLE ( 'NONE', #28466, 0.5000000000000004441 ) ;
#6049 = CARTESIAN_POINT ( 'NONE',  ( 78.59573142019985426, 24.17918843217023195, 5.412820279296878923 ) ) ;
#6050 = CARTESIAN_POINT ( 'NONE',  ( -2.742527549463608771, 0.2598362491861793688, -1.021881266978575731 ) ) ;
#6051 = DIRECTION ( 'NONE',  ( -0.000000000000000000, -0.000000000000000000, -1.000000000000000000 ) ) ;
#6052 = SECURITY_CLASSIFICATION ( '', '', #12551 ) ;
#6053 = CARTESIAN_POINT ( 'NONE',  ( 7.249760686538667009, 8.014274990069656823, -8.669741416787380218E-17 ) ) ;
#6054 = CARTESIAN_POINT ( 'NONE',  ( -5.987550801365593145, -3.521866450007987037, -0.3701630799359323931 ) ) ;
#6055 = ORIENTED_EDGE ( 'NONE', *, *, #12708, .T. ) ;
#6056 = B_SPLINE_CURVE_WITH_KNOTS ( 'NONE', 3,
 ( #7442, #25361, #17641, #27850 ),
 .UNSPECIFIED., .F., .F.,
 ( 4, 4 ),
 ( 0.000000000000000000, 0.0002520312449908130637 ),
 .UNSPECIFIED. ) ;
#6057 = CARTESIAN_POINT ( 'NONE',  ( 10.00000000000000000, -3.641590349731950393, 3.055657119358789142 ) ) ;
#6058 = DIRECTION ( 'NONE',  ( -0.000000000000000000, -0.000000000000000000, -1.000000000000000000 ) ) ;
#6060 = DIRECTION ( 'NONE',  ( 0.000000000000000000, 0.000000000000000000, 1.000000000000000000 ) ) ;
#6059 = LINE ( 'NONE', #889, #16630 ) ;
#6061 = ORIENTED_EDGE ( 'NONE', *, *, #8432, .F. ) ;
#6062 = AXIS2_PLACEMENT_3D ( 'NONE', #20797, #2952, #7925 ) ;
#6063 = CARTESIAN_POINT ( 'NONE',  ( -4.850050800000000883, -1.549418761218565255, 2.853674364686380471 ) ) ;
#6064 = ORIENTED_EDGE ( 'NONE', *, *, #16968, .T. ) ;
#6065 = DIRECTION ( 'NONE',  ( 7.023442172597900002E-17, 0.8191520442889966835, -0.5735764363510392760 ) ) ;
#6067 = VERTEX_POINT ( 'NONE', #9932 ) ;
#6066 = FACE_OUTER_BOUND ( 'NONE', #26407, .T. ) ;
#6068 = EDGE_LOOP ( 'NONE', ( #4180, #5360, #23087, #1763 ) ) ;
#6069 = CARTESIAN_POINT ( 'NONE',  ( 102.8580990270160385, -4.820463887425400884, -4.522129901861164036 ) ) ;
#6070 = VECTOR ( 'NONE', #22048, 1000.000000000000000 ) ;
#6071 = AXIS2_PLACEMENT_3D ( 'NONE', #2967, #13123, #28669 ) ;
#6072 = VECTOR ( 'NONE', #6816, 1000.000000000000000 ) ;
#6073 = CARTESIAN_POINT ( 'NONE',  ( -6.000050802731188959, 3.113457007523260156, -0.9222479816126439855 ) ) ;
#6075 = VERTEX_POINT ( 'NONE', #27149 ) ;
#6074 = LINE ( 'NONE', #1045, #4300 ) ;
#6076 = CARTESIAN_POINT ( 'NONE',  ( 17.54326037862280430, 13.05023557628343056, -1.500000000000000000 ) ) ;
#6077 = CARTESIAN_POINT ( 'NONE',  ( 7.721070889493614864, -18.80910814508606066, -1.749364008687505301 ) ) ;
#6078 = EDGE_CURVE ( 'NONE', #14302, #21638, #22391, .T. ) ;
#6079 = DIRECTION ( 'NONE',  ( -1.000000000000000000, 2.473959037481237219E-13, -0.000000000000000000 ) ) ;
#6080 = CC_DESIGN_SECURITY_CLASSIFICATION ( #26353, ( #17797 ) ) ;
#6081 = CARTESIAN_POINT ( 'NONE',  ( 11.72844749914836271, -13.05523934214929582, -1.500000000000280220 ) ) ;
#6082 = CARTESIAN_POINT ( 'NONE',  ( 107.9806121034343818, -17.79018122917594269, -4.339844731563715641 ) ) ;
#6083 = DIRECTION ( 'NONE',  ( -1.000000000000000000, -0.000000000000000000, -0.000000000000000000 ) ) ;
#6084 = EDGE_CURVE ( 'NONE', #19227, #6218, #31091, .T. ) ;
#6085 = B_SPLINE_CURVE_WITH_KNOTS ( 'NONE', 3,
 ( #14625, #25331, #10089, #15118 ),
 .UNSPECIFIED., .F., .F.,
 ( 4, 4 ),
 ( 5.099451029762119343E-07, 0.0003283404404905848075 ),
 .UNSPECIFIED. ) ;
#6086 = B_SPLINE_CURVE_WITH_KNOTS ( 'NONE', 3,
 ( #7538, #16224, #8518, #21399, #5705, #23267, #6191, #18421 ),
 .UNSPECIFIED., .F., .F.,
 ( 4, 2, 2, 4 ),
 ( 2.304311362529957687E-07, 0.001227991214883143506, 0.001841871606756588899, 0.002455751998630034509 ),
 .UNSPECIFIED. ) ;
#6087 = CARTESIAN_POINT ( 'NONE',  ( 7.249760686538667009, 0.000000000000000000, 0.000000000000000000 ) ) ;
#6088 = CARTESIAN_POINT ( 'NONE',  ( -23.54713438637982748, 8.275374457817619600, 8.600000000000004974 ) ) ;
#6089 = EDGE_CURVE ( 'NONE', #7759, #19976, #17453, .T. ) ;
#6090 = EDGE_CURVE ( 'NONE', #28814, #27014, #7264, .T. ) ;
#6091 = CARTESIAN_POINT ( 'NONE',  ( -3.150050800000000262, -3.113457007523259268, 0.9222479816126455399 ) ) ;
#6092 = DIRECTION ( 'NONE',  ( 0.000000000000000000, 0.000000000000000000, 1.000000000000000000 ) ) ;
#6093 = CIRCLE ( 'NONE', #246, 8.749000000000002331 ) ;
#6094 = VERTEX_POINT ( 'NONE', #14424 ) ;
#6095 = CARTESIAN_POINT ( 'NONE',  ( -3.691545173129016004E-13, 1.425064293572904539, 10.85582367538961535 ) ) ;
#6096 = EDGE_CURVE ( 'NONE', #21274, #5714, #20005, .T. ) ;
#6097 = PLANE ( 'NONE',  #21993 ) ;
#6098 = CARTESIAN_POINT ( 'NONE',  ( 2.437082316315989594, 10.59788678609684176, 1.217322776604743639 ) ) ;
#6099 = VERTEX_POINT ( 'NONE', #9269 ) ;
#6100 = CARTESIAN_POINT ( 'NONE',  ( 25.31491971536988927, -1.639151784509444987, 1.999968332672603877 ) ) ;
#6101 = CARTESIAN_POINT ( 'NONE',  ( 21.05407077897105594, -21.72523992960374883, -1.419373079979250551 ) ) ;
#6102 = SECURITY_CLASSIFICATION ( '', '', #3120 ) ;
#6103 = ORIENTED_EDGE ( 'NONE', *, *, #29034, .T. ) ;
#6104 = CARTESIAN_POINT ( 'NONE',  ( 6.530491751506348308, 7.017944781892023975, -5.074604403564599409 ) ) ;
#6105 = ORIENTED_EDGE ( 'NONE', *, *, #1570, .T. ) ;
#6106 = EDGE_CURVE ( 'NONE', #22604, #13143, #6358, .T. ) ;
#6107 = EDGE_LOOP ( 'NONE', ( #3864, #30498, #15782, #13882 ) ) ;
#6108 = CARTESIAN_POINT ( 'NONE',  ( 24.40424503925390454, -17.45211869376770153, -1.605444122987507383 ) ) ;
#6110 = ORIENTED_EDGE ( 'NONE', *, *, #7356, .F. ) ;
#6109 = CARTESIAN_POINT ( 'NONE',  ( -0.6528202993443394941, 0.000000000000000000, 5.412820279296878923 ) ) ;
#6111 = VERTEX_POINT ( 'NONE', #557 ) ;
#6112 = LINE ( 'NONE', #16608, #3297 ) ;
#6113 = ORIENTED_EDGE ( 'NONE', *, *, #26910, .F. ) ;
#6114 = DIRECTION ( 'NONE',  ( -0.8660254037844399289, 0.4999999999999978906, 0.000000000000000000 ) ) ;
#6115 = AXIS2_PLACEMENT_3D ( 'NONE', #24329, #11967, #26520 ) ;
#6117 = ORIENTED_EDGE ( 'NONE', *, *, #9574, .F. ) ;
#6116 = LINE ( 'NONE', #3462, #3749 ) ;
#6118 = DIRECTION ( 'NONE',  ( -0.000000000000000000, 0.000000000000000000, 1.000000000000000000 ) ) ;
#6119 = CARTESIAN_POINT ( 'NONE',  ( 0.6420652513406681638, 8.983930386558810710, 2.300561732648136015 ) ) ;
#6120 = DIRECTION ( 'NONE',  ( -1.000000000000000000, 8.574039729943018344E-17, -0.000000000000000000 ) ) ;
#6121 = CARTESIAN_POINT ( 'NONE',  ( 7.064632951172269415, 5.064320921489821714, 7.135485519862013959 ) ) ;
#6122 = CARTESIAN_POINT ( 'NONE',  ( 107.5620291353747717, -18.98729610813186852, 4.512028494923953303 ) ) ;
#6123 = CARTESIAN_POINT ( 'NONE',  ( 6.220890055307039646, -15.20372210278347680, -4.522129901861164925 ) ) ;
#6124 = DIRECTION ( 'NONE',  ( -1.000000000000000000, -0.000000000000000000, 0.000000000000000000 ) ) ;
#6125 = CARTESIAN_POINT ( 'NONE',  ( 18.96044790064761898, -3.619335823787583006, 0.07017451552783579571 ) ) ;
#6126 = EDGE_CURVE ( 'NONE', #5615, #9418, #32665, .T. ) ;
#6127 = EDGE_CURVE ( 'NONE', #21122, #21390, #17145, .T. ) ;
#6128 = DIRECTION ( 'NONE',  ( 1.000000000000000000, -8.574039729943018344E-17, -0.000000000000000000 ) ) ;
#6129 = DIRECTION ( 'NONE',  ( -0.03487826274237470353, -0.9987827659587183993, -0.03487826274237470353 ) ) ;
#6130 = CARTESIAN_POINT ( 'NONE',  ( 24.10999999999999943, 1.942864903642424146, 1.573300977624592534 ) ) ;
#6131 = DIRECTION ( 'NONE',  ( 0.000000000000000000, 0.000000000000000000, -1.000000000000000000 ) ) ;
#6132 = FACE_OUTER_BOUND ( 'NONE', #18744, .T. ) ;
#6133 = EDGE_CURVE ( 'NONE', #18871, #15255, #25986, .T. ) ;
#6134 = CARTESIAN_POINT ( 'NONE',  ( -4.262550801365594388, -3.521866450007987037, -0.3701630799359323931 ) ) ;
#6135 = ORIENTED_EDGE ( 'NONE', *, *, #21668, .F. ) ;
#6136 = CARTESIAN_POINT ( 'NONE',  ( -7.000050800000001239, -1.887961173149512062, -2.331437884370912261 ) ) ;
#6137 = AXIS2_PLACEMENT_3D ( 'NONE', #6088, #3582, #3733 ) ;
#6138 = CARTESIAN_POINT ( 'NONE',  ( 107.6996442589676235, 19.35565155597516807, 4.629213727441722881 ) ) ;
#6139 = CARTESIAN_POINT ( 'NONE',  ( -0.9232102171129831225, 0.000000000000000000, -4.522129901861166701 ) ) ;
#6140 = CARTESIAN_POINT ( 'NONE',  ( 7.289999264625238951, -8.244573099998591559, 1.000000000000000000 ) ) ;
#6141 = ORIENTED_EDGE ( 'NONE', *, *, #22846, .F. ) ;
#6142 = CARTESIAN_POINT ( 'NONE',  ( 0.000000000000000000, 0.000000000000000000, 0.000000000000000000 ) ) ;
#6143 = EDGE_CURVE ( 'NONE', #3835, #6959, #25826, .T. ) ;
#6144 = CC_DESIGN_DATE_AND_TIME_ASSIGNMENT ( #13275, #23659, ( #27464 ) ) ;
#6145 = ORIENTED_EDGE ( 'NONE', *, *, #21065, .T. ) ;
#6146 = CARTESIAN_POINT ( 'NONE',  ( 6.718200922662554753, -13.33586090649603229, 1.500000000000000000 ) ) ;
#6147 = PERSON_AND_ORGANIZATION_ROLE ( 'classification_officer' ) ;
#6148 = CARTESIAN_POINT ( 'NONE',  ( 69.05424452631314125, -5.791958783386577103, 4.275175994950480174 ) ) ;
#6149 = CARTESIAN_POINT ( 'NONE',  ( 22.29416355858534970, 17.04711948199285843, -1.050000000000000266 ) ) ;
#6150 = FACE_OUTER_BOUND ( 'NONE', #32449, .T. ) ;
#6151 = DIRECTION ( 'NONE',  ( -1.000000000000000000, 0.000000000000000000, 0.000000000000000000 ) ) ;
#6152 = ORIENTED_EDGE ( 'NONE', *, *, #26707, .F. ) ;
#6153 = CARTESIAN_POINT ( 'NONE',  ( 6.356381935169119757, -8.357622142800098075, 2.055898738447969887 ) ) ;
#6154 = CARTESIAN_POINT ( 'NONE',  ( 25.18701699284994078, 18.96209959523617172, -1.477901791411339483 ) ) ;
#6155 = CARTESIAN_POINT ( 'NONE',  ( -1.152183934781129714E-14, 21.49000000000002331, 1.500000000000000000 ) ) ;
#6157 = ORIENTED_EDGE ( 'NONE', *, *, #28789, .F. ) ;
#6156 = DIRECTION ( 'NONE',  ( 0.000000000000000000, -0.5877852522924797984, 0.8090169943749426773 ) ) ;
#6158 = LINE ( 'NONE', #8825, #4961 ) ;
#6159 = DIRECTION ( 'NONE',  ( -0.000000000000000000, 0.000000000000000000, 1.000000000000000000 ) ) ;
#6160 = EDGE_CURVE ( 'NONE', #21430, #32821, #15112, .T. ) ;
#6161 = VERTEX_POINT ( 'NONE', #13106 ) ;
#6162 = CARTESIAN_POINT ( 'NONE',  ( -4.162942409646514186, -5.022711880624455567E-15, 2.999999999999999556 ) ) ;
#6163 = CARTESIAN_POINT ( 'NONE',  ( 0.5032040285305349192, -3.698073368203369515, 9.002252291025278907 ) ) ;
#6164 = CARTESIAN_POINT ( 'NONE',  ( -32.07659242536668387, -21.93932300455395534, -1.292893218813452538 ) ) ;
#6165 = DIRECTION ( 'NONE',  ( -7.770718973608931818E-17, -0.9063077870366451627, -0.4226182617407097108 ) ) ;
#6166 = DIRECTION ( 'NONE',  ( -1.000000000000000000, -0.000000000000000000, 0.000000000000000000 ) ) ;
#6167 = ORIENTED_EDGE ( 'NONE', *, *, #11202, .T. ) ;
#6168 = LINE ( 'NONE', #16354, #29534 ) ;
#6169 =( BOUNDED_SURFACE ( )  B_SPLINE_SURFACE ( 1, 2, ( 
 ( #14826, #29738, #25025, #14984, #25204, #17004, #27206, #2140, #4318, #2327, #22715, #14496, #1990, #17182, #4505, #12163, #22361, #26156, #8427, #12659, #20983, #31203, #3263, #18620, #17860, #920, #11098, #5911, #15330, #22862, #33064, #15178, #28815, #28667, #7468, #3442, #26004, #3112, #7661, #27880, #8282, #10949, #30578, #18475, #13425, #20198, #2490, #21151, #13267, #20360, #15941, #5155, #28058, #23471, #580, #16104, #31350, #26336, #13601, #17668, #25382, #10769, #23806, #9987, #5762, #32918, #23644, #767, #30394, #4994, #10139, #23271, #24636, #10399, #12883, #7104, #17926, #7883, #28117, #1767, #24974 ),
 ( #12262, #2708, #374, #20609, #9771, #10548, #2087, #11962, #30815, #7734, #32521, #22472, #19646, #18075, #29685, #9583, #6764, #19803, #15391, #22159, #32689, #23102, #24821, #19993, #25599, #16954, #29840, #223, #17305, #14620, #5215, #30011, #27501, #4601, #14776, #5375, #28268, #15563, #25780, #32370, #9429, #30657, #13070, #27151, #2907, #4254, #14427, #6917, #17113, #27324, #4444, #1940, #12113, #22310, #3546, #31301, #8523, #31614, #18726, #25948, #16036, #24059, #18917, #13705, #15746, #23906, #1014, #13549, #18570, #11198, #5853, #28452, #8041, #13214, #28762, #10705, #21406, #28930, #26267, #3382, #26448 ) ),
 .UNSPECIFIED., .F., .F., .F. ) 
 B_SPLINE_SURFACE_WITH_KNOTS ( ( 2, 2 ),
 ( 3, 2, 2, 2, 2, 2, 2, 2, 2, 2, 2, 2, 2, 2, 2, 2, 2, 2, 2, 2, 2, 2, 2, 2, 2, 2, 2, 2, 2, 2, 2, 2, 2, 2, 2, 2, 2, 2, 2, 2, 3 ),
 ( 0.000000000000000000, 1.000000000000000000 ),
 ( 0.000000000000000000, 0.02500000000000000139, 0.05000000000000000278, 0.07499999999999999722, 0.1000000000000000056, 0.1250000000000000000, 0.1499999999999999944, 0.1749999999999999889, 0.2000000000000000111, 0.2250000000000000056, 0.2500000000000000000, 0.2750000000000000222, 0.2999999999999999889, 0.3250000000000000111, 0.3499999999999999778, 0.3750000000000000000, 0.4000000000000000222, 0.4249999999999999889, 0.4500000000000000111, 0.4749999999999999778, 0.5000000000000000000, 0.5250000000000000222, 0.5500000000000000444, 0.5749999999999999556, 0.5999999999999999778, 0.6250000000000000000, 0.6500000000000000222, 0.6750000000000000444, 0.6999999999999999556, 0.7249999999999999778, 0.7500000000000000000, 0.7750000000000000222, 0.8000000000000000444, 0.8249999999999999556, 0.8499999999999999778, 0.8750000000000000000, 0.9000000000000000222, 0.9250000000000000444, 0.9499999999999999556, 0.9749999999999999778, 1.000000000000000000 ),
 .UNSPECIFIED. ) 
 GEOMETRIC_REPRESENTATION_ITEM ( )  RATIONAL_B_SPLINE_SURFACE ( (
 ( 1.000000000000000000, 0.9238795325112867385, 1.000000000000000000, 0.9238795325112867385, 1.000000000000000000, 0.9238795325112867385, 1.000000000000000000, 0.9238795325112867385, 1.000000000000000000, 0.9238795325112867385, 1.000000000000000000, 0.9238795325112867385, 1.000000000000000000, 0.9238795325112867385, 1.000000000000000000, 0.9238795325112867385, 1.000000000000000000, 0.9238795325112867385, 1.000000000000000000, 0.9238795325112867385, 1.000000000000000000, 0.9238795325112867385, 1.000000000000000000, 0.9238795325112867385, 1.000000000000000000, 0.9238795325112867385, 1.000000000000000000, 0.9238795325112867385, 1.000000000000000000, 0.9238795325112867385, 1.000000000000000000, 0.9238795325112867385, 1.000000000000000000, 0.9238795325112867385, 1.000000000000000000, 0.9238795325112867385, 1.000000000000000000, 0.9238795325112867385, 1.000000000000000000, 0.9238795325112867385, 1.000000000000000000, 0.9238795325112867385, 1.000000000000000000, 0.9238795325112867385, 1.000000000000000000, 0.9238795325112867385, 1.000000000000000000, 0.9238795325112867385, 1.000000000000000000, 0.9238795325112867385, 1.000000000000000000, 0.9238795325112867385, 1.000000000000000000, 0.9238795325112867385, 1.000000000000000000, 0.9238795325112867385, 1.000000000000000000, 0.9238795325112867385, 1.000000000000000000, 0.9238795325112867385, 1.000000000000000000, 0.9238795325112867385, 1.000000000000000000, 0.9238795325112867385, 1.000000000000000000, 0.9238795325112867385, 1.000000000000000000, 0.9238795325112867385, 1.000000000000000000, 0.9238795325112867385, 1.000000000000000000, 0.9238795325112867385, 1.000000000000000000, 0.9238795325112867385, 1.000000000000000000, 0.9238795325112867385, 1.000000000000000000, 0.9238795325112867385, 1.000000000000000000, 0.9238795325112867385, 1.000000000000000000),
 ( 1.000000000000000000, 0.9238795325112867385, 1.000000000000000000, 0.9238795325112867385, 1.000000000000000000, 0.9238795325112867385, 1.000000000000000000, 0.9238795325112867385, 1.000000000000000000, 0.9238795325112867385, 1.000000000000000000, 0.9238795325112867385, 1.000000000000000000, 0.9238795325112867385, 1.000000000000000000, 0.9238795325112867385, 1.000000000000000000, 0.9238795325112867385, 1.000000000000000000, 0.9238795325112867385, 1.000000000000000000, 0.9238795325112867385, 1.000000000000000000, 0.9238795325112867385, 1.000000000000000000, 0.9238795325112867385, 1.000000000000000000, 0.9238795325112867385, 1.000000000000000000, 0.9238795325112867385, 1.000000000000000000, 0.9238795325112867385, 1.000000000000000000, 0.9238795325112867385, 1.000000000000000000, 0.9238795325112867385, 1.000000000000000000, 0.9238795325112867385, 1.000000000000000000, 0.9238795325112867385, 1.000000000000000000, 0.9238795325112867385, 1.000000000000000000, 0.9238795325112867385, 1.000000000000000000, 0.9238795325112867385, 1.000000000000000000, 0.9238795325112867385, 1.000000000000000000, 0.9238795325112867385, 1.000000000000000000, 0.9238795325112867385, 1.000000000000000000, 0.9238795325112867385, 1.000000000000000000, 0.9238795325112867385, 1.000000000000000000, 0.9238795325112867385, 1.000000000000000000, 0.9238795325112867385, 1.000000000000000000, 0.9238795325112867385, 1.000000000000000000, 0.9238795325112867385, 1.000000000000000000, 0.9238795325112867385, 1.000000000000000000, 0.9238795325112867385, 1.000000000000000000, 0.9238795325112867385, 1.000000000000000000, 0.9238795325112867385, 1.000000000000000000, 0.9238795325112867385, 1.000000000000000000, 0.9238795325112867385, 1.000000000000000000, 0.9238795325112867385, 1.000000000000000000, 0.9238795325112867385, 1.000000000000000000) ) ) 
 REPRESENTATION_ITEM ( '' )  SURFACE ( )  );
#6170 = CARTESIAN_POINT ( 'NONE',  ( -57.38987804550299643, -3.170151398038286938, 5.871858310191695907 ) ) ;
#6171 = CARTESIAN_POINT ( 'NONE',  ( -3.037550801365593856, 1.088641768524161613, 3.675193018007246959 ) ) ;
#6172 = LINE ( 'NONE', #21376, #8707 ) ;
#6173 = CARTESIAN_POINT ( 'NONE',  ( 32.99635089100449648, 0.06958667959534070580, 0.9963508910047327305 ) ) ;
#6174 = VERTEX_POINT ( 'NONE', #409 ) ;
#6175 = FACE_OUTER_BOUND ( 'NONE', #26975, .T. ) ;
#6176 = EDGE_CURVE ( 'NONE', #15051, #24398, #13392, .T. ) ;
#6177 = CC_DESIGN_PERSON_AND_ORGANIZATION_ASSIGNMENT ( #29091, #31114, ( #5241 ) ) ;
#6178 = ORIENTED_EDGE ( 'NONE', *, *, #9343, .F. ) ;
#6179 = PERSON_AND_ORGANIZATION ( #6766, #25292 ) ;
#6180 = CARTESIAN_POINT ( 'NONE',  ( 85.03572474060098330, -5.203290465832886902, 3.995335864764280043 ) ) ;
#6181 = CARTESIAN_POINT ( 'NONE',  ( 108.1300413742128228, -19.95926608421483195, 0.000000000000000000 ) ) ;
#6182 = EDGE_LOOP ( 'NONE', ( #12435, #783, #32029, #23861 ) ) ;
#6183 = DIRECTION ( 'NONE',  ( 0.000000000000000000, 0.000000000000000000, 1.000000000000000000 ) ) ;
#6184 = ORIENTED_EDGE ( 'NONE', *, *, #28994, .F. ) ;
#6185 = ORIENTED_EDGE ( 'NONE', *, *, #26925, .T. ) ;
#6186 = LINE ( 'NONE', #3681, #1773 ) ;
#6187 = CARTESIAN_POINT ( 'NONE',  ( -2.862550801365593145, -0.3701630799359326152, 3.521866450007987037 ) ) ;
#6188 = EDGE_CURVE ( 'NONE', #502, #18404, #23462, .T. ) ;
#6189 = CARTESIAN_POINT ( 'NONE',  ( 10.28480887676917455, -12.81065604946497061, 1.500000000000000000 ) ) ;
#6190 = DIRECTION ( 'NONE',  ( 0.000000000000000000, 0.000000000000000000, -1.000000000000000000 ) ) ;
#6192 = ORIENTED_EDGE ( 'NONE', *, *, #23158, .F. ) ;
#6191 = CARTESIAN_POINT ( 'NONE',  ( 0.08034253656914167041, -5.242601083769347525, 9.429377841196169285 ) ) ;
#6193 = CARTESIAN_POINT ( 'NONE',  ( -7.437550801365595099, -1.088641768524163389, -3.675193018007246071 ) ) ;
#6194 = CYLINDRICAL_SURFACE ( 'NONE', #25112, 8.749000000000002331 ) ;
#6195 = EDGE_CURVE ( 'NONE', #4248, #15236, #23622, .T. ) ;
#6196 = CARTESIAN_POINT ( 'NONE',  ( 11.65793814731733846, -20.33404869677255888, 1.500000000000000444 ) ) ;
#6197 = DIRECTION ( 'NONE',  ( 0.000000000000000000, 0.000000000000000000, 1.000000000000000000 ) ) ;
#6199 = EDGE_LOOP ( 'NONE', ( #28243, #12681, #8835, #16341, #5417, #5250, #23540, #11167, #29877, #32913, #9541, #13840 ) ) ;
#6198 = CARTESIAN_POINT ( 'NONE',  ( 5.175170698068133568, 0.000000000000000000, 5.403836275575642389 ) ) ;
#6200 = DIRECTION ( 'NONE',  ( 1.000000000000000000, -0.000000000000000000, -0.000000000000000000 ) ) ;
#6201 = CARTESIAN_POINT ( 'NONE',  ( -16.60354855507977234, 9.200062826706011165, 1.500000000000000000 ) ) ;
#6202 = CARTESIAN_POINT ( 'NONE',  ( -50.60000000000000142, -10.96966150227468972, 0.9999999999999991118 ) ) ;
#6203 = CARTESIAN_POINT ( 'NONE',  ( -3.817249540146987474, -10.46527866769224424, -1.500000000000000000 ) ) ;
#6204 = CARTESIAN_POINT ( 'NONE',  ( 0.000000000000000000, -9.915734732513184824, -4.762163868918376508 ) ) ;
#6205 = CARTESIAN_POINT ( 'NONE',  ( 9.292237988713592856, 0.2314288474955234209, 1.048307530264791287 ) ) ;
#6206 = CARTESIAN_POINT ( 'NONE',  ( 107.8102081147311821, -16.09624553401233271, 1.444131124663140309 ) ) ;
#6207 = ORIENTED_EDGE ( 'NONE', *, *, #1258, .T. ) ;
#6208 = B_SPLINE_CURVE_WITH_KNOTS ( 'NONE', 3,
 ( #25661, #12624, #22828, #13125, #2782, #23177, #33032, #10105, #20324, #30533 ),
 .UNSPECIFIED., .F., .F.,
 ( 4, 2, 2, 2, 4 ),
 ( 1.968338519012285402E-07, 0.0005467926089500459250, 0.001093388384048190644, 0.001639984159146335363, 0.002186579934244480081 ),
 .UNSPECIFIED. ) ;
#6209 = CARTESIAN_POINT ( 'NONE',  ( 18.68429645396846439, -21.55436976724084275, 1.490931396286530042 ) ) ;
#6210 = CARTESIAN_POINT ( 'NONE',  ( 68.79832465278707332, -7.861404707910025991, -0.07017451552783410262 ) ) ;
#6212 = CARTESIAN_POINT ( 'NONE',  ( 5.612974384376776982, -7.213266193303285334, 3.934067627273179824 ) ) ;
#6211 = PLANE ( 'NONE',  #5972 ) ;
#6213 = ORIENTED_EDGE ( 'NONE', *, *, #4736, .T. ) ;
#6214 = CARTESIAN_POINT ( 'NONE',  ( 26.08945412691625521, 19.05746434167071612, -1.050000000000000044 ) ) ;
#6215 = ORIENTED_EDGE ( 'NONE', *, *, #32033, .F. ) ;
#6216 = CARTESIAN_POINT ( 'NONE',  ( -7.757304906975409864, -1.062355717592095017, -2.999999999999999556 ) ) ;
#6218 = VERTEX_POINT ( 'NONE', #8892 ) ;
#6217 = CARTESIAN_POINT ( 'NONE',  ( 69.01341435844646810, -4.974009774632454750, -3.999774175339687599 ) ) ;
#6219 = ORIENTED_EDGE ( 'NONE', *, *, #7566, .T. ) ;
#6220 = CARTESIAN_POINT ( 'NONE',  ( 85.45070076415650817, -7.158483446666923378, -2.713652344655543391 ) ) ;
#6221 = EDGE_CURVE ( 'NONE', #23825, #4970, #14906, .T. ) ;
#6222 = EDGE_CURVE ( 'NONE', #136, #5270, #15925, .T. ) ;
#6223 = B_SPLINE_CURVE_WITH_KNOTS ( 'NONE', 3,
 ( #26143, #5899, #23312, #3430 ),
 .UNSPECIFIED., .F., .F.,
 ( 4, 4 ),
 ( 0.000000000000000000, 2.207496373042337949E-08 ),
 .UNSPECIFIED. ) ;
#6224 = LINE ( 'NONE', #16408, #8614 ) ;
#6226 = EDGE_LOOP ( 'NONE', ( #29499, #12856, #19965, #11282 ) ) ;
#6225 = DIRECTION ( 'NONE',  ( 1.224646799147353207E-16, 1.000000000000000000, 0.000000000000000000 ) ) ;
#6227 = CARTESIAN_POINT ( 'NONE',  ( 11.67104222964946558, 3.952383228255008429, -1.500000000000829337 ) ) ;
#6228 = CARTESIAN_POINT ( 'NONE',  ( 25.43628654896041397, -17.54453578616353582, 1.000000000000000000 ) ) ;
#6229 = DIRECTION ( 'NONE',  ( 0.000000000000000000, -0.9271838545667855369, -0.3746065934159163446 ) ) ;
#6230 = CARTESIAN_POINT ( 'NONE',  ( 14.03158388684507152, -14.04624127993173843, -1.499999999999859224 ) ) ;
#6231 = FACE_OUTER_BOUND ( 'NONE', #825, .T. ) ;
#6232 = CARTESIAN_POINT ( 'NONE',  ( -4.956376981307138330, -0.1572233378491221800, 3.000000000000000000 ) ) ;
#6233 = CARTESIAN_POINT ( 'NONE',  ( 2.357329973329943762, 4.593471141847181194, -9.815384016743262663 ) ) ;
#6234 = FACE_BOUND ( 'NONE', #872, .T. ) ;
#6235 = CARTESIAN_POINT ( 'NONE',  ( -4.317168503051449946, -7.715934794172482292, 1.500000000000000000 ) ) ;
#6236 = CARTESIAN_POINT ( 'NONE',  ( 10.55147673363119232, 4.116875700062115229, -2.376879293651021019 ) ) ;
#6237 = VERTEX_POINT ( 'NONE', #16265 ) ;
#6238 = LINE ( 'NONE', #19277, #30602 ) ;
#6239 = CARTESIAN_POINT ( 'NONE',  ( 8.911384905465473238, 0.2172754300402908179, -1.412391582771881371 ) ) ;
#6240 = EDGE_CURVE ( 'NONE', #31647, #29157, #1583, .T. ) ;
#6241 = CARTESIAN_POINT ( 'NONE',  ( 56.97280603064904625, -277.2763395528616002, -566.7009208965738480 ) ) ;
#6242 = ORIENTED_EDGE ( 'NONE', *, *, #4653, .F. ) ;
#6243 = CARTESIAN_POINT ( 'NONE',  ( 25.53161554397954092, -0.8571990387063047612, -2.667681220810584009 ) ) ;
#6244 = CARTESIAN_POINT ( 'NONE',  ( 47.62814091865205768, 23.65599663307499512, -4.612695725900423760 ) ) ;
#6245 = VERTEX_POINT ( 'NONE', #13737 ) ;
#6246 = CARTESIAN_POINT ( 'NONE',  ( 3.326984917281274878, -11.41685861481259678, -1.499999999999999334 ) ) ;
#6247 = DIRECTION ( 'NONE',  ( 1.000000000000000000, 0.000000000000000000, 0.000000000000000000 ) ) ;
#6248 = VERTEX_POINT ( 'NONE', #3901 ) ;
#6249 = EDGE_CURVE ( 'NONE', #32816, #13791, #6919, .T. ) ;
#6250 = ORIENTED_EDGE ( 'NONE', *, *, #17613, .T. ) ;
#6251 = CARTESIAN_POINT ( 'NONE',  ( 25.06773407388217834, -17.47416606015785945, -1.197364706239002485 ) ) ;
#6252 = B_SPLINE_SURFACE_WITH_KNOTS ( 'NONE', 3, 3, ( 
 ( #31773, #3530, #19204, #26573, #1165, #3674, #11031 ),
 ( #24380, #8992, #19052, #16865, #13531, #8505, #13687 ),
 ( #6496, #8683, #1348, #21385, #11522, #16699, #29592 ),
 ( #23740, #6180, #11674, #24040, #11363, #26909, #11180 ),
 ( #29242, #21567, #26725, #6326, #16364, #16513, #18707 ),
 ( #21870, #9158, #19391, #28911, #855, #31595, #23889 ),
 ( #998, #9339, #4164, #25219, #30255, #17196, #4331 ),
 ( #14329, #32587, #19707, #22552, #7178, #7328, #27711 ),
 ( #27566, #4818, #22725, #20059, #32429, #1847, #24887 ),
 ( #6828, #24533, #17518, #22370, #9491, #12336, #14507 ),
 ( #29906, #9659, #6988, #2339, #12519, #29747, #14999 ),
 ( #32279, #17013, #27405, #4514, #32928, #14689, #27216 ),
 ( #24720, #32768, #1999, #9998, #17372, #20210, #19549 ),
 ( #30406, #12172, #25034, #19884, #7479, #30098, #4663 ),
 ( #12025, #1657, #17683, #14835, #11849, #22058, #2149 ),
 ( #9847, #22220, #15499, #3012, #30589, #15191, #20862 ),
 ( #22873, #26051, #23222, #23523, #12818, #12669, #5661 ),
 ( #23035, #2502, #20374, #10152, #33076, #7672, #30765 ),
 ( #15841, #18028, #17874, #25715, #15342, #13165, #20555 ),
 ( #30912, #638, #28068, #25544, #3156, #2841, #15691 ),
 ( #13313, #155, #5320, #10829, #5164, #25392, #21045 ),
 ( #18178, #10341, #31251, #13013, #2651, #7835, #25899 ),
 ( #10653, #28217, #18369, #20713, #8326, #326, #10501 ),
 ( #7987, #5502, #27893, #28386, #23368, #5009, #472 ),
 ( #31073, #8163, #28567, #6292, #13965, #18521, #28714 ),
 ( #13652, #23856, #6148, #29058, #8812, #1460, #18856 ),
 ( #32045, #31737, #21833, #18669, #16330, #19019, #964 ),
 ( #26683, #6446, #24184, #26539, #29203, #21345, #5806 ),
 ( #26397, #23704, #821, #8639, #3979, #10998, #1312 ),
 ( #21199, #31396, #8472, #31551, #11144, #3796, #11487 ),
 ( #28870, #21681, #16477, #8955, #14150, #31889, #3642 ),
 ( #15988, #26210, #5970, #13796, #24001, #1122, #11317 ),
 ( #11638, #21528, #19165, #3319, #29358, #13491, #16166 ),
 ( #16652, #26862, #3495, #24348, #30217, #14802, #19672 ) ),
 .UNSPECIFIED., .F., .F., .F.,
 ( 4, 3, 3, 3, 3, 3, 3, 3, 3, 3, 3, 4 ),
 ( 4, 3, 4 ),
 ( -2.660026849229521048E-11, 0.001953124973451693261, 0.003906249973503654951, 0.007812499973607578765, 0.01562499997381542639, 0.03124999997423111991, 0.06249999997506251043, 0.1249999999767252845, 0.2499999999800508466, 0.4999999999867019707, 0.7499999999933530948, 1.000000000000004219 ),
 ( 0.003589107913147454587, 0.5017945539568872126, 1.000000000000627054 ),
 .UNSPECIFIED. ) ;
#6254 = EDGE_LOOP ( 'NONE', ( #15012, #24088, #20645, #28431 ) ) ;
#6253 = CARTESIAN_POINT ( 'NONE',  ( 22.92250000000000298, 2.378061970571979433, -1.291182301015470602 ) ) ;
#6255 = ORIENTED_EDGE ( 'NONE', *, *, #26381, .F. ) ;
#6256 = DIRECTION ( 'NONE',  ( 0.000000000000000000, 0.000000000000000000, -1.000000000000000000 ) ) ;
#6257 = ORIENTED_EDGE ( 'NONE', *, *, #32044, .F. ) ;
#6258 = CARTESIAN_POINT ( 'NONE',  ( -53.73534286770232882, 4.623678987564122878, 5.128141679950119602 ) ) ;
#6259 = DIRECTION ( 'NONE',  ( -0.000000000000000000, -0.000000000000000000, 1.000000000000000000 ) ) ;
#6261 = VERTEX_POINT ( 'NONE', #31659 ) ;
#6260 = CARTESIAN_POINT ( 'NONE',  ( 84.85832005755730734, -2.331047133796637638, -0.4367664088709692360 ) ) ;
#6262 = DIRECTION ( 'NONE',  ( -1.000000000000000000, 0.000000000000000000, 0.000000000000000000 ) ) ;
#6263 = EDGE_CURVE ( 'NONE', #2976, #10851, #25616, .T. ) ;
#6264 = CARTESIAN_POINT ( 'NONE',  ( 101.8016823592330127, -4.042758964360499974, 3.993434276137187489 ) ) ;
#6265 = CARTESIAN_POINT ( 'NONE',  ( 7.249760686538667009, 5.064320921489820826, 7.135485519862015735 ) ) ;
#6266 = DIRECTION ( 'NONE',  ( 1.000000000000000000, 0.000000000000000000, 0.000000000000000000 ) ) ;
#6267 = B_SPLINE_CURVE_WITH_KNOTS ( 'NONE', 3,
 ( #26806, #26637, #9249, #24446, #21950, #24610 ),
 .UNSPECIFIED., .F., .F.,
 ( 4, 2, 4 ),
 ( 0.000000000000000000, 0.0008472833942745525669, 0.001694566788549105134 ),
 .UNSPECIFIED. ) ;
#6268 = DIRECTION ( 'NONE',  ( 0.000000000000000000, -0.9271838545667856479, -0.3746065934159163446 ) ) ;
#6269 = ADVANCED_FACE ( 'NONE', ( #5746 ), #10781, .F. ) ;
#6270 = CARTESIAN_POINT ( 'NONE',  ( 29.18336473368350426, -8.306880066003914820, -0.4367664981582846662 ) ) ;
#6271 = SPHERICAL_SURFACE ( 'NONE', #32837, 0.5000000000000000000 ) ;
#6272 = CARTESIAN_POINT ( 'NONE',  ( 1.624999999999999778, 9.915734732513218574, 4.762163868918307230 ) ) ;
#6273 = DIRECTION ( 'NONE',  ( 0.000000000000000000, 0.000000000000000000, 1.000000000000000000 ) ) ;
#6274 = DIRECTION ( 'NONE',  ( -0.000000000000000000, 0.000000000000000000, 1.000000000000000000 ) ) ;
#6275 = DIRECTION ( 'NONE',  ( 1.000000000000000000, -0.000000000000000000, -0.000000000000000000 ) ) ;
#6276 = EDGE_CURVE ( 'NONE', #4235, #3463, #11568, .T. ) ;
#6277 = CARTESIAN_POINT ( 'NONE',  ( -50.60000000000000142, -10.96966150227468972, 7.500000000000000000 ) ) ;
#6278 = CARTESIAN_POINT ( 'NONE',  ( -6.450050802731187360, -2.331437884370912705, 1.887961173149512062 ) ) ;
#6279 = ORIENTED_EDGE ( 'NONE', *, *, #21148, .T. ) ;
#6280 = CARTESIAN_POINT ( 'NONE',  ( -5.250050800000000351, 1.549418761218566143, -2.853674364686379583 ) ) ;
#6281 = ADVANCED_FACE ( 'NONE', ( #32151 ), #1903, .T. ) ;
#6282 = CARTESIAN_POINT ( 'NONE',  ( -5.304000690461529555E-12, -21.43932300456189566, -1.000000000000000000 ) ) ;
#6283 = DIRECTION ( 'NONE',  ( 0.000000000000000000, -0.9945218953682734009, -0.1045284632676536235 ) ) ;
#6284 = PLANE ( 'NONE',  #12991 ) ;
#6285 = EDGE_LOOP ( 'NONE', ( #1010, #17292, #22304, #19082 ) ) ;
#6286 = CARTESIAN_POINT ( 'NONE',  ( -7.250050800000000351, -1.549418761218565255, 2.853674364686380471 ) ) ;
#6287 = ORIENTED_EDGE ( 'NONE', *, *, #9385, .F. ) ;
#6288 = CARTESIAN_POINT ( 'NONE',  ( 0.5290760861564465234, -6.525414595377379889, 1.500000000000000000 ) ) ;
#6289 = CALENDAR_DATE ( 2026, 6, 10 ) ;
#6291 = EDGE_CURVE ( 'NONE', #7973, #32003, #20805, .T. ) ;
#6290 = EDGE_LOOP ( 'NONE', ( #15803, #2977, #2135, #2110, #21636 ) ) ;
#6292 = CARTESIAN_POINT ( 'NONE',  ( 54.97099024849422477, -6.281314660089699409, 4.215290387836660990 ) ) ;
#6293 = EDGE_CURVE ( 'NONE', #2704, #19221, #4564, .T. ) ;
#6294 = CARTESIAN_POINT ( 'NONE',  ( -6.100050799999999995, 0.3135853898029611342, -2.983565686104819648 ) ) ;
#6295 = CARTESIAN_POINT ( 'NONE',  ( 54.95170718585931979, -5.584587902124617642, -4.215290387841124975 ) ) ;
#6296 = DIRECTION ( 'NONE',  ( 0.000000000000000000, 1.000000000000000000, 0.000000000000000000 ) ) ;
#6297 = CARTESIAN_POINT ( 'NONE',  ( 2.357330042320760821, 5.240837896778964833, 9.485534025193812724 ) ) ;
#6298 = ORIENTED_EDGE ( 'NONE', *, *, #13974, .T. ) ;
#6299 = CARTESIAN_POINT ( 'NONE',  ( 8.950995676490906661, 0.000000000000000000, 1.008084992930269541 ) ) ;
#6300 = DIRECTION ( 'NONE',  ( 0.7895257206258718963, 0.6137174728408810731, 0.000000000000000000 ) ) ;
#6301 = ORIENTED_EDGE ( 'NONE', *, *, #3519, .T. ) ;
#6302 = LINE ( 'NONE', #16490, #718 ) ;
#6303 = B_SPLINE_CURVE_WITH_KNOTS ( 'NONE', 3,
 ( #28877, #10840, #29212, #8332, #13660, #21353, #971, #26547 ),
 .UNSPECIFIED., .F., .F.,
 ( 4, 2, 2, 4 ),
 ( 2.024520226885745157E-07, 0.001227962984611326042, 0.001841843250905642743, 0.002455723517199959443 ),
 .UNSPECIFIED. ) ;
#6304 = FACE_OUTER_BOUND ( 'NONE', #32273, .T. ) ;
#6305 = CARTESIAN_POINT ( 'NONE',  ( 2.864530965498449433, -2.320611941139863355, -9.276519854389901454 ) ) ;
#6306 = CARTESIAN_POINT ( 'NONE',  ( 4.749760686538667009, 6.940565734314597002, 4.007137495034836405 ) ) ;
#6307 = ADVANCED_FACE ( 'NONE', ( #14887 ), #19756, .T. ) ;
#6308 = LINE ( 'NONE', #24019, #14509 ) ;
#6309 = LINE ( 'NONE', #24020, #4873 ) ;
#6310 = DIRECTION ( 'NONE',  ( 0.000000000000000000, -0.000000000000000000, -1.000000000000000000 ) ) ;
#6311 = CARTESIAN_POINT ( 'NONE',  ( 72.72614267423888634, -20.12349919362671358, 5.485967528433933538 ) ) ;
#6312 = EDGE_LOOP ( 'NONE', ( #4669, #6432, #13345, #9011 ) ) ;
#6313 = LINE ( 'NONE', #16006, #20479 ) ;
#6314 = VERTEX_POINT ( 'NONE', #7052 ) ;
#6315 = CARTESIAN_POINT ( 'NONE',  ( 8.870145747188287189, 0.000000000000000000, -1.000000000000000000 ) ) ;
#6316 = CARTESIAN_POINT ( 'NONE',  ( -59.40947820539835789, -5.253841109363955653, 5.268872846900772622 ) ) ;
#6317 = CARTESIAN_POINT ( 'NONE',  ( -2.487550801365593589, 2.752080473201636845, -2.228590825266444142 ) ) ;
#6318 = CARTESIAN_POINT ( 'NONE',  ( 0.000000000000000000, 1.239665997527021002, -9.314797388894877628 ) ) ;
#6319 = CARTESIAN_POINT ( 'NONE',  ( 55.00869849602042905, -7.632537969515627019, 2.184956776156973035 ) ) ;
#6320 = ORIENTED_EDGE ( 'NONE', *, *, #15706, .T. ) ;
#6321 = CARTESIAN_POINT ( 'NONE',  ( 7.249760686538667009, 1.391664247347228045, 7.892520144992438702 ) ) ;
#6322 = ADVANCED_FACE ( 'NONE', ( #14380 ), #4066, .F. ) ;
#6323 = EDGE_LOOP ( 'NONE', ( #1710, #30315, #17140, #14867, #8014 ) ) ;
#6324 = COORDINATED_UNIVERSAL_TIME_OFFSET ( 0, 0, .AHEAD. ) ;
#6325 = ADVANCED_FACE ( 'NONE', ( #4210 ), #2095, .T. ) ;
#6326 = CARTESIAN_POINT ( 'NONE',  ( 54.97717972842301748, -6.504952610483546671, 3.995970705059755268 ) ) ;
#6327 = EDGE_CURVE ( 'NONE', #23697, #11749, #6563, .T. ) ;
#6328 = LINE ( 'NONE', #11675, #14940 ) ;
#6329 = VERTEX_POINT ( 'NONE', #4718 ) ;
#6330 = CARTESIAN_POINT ( 'NONE',  ( 109.7266016284592069, 16.47760998941509669, -5.471072653611049219 ) ) ;
#6331 = VERTEX_POINT ( 'NONE', #24781 ) ;
#6332 = EDGE_LOOP ( 'NONE', ( #31353, #3695, #14727 ) ) ;
#6333 = CARTESIAN_POINT ( 'NONE',  ( 0.8407900506754626413, -11.56055812333295130, -4.522129901861164925 ) ) ;
#6334 = CARTESIAN_POINT ( 'NONE',  ( -4.762550801365593500, 2.752080473201636845, -2.228590825266444142 ) ) ;
#6335 = CARTESIAN_POINT ( 'NONE',  ( 25.29749999999999943, -0.7685399846772070775, 2.594547506269381465 ) ) ;
#6336 = CARTESIAN_POINT ( 'NONE',  ( 3.063284526845908129, -0.4999240074859571670, -8.734705317652709411 ) ) ;
#6338 = ORIENTED_EDGE ( 'NONE', *, *, #27124, .F. ) ;
#6337 = DIRECTION ( 'NONE',  ( -1.000000000000000000, -0.000000000000000000, -0.000000000000000000 ) ) ;
#6339 = CARTESIAN_POINT ( 'NONE',  ( -8.137550801365593500, 1.828967928396027176, -3.368539882008727115 ) ) ;
#6340 = CARTESIAN_POINT ( 'NONE',  ( 10.55147673363118876, -2.285372942704986698, 4.458382051008185520 ) ) ;
#6341 = CARTESIAN_POINT ( 'NONE',  ( 15.90621216620982281, -21.21021934853489910, 1.499999999999999112 ) ) ;
#6342 = FACE_OUTER_BOUND ( 'NONE', #8492, .T. ) ;
#6343 = ORIENTED_EDGE ( 'NONE', *, *, #4689, .T. ) ;
#6345 = VERTEX_POINT ( 'NONE', #1718 ) ;
#6344 = CARTESIAN_POINT ( 'NONE',  ( 13.44361105969346504, 21.88231906142583938, 1.272599291342047190 ) ) ;
#6346 = EDGE_CURVE ( 'NONE', #8252, #22534, #634, .T. ) ;
#6347 = APPROVAL ( #27892, 'UNSPECIFIED' ) ;
#6348 = CARTESIAN_POINT ( 'NONE',  ( 20.54750000273118715, -0.7685399846772070775, 2.594547506269381465 ) ) ;
#6349 = LINE ( 'NONE', #3212, #28430 ) ;
#6350 = FACE_OUTER_BOUND ( 'NONE', #10147, .T. ) ;
#6351 = CARTESIAN_POINT ( 'NONE',  ( -4.125275233336413550, -7.575318389262013064, -1.744514813436137235 ) ) ;
#6352 = CARTESIAN_POINT ( 'NONE',  ( 0.7632845268398873451, -5.538577986808840059, -6.772677083992440394 ) ) ;
#6353 = DIRECTION ( 'NONE',  ( -1.000000000000000000, -0.000000000000000000, -0.000000000000000000 ) ) ;
#6354 = CARTESIAN_POINT ( 'NONE',  ( 2.632061376486628301, -0.4999999999999997780, -1.949999999999999956 ) ) ;
#6355 = ORIENTED_EDGE ( 'NONE', *, *, #15919, .T. ) ;
#6356 = EDGE_CURVE ( 'NONE', #22691, #25765, #3198, .T. ) ;
#6357 = CARTESIAN_POINT ( 'NONE',  ( 20.69942760064479259, -21.74528614261434711, 1.396244390126957224 ) ) ;
#6358 = B_SPLINE_CURVE_WITH_KNOTS ( 'NONE', 3,
 ( #32686, #14269, #9767, #4441, #2256, #14618, #19491, #24464, #11769, #24819, #29683, #1938, #12110, #22308, #28497, #7590, #30507, #2588 ),
 .UNSPECIFIED., .F., .F.,
 ( 4, 2, 2, 2, 2, 2, 2, 2, 4 ),
 ( 0.000000000000000000, 0.0003646863777415453706, 0.0005470295666123181372, 0.0006382011610477136008, 0.0006837869582654212530, 0.0007065798568742751333, 0.0007179763061787019108, 0.0007236745308309153538, 0.0007293727554831286883 ),
 .UNSPECIFIED. ) ;
#6359 = DIRECTION ( 'NONE',  ( 0.1908089953765452762, 0.000000000000000000, 0.9816271834476639757 ) ) ;
#6361 = CARTESIAN_POINT ( 'NONE',  ( 21.08401840680159367, -16.78474387324287775, 1.500000000000000000 ) ) ;
#6360 = CARTESIAN_POINT ( 'NONE',  ( -23.35000000000000142, -10.96966150227469505, 4.500000000000000888 ) ) ;
#6362 = ORIENTED_EDGE ( 'NONE', *, *, #9891, .F. ) ;
#6363 = AXIS2_PLACEMENT_3D ( 'NONE', #444, #26024, #15311 ) ;
#6364 = CARTESIAN_POINT ( 'NONE',  ( 3.063284526839887167, -7.360373001730951437, 4.729683950898845524 ) ) ;
#6365 = ORIENTED_EDGE ( 'NONE', *, *, #13487, .T. ) ;
#6366 =( BOUNDED_CURVE ( )  B_SPLINE_CURVE ( 2, ( #15963, #13291, #5787, #20835, #3471, #26365, #11121, #23497, #31049, #5470, #15822 ),
 .UNSPECIFIED., .F., .F. ) 
 B_SPLINE_CURVE_WITH_KNOTS ( ( 3, 2, 2, 2, 2, 3 ),
 ( 0.6853822619934377691, 0.6875000000000000000, 0.7031250000000000000, 0.7187500000000000000, 0.7343750000000000000, 0.7478822619934377691 ),
 .UNSPECIFIED. ) 
 CURVE ( )  GEOMETRIC_REPRESENTATION_ITEM ( )  RATIONAL_B_SPLINE_CURVE ( ( 0.9821626249036861100, 0.9896829947469995004, 1.000000000000000000, 0.9238795325112867385, 1.000000000000000000, 0.9238795325112867385, 1.000000000000000000, 0.9238795325112867385, 1.000000000000000000, 0.9341965377642872381, 0.9821626249036861100 ) ) 
 REPRESENTATION_ITEM ( '' )  );
#6367 = CARTESIAN_POINT ( 'NONE',  ( -38.14293509397969473, 10.97000000000000419, 1.050000000000000044 ) ) ;
#6369 = ORIENTED_EDGE ( 'NONE', *, *, #8526, .T. ) ;
#6368 = CARTESIAN_POINT ( 'NONE',  ( 40.87773644913306015, -5.749500242219811597, -3.994702139305111199 ) ) ;
#6370 = VERTEX_POINT ( 'NONE', #23100 ) ;
#6371 = CARTESIAN_POINT ( 'NONE',  ( 7.249760686538667009, 0.000000000000000000, 0.000000000000000000 ) ) ;
#6372 = LINE ( 'NONE', #1542, #28387 ) ;
#6374 = EDGE_LOOP ( 'NONE', ( #2751, #18604, #17302 ) ) ;
#6373 = DIRECTION ( 'NONE',  ( 0.2880220749472559572, 0.1662896225033555220, -0.9430753128943462071 ) ) ;
#6375 = CARTESIAN_POINT ( 'NONE',  ( 18.71251328246767898, 14.89923106884208615, -1.500000000000000000 ) ) ;
#6376 = CARTESIAN_POINT ( 'NONE',  ( -4.121060316658296863, -7.626742303306310866, -1.744488848298825223 ) ) ;
#6377 = DIRECTION ( 'NONE',  ( 0.1027947991993876792, -0.9947025833170222153, 0.000000000000000000 ) ) ;
#6378 = CARTESIAN_POINT ( 'NONE',  ( 9.555580689062686872, -12.32072190999758021, -1.500000000000000000 ) ) ;
#6380 = ORIENTED_EDGE ( 'NONE', *, *, #31638, .F. ) ;
#6379 = CARTESIAN_POINT ( 'NONE',  ( -3.150050802731187538, -2.983565686104819648, -0.3135853898029605791 ) ) ;
#6381 = CARTESIAN_POINT ( 'NONE',  ( -4.650050802731187538, -1.887961173149512062, -2.331437884370912261 ) ) ;
#6382 = AXIS2_PLACEMENT_3D ( 'NONE', #27586, #4686, #2173 ) ;
#6383 = CIRCLE ( 'NONE', #14362, 302.4235430809786749 ) ;
#6384 = CARTESIAN_POINT ( 'NONE',  ( 24.79750000273118715, -2.594547506269383685, -0.7685399846772043020 ) ) ;
#6385 = LINE ( 'NONE', #14241, #29626 ) ;
#6386 = CARTESIAN_POINT ( 'NONE',  ( -2.386718424894567203, -9.330009425478154483, 4.522129901861158707 ) ) ;
#6387 = CARTESIAN_POINT ( 'NONE',  ( -1.348815490713419493E-16, -7.533794289458111137, 7.944914065997086716 ) ) ;
#6388 = CIRCLE ( 'NONE', #15463, 6.248999999999999666 ) ;
#6389 = ORIENTED_EDGE ( 'NONE', *, *, #8164, .F. ) ;
#6390 = DIRECTION ( 'NONE',  ( 0.000000000000000000, 0.000000000000000000, -1.000000000000000000 ) ) ;
#6391 = CARTESIAN_POINT ( 'NONE',  ( 107.4223672430906049, -16.96176113054595547, -3.705237567694021461 ) ) ;
#6392 = EDGE_CURVE ( 'NONE', #1933, #9859, #5150, .T. ) ;
#6393 = CARTESIAN_POINT ( 'NONE',  ( -8.000050800000000351, 0.000000000000000000, 0.000000000000000000 ) ) ;
#6394 = ORIENTED_EDGE ( 'NONE', *, *, #6747, .T. ) ;
#6395 = EDGE_CURVE ( 'NONE', #23529, #685, #12844, .T. ) ;
#6396 = EDGE_CURVE ( 'NONE', #8403, #17832, #21403, .T. ) ;
#6397 = DIRECTION ( 'NONE',  ( 1.000000000000000000, 0.000000000000000000, 0.000000000000000000 ) ) ;
#6398 = CARTESIAN_POINT ( 'NONE',  ( 21.19329141388233850, -21.80292992253813367, -1.345625751489397226 ) ) ;
#6399 = ORIENTED_EDGE ( 'NONE', *, *, #6641, .F. ) ;
#6400 = PLANE ( 'NONE',  #12889 ) ;
#6401 = ORIENTED_EDGE ( 'NONE', *, *, #11590, .T. ) ;
#6402 = AXIS2_PLACEMENT_3D ( 'NONE', #25991, #32558, #15430 ) ;
#6403 = VECTOR ( 'NONE', #25512, 1000.000000000000000 ) ;
#6404 = ORIENTED_EDGE ( 'NONE', *, *, #16688, .T. ) ;
#6405 = B_SPLINE_CURVE_WITH_KNOTS ( 'NONE', 3,
 ( #10229, #2562, #5226, #19964, #14899, #27629, #25104, #12409, #19769, #10058 ),
 .UNSPECIFIED., .F., .F.,
 ( 4, 2, 2, 2, 4 ),
 ( 1.387948177032400748E-17, 0.002010218194407704159, 0.003015327291611544312, 0.003517881840213458750, 0.004020436388815372755 ),
 .UNSPECIFIED. ) ;
#6406 = CARTESIAN_POINT ( 'NONE',  ( 25.42756288599143133, -17.55292975162308267, -1.197473197311734294 ) ) ;
#6408 = ORIENTED_EDGE ( 'NONE', *, *, #15769, .F. ) ;
#6407 = DIRECTION ( 'NONE',  ( -0.4999999999999982236, -0.8660254037844397068, 0.000000000000000000 ) ) ;
#6409 = ORIENTED_EDGE ( 'NONE', *, *, #29164, .T. ) ;
#6410 = DIRECTION ( 'NONE',  ( -1.000000000000000000, 0.000000000000000000, -0.000000000000000000 ) ) ;
#6411 = ORIENTED_EDGE ( 'NONE', *, *, #11165, .T. ) ;
#6413 = VECTOR ( 'NONE', #24203, 1000.000000000000000 ) ;
#6412 = CARTESIAN_POINT ( 'NONE',  ( 13.41780342409107973, 19.07609913100965571, 4.629213727441584325 ) ) ;
#6414 = DIRECTION ( 'NONE',  ( -0.000000000000000000, -0.000000000000000000, -1.000000000000000000 ) ) ;
#6416 = ORIENTED_EDGE ( 'NONE', *, *, #8751, .F. ) ;
#6415 = CARTESIAN_POINT ( 'NONE',  ( -2.319264028778656339, 1.051699019630317755, 3.241526370156308623 ) ) ;
#6417 = CARTESIAN_POINT ( 'NONE',  ( -50.60000000000000142, -10.96966150227468972, 1.500000000000000000 ) ) ;
#6418 = DIRECTION ( 'NONE',  ( -1.000000000000000000, 0.000000000000000000, 0.000000000000000000 ) ) ;
#6419 = CARTESIAN_POINT ( 'NONE',  ( -56.77528804678861007, 0.4484486523079136977, 1.857590217363785712 ) ) ;
#6420 = CARTESIAN_POINT ( 'NONE',  ( 10.56183597391177464, 4.888740217817763464E-14, -4.753758587302147731 ) ) ;
#6421 = CARTESIAN_POINT ( 'NONE',  ( 108.0282448396077797, -18.47608078053866265, 4.361986266605526907 ) ) ;
#6422 = AXIS2_PLACEMENT_3D ( 'NONE', #16555, #29446, #24267 ) ;
#6423 = CARTESIAN_POINT ( 'NONE',  ( 3.499999999999999556, -5.349675154362342866, 3.229702268444914370 ) ) ;
#6424 = CARTESIAN_POINT ( 'NONE',  ( 55.02542983044660474, -8.237060396196271839, -0.07017451552783633695 ) ) ;
#6425 = FACE_OUTER_BOUND ( 'NONE', #5285, .T. ) ;
#6426 = AXIS2_PLACEMENT_3D ( 'NONE', #11986, #11800, #6790 ) ;
#6427 = EDGE_CURVE ( 'NONE', #6020, #10425, #15061, .T. ) ;
#6428 = LINE ( 'NONE', #3477, #3821 ) ;
#6429 = DIRECTION ( 'NONE',  ( -1.000000000000000000, 0.000000000000000000, 0.000000000000000000 ) ) ;
#6430 = DIRECTION ( 'NONE',  ( 2.219124775574899835E-17, 0.2588190451025176309, 0.9659258262890692004 ) ) ;
#6431 = CARTESIAN_POINT ( 'NONE',  ( -6.050050802731187893, 2.331437884370912705, -1.887961173149511618 ) ) ;
#6432 = ORIENTED_EDGE ( 'NONE', *, *, #22454, .T. ) ;
#6433 = CARTESIAN_POINT ( 'NONE',  ( -5.950050799999999640, 3.113457007523260156, -0.9222479816126439855 ) ) ;
#6434 = AXIS2_PLACEMENT_3D ( 'NONE', #21756, #4053, #19249 ) ;
#6435 = DIRECTION ( 'NONE',  ( 0.000000000000000000, -0.9063077870366448296, -0.4226182617407104325 ) ) ;
#6436 = CARTESIAN_POINT ( 'NONE',  ( -5.700050802731187360, -1.549418761218565255, 2.853674364686380471 ) ) ;
#6437 = CARTESIAN_POINT ( 'NONE',  ( 7.166310626577053533, -7.340520188511631794, 1.000000000000000000 ) ) ;
#6438 = ORIENTED_EDGE ( 'NONE', *, *, #26427, .T. ) ;
#6439 = CARTESIAN_POINT ( 'NONE',  ( 21.08401840680096129, -16.78474387324269657, -1.500000000000000000 ) ) ;
#6440 = VERTEX_POINT ( 'NONE', #20260 ) ;
#6441 = CARTESIAN_POINT ( 'NONE',  ( 2.820807997218022223, -11.54323945762161507, 1.759797141769505968 ) ) ;
#6442 = APPROVAL_STATUS ( 'not_yet_approved' ) ;
#6443 = CIRCLE ( 'NONE', #27293, 4.999999999999999112 ) ;
#6444 = CARTESIAN_POINT ( 'NONE',  ( -3.936147556303791983, 18.00000000000000355, 4.854816414140053382 ) ) ;
#6445 = ORIENTED_EDGE ( 'NONE', *, *, #17263, .T. ) ;
#6446 = CARTESIAN_POINT ( 'NONE',  ( 85.00069437095692138, -4.631723123801140041, 4.312042181584448741 ) ) ;
#6447 = AXIS2_PLACEMENT_3D ( 'NONE', #11015, #21216, #31909 ) ;
#6448 = AXIS2_PLACEMENT_3D ( 'NONE', #32392, #9451, #16650 ) ;
#6449 = CYLINDRICAL_SURFACE ( 'NONE', #9090, 5.010000000000000675 ) ;
#6450 = CARTESIAN_POINT ( 'NONE',  ( 102.3479907709230616, -2.912778821759231196, -4.073741746338383152 ) ) ;
#6451 = VECTOR ( 'NONE', #30735, 999.9999999999998863 ) ;
#6452 = CARTESIAN_POINT ( 'NONE',  ( 24.09939086539479192, -17.43210107469705861, -1.523452847364070939 ) ) ;
#6453 = DIRECTION ( 'NONE',  ( -1.000000000000000000, 0.000000000000000000, -0.000000000000000000 ) ) ;
#6454 = VERTEX_POINT ( 'NONE', #17747 ) ;
#6455 = ADVANCED_FACE ( 'NONE', ( #27956 ), #5061, .F. ) ;
#6456 = CARTESIAN_POINT ( 'NONE',  ( 23.07496354194262977, -21.92049040218789457, -1.202267097226756176 ) ) ;
#6457 = CARTESIAN_POINT ( 'NONE',  ( 3.063284526839887167, -5.538577986808947529, 6.772677083992368452 ) ) ;
#6458 = CARTESIAN_POINT ( 'NONE',  ( 5.612718622971682336, -7.650113768151195259, 2.996580135471498707 ) ) ;
#6459 = AXIS2_PLACEMENT_3D ( 'NONE', #20291, #28297, #258 ) ;
#6461 = ORIENTED_EDGE ( 'NONE', *, *, #25064, .T. ) ;
#6460 = DIRECTION ( 'NONE',  ( 0.000000000000000000, -0.2588190451025240701, -0.9659258262890673130 ) ) ;
#6462 = CARTESIAN_POINT ( 'NONE',  ( -3.912550801365593856, 3.675193018007247403, -1.088641768524161391 ) ) ;
#6463 = ADVANCED_FACE ( 'NONE', ( #25441 ), #2208, .F. ) ;
#6464 = DIRECTION ( 'NONE',  ( 0.000000000000000000, 0.000000000000000000, 1.000000000000000000 ) ) ;
#6465 = CARTESIAN_POINT ( 'NONE',  ( 7.249760686538667009, -3.748318449932238838, -7.906491560603703839 ) ) ;
#6466 = DIRECTION ( 'NONE',  ( 0.000000000000000000, -0.9063077870366551547, 0.4226182617406882835 ) ) ;
#6467 = LINE ( 'NONE', #10898, #4504 ) ;
#6468 = B_SPLINE_CURVE_WITH_KNOTS ( 'NONE', 3,
 ( #5103, #15279, #12934, #25481, #23156, #562 ),
 .UNSPECIFIED., .F., .F.,
 ( 4, 2, 4 ),
 ( 5.099451029765178191E-07, 0.0008274240357315270017, 0.001654338126360077339 ),
 .UNSPECIFIED. ) ;
#6469 = DIRECTION ( 'NONE',  ( -0.000000000000000000, -0.000000000000000000, -1.000000000000000000 ) ) ;
#6470 = CARTESIAN_POINT ( 'NONE',  ( 25.43628654896337693, -17.54453578616444176, -1.000000000000000000 ) ) ;
#6471 = CARTESIAN_POINT ( 'NONE',  ( 10.52034268205830259, -3.055657119358826446, 3.641590349731918863 ) ) ;
#6472 = CARTESIAN_POINT ( 'NONE',  ( 110.4915906369627123, -18.78144465615450187, 4.522129901861159595 ) ) ;
#6473 = B_SPLINE_CURVE_WITH_KNOTS ( 'NONE', 3,
 ( #22080, #9358, #32108, #9184, #27236, #19568, #29764, #22239 ),
 .UNSPECIFIED., .F., .F.,
 ( 4, 2, 2, 4 ),
 ( 0.000000000000000000, 0.0003683317334693677692, 0.0007366634669387355384, 0.001473326933877471077 ),
 .UNSPECIFIED. ) ;
#6474 = ORIENTED_EDGE ( 'NONE', *, *, #612, .T. ) ;
#6475 = AXIS2_PLACEMENT_3D ( 'NONE', #3583, #13743, #3433 ) ;
#6476 = ADVANCED_FACE ( 'NONE', ( #20605 ), #32874, .T. ) ;
#6477 = CIRCLE ( 'NONE', #624, 5.009999999999999787 ) ;
#6478 = ADVANCED_FACE ( 'NONE', ( #18915 ), #6194, .T. ) ;
#6479 = CYLINDRICAL_SURFACE ( 'NONE', #21510, 2.999999999999998224 ) ;
#6480 = VERTEX_POINT ( 'NONE', #29106 ) ;
#6481 = CIRCLE ( 'NONE', #23570, 2.999999999999999556 ) ;
#6482 = DIRECTION ( 'NONE',  ( 2.219124775574819717E-17, 0.2588190451025081940, 0.9659258262890716429 ) ) ;
#6483 = CARTESIAN_POINT ( 'NONE',  ( -2.096054051514731231, 1.210157370878028882, 1.500000000000000000 ) ) ;
#6484 = VECTOR ( 'NONE', #13499, 1000.000000000000227 ) ;
#6485 = CARTESIAN_POINT ( 'NONE',  ( 48.06508596181272708, -7.548662730768715079, -4.522129901861164036 ) ) ;
#6486 = DIRECTION ( 'NONE',  ( 0.000000000000000000, -0.08715574274765383600, -0.9961946980917459893 ) ) ;
#6487 = DIRECTION ( 'NONE',  ( 0.000000000000000000, -0.5877852522924799095, 0.8090169943749425663 ) ) ;
#6488 = CIRCLE ( 'NONE', #28902, 5.000000000000000888 ) ;
#6489 = ORIENTED_EDGE ( 'NONE', *, *, #19908, .F. ) ;
#6490 = CARTESIAN_POINT ( 'NONE',  ( 107.4385791398478744, 17.85938043952739918, -4.612695725900423760 ) ) ;
#6491 = EDGE_CURVE ( 'NONE', #5364, #3782, #574, .T. ) ;
#6492 = VECTOR ( 'NONE', #3500, 1000.000000000000227 ) ;
#6493 = B_SPLINE_CURVE_WITH_KNOTS ( 'NONE', 3,
 ( #7992, #31256, #16336, #3503, #26546, #3328, #3647, #26058 ),
 .UNSPECIFIED., .F., .F.,
 ( 4, 2, 2, 4 ),
 ( 2.737843117574324537E-07, 0.001228034957219864380, 0.001841915543673917259, 0.002455796130127970572 ),
 .UNSPECIFIED. ) ;
#6494 = ORIENTED_EDGE ( 'NONE', *, *, #31084, .T. ) ;
#6495 = PERSON_AND_ORGANIZATION ( #6766, #25292 ) ;
#6496 = CARTESIAN_POINT ( 'NONE',  ( 102.4232361084521585, -3.998984015183867591, 3.994702627084546709 ) ) ;
#6497 = EDGE_CURVE ( 'NONE', #24814, #29452, #8576, .T. ) ;
#6498 = CARTESIAN_POINT ( 'NONE',  ( -3.762942409646513386, 4.884725290497410777E-15, -2.999999999999999556 ) ) ;
#6499 = ORIENTED_EDGE ( 'NONE', *, *, #20666, .T. ) ;
#6500 = CARTESIAN_POINT ( 'NONE',  ( 5.489321676144491846, 3.969109389279964262, 7.082488557107303961 ) ) ;
#6501 = ORIENTED_EDGE ( 'NONE', *, *, #4515, .T. ) ;
#6502 = AXIS2_PLACEMENT_3D ( 'NONE', #20807, #22971, #5759 ) ;
#6503 = EDGE_LOOP ( 'NONE', ( #11061, #15462, #7917, #22388, #31779, #15868 ) ) ;
#6504 = CARTESIAN_POINT ( 'NONE',  ( 0.3045634671936401361, -0.9829946734953967091, -10.22982953726848621 ) ) ;
#6505 = CARTESIAN_POINT ( 'NONE',  ( -53.35155202832373078, 4.845260731991866798, 5.128141679950118714 ) ) ;
#6506 = AXIS2_PLACEMENT_3D ( 'NONE', #19499, #22317, #4608 ) ;
#6507 = CARTESIAN_POINT ( 'NONE',  ( 23.17250000000000298, 1.291182301015469047, 2.378061970571981654 ) ) ;
#6508 = AXIS2_PLACEMENT_3D ( 'NONE', #11302, #29528, #16634 ) ;
#6509 = CARTESIAN_POINT ( 'NONE',  ( 3.499999999999999556, -5.522688772756441544, 6.461416928141223259 ) ) ;
#6511 = ORIENTED_EDGE ( 'NONE', *, *, #3383, .F. ) ;
#6510 = FACE_OUTER_BOUND ( 'NONE', #29487, .T. ) ;
#6512 = CARTESIAN_POINT ( 'NONE',  ( -6.737550801365594033, -3.368539882008727115, -1.828967928396028064 ) ) ;
#6513 = VECTOR ( 'NONE', #15205, 1000.000000000000000 ) ;
#6514 = CARTESIAN_POINT ( 'NONE',  ( 23.22564588060107482, -21.93932300456764040, -1.000000000000000000 ) ) ;
#6515 = CARTESIAN_POINT ( 'NONE',  ( 26.05774446050081750, 21.87587288138697872, 4.999054092451761022 ) ) ;
#6516 = DIRECTION ( 'NONE',  ( 7.770718973608945377E-17, 0.9063077870366468280, 0.4226182617407062136 ) ) ;
#6517 = AXIS2_PLACEMENT_3D ( 'NONE', #30414, #17693, #22883 ) ;
#6518 = ORIENTED_EDGE ( 'NONE', *, *, #18269, .F. ) ;
#6520 = ORIENTED_EDGE ( 'NONE', *, *, #23890, .T. ) ;
#6519 = DIRECTION ( 'NONE',  ( 0.000000000000000000, -0.9961946980917457672, -0.08715574274765541807 ) ) ;
#6521 = VECTOR ( 'NONE', #30181, 1000.000000000000000 ) ;
#6522 = CARTESIAN_POINT ( 'NONE',  ( 110.2875796713736776, 19.60135708372761343, -5.471072653611063430 ) ) ;
#6523 = CARTESIAN_POINT ( 'NONE',  ( -8.000050800000000351, 3.673940397442060361E-16, 3.000000000000000444 ) ) ;
#6524 = EDGE_CURVE ( 'NONE', #13458, #15872, #17502, .T. ) ;
#6525 = EDGE_CURVE ( 'NONE', #15485, #23867, #32602, .T. ) ;
#6526 = CARTESIAN_POINT ( 'NONE',  ( 25.71477796605635291, 3.113678757437459588, 0.5295765639727612051 ) ) ;
#6527 = CARTESIAN_POINT ( 'NONE',  ( -27.72185742298243838, 17.09829073722480075, 1.500000000000000000 ) ) ;
#6528 = CARTESIAN_POINT ( 'NONE',  ( -4.060002436691794614, -5.088205424081681194, -1.745854636721019260 ) ) ;
#6529 = CARTESIAN_POINT ( 'NONE',  ( -33.81874022276151237, 19.50000000000000000, -1.818740222761504599 ) ) ;
#6530 = B_SPLINE_SURFACE_WITH_KNOTS ( 'NONE', 1, 3, ( 
 ( #30981, #30488, #13235, #18094, #20778, #20467, #7574, #30328 ),
 ( #7757, #17949, #5399, #28136, #5235, #15409, #25620, #2735 ) ),
 .UNSPECIFIED., .F., .F., .F.,
 ( 2, 2 ),
 ( 4, 2, 2, 4 ),
 ( 0.000000000000000000, 1.000000000000000000 ),
 ( 0.000000000000000000, 0.5000000000000000000, 0.7500000000000000000, 1.000000000000000000 ),
 .UNSPECIFIED. ) ;
#6531 = CIRCLE ( 'NONE', #30065, 4.999999999999997335 ) ;
#6532 = AXIS2_PLACEMENT_3D ( 'NONE', #15575, #28125, #7743 ) ;
#6533 = CARTESIAN_POINT ( 'NONE',  ( 102.2410647596616116, -1.384237843926831690, 1.529339869964214671 ) ) ;
#6534 = DIRECTION ( 'NONE',  ( 0.8616149568369098066, -0.5075624751249150357, 0.000000000000000000 ) ) ;
#6535 = ADVANCED_FACE ( 'NONE', ( #7002 ), #29606, .T. ) ;
#6536 = CARTESIAN_POINT ( 'NONE',  ( 23.57316428367446193, -9.051964865574909425, -0.07017451552783579571 ) ) ;
#6537 = ORIENTED_EDGE ( 'NONE', *, *, #14602, .T. ) ;
#6538 = AXIS2_PLACEMENT_3D ( 'NONE', #26147, #8755, #14592 ) ;
#6539 = AXIS2_PLACEMENT_3D ( 'NONE', #1949, #17809, #20155 ) ;
#6540 = DIRECTION ( 'NONE',  ( -1.000000000000000000, -0.000000000000000000, 0.000000000000000000 ) ) ;
#6541 = VECTOR ( 'NONE', #370, 1000.000000000000000 ) ;
#6542 = CARTESIAN_POINT ( 'NONE',  ( 4.716257286563768858, 19.50000000000000000, 4.924645716438879717 ) ) ;
#6545 = CARTESIAN_POINT ( 'NONE',  ( 6.038145208238973716, -7.553619661406936636, 3.842870190353671944 ) ) ;
#6544 = CARTESIAN_POINT ( 'NONE',  ( 6.524595126109739240, 2.112519041817613630, 8.397268106035218338 ) ) ;
#6543 = AXIS2_PLACEMENT_3D ( 'NONE', #22593, #20093, #30285 ) ;
#6546 = VERTEX_POINT ( 'NONE', #6514 ) ;
#6547 = CIRCLE ( 'NONE', #16162, 10.99999999999999822 ) ;
#6548 = EDGE_CURVE ( 'NONE', #22217, #28781, #5905, .T. ) ;
#6549 = B_SPLINE_CURVE_WITH_KNOTS ( 'NONE', 3,
 ( #7968, #30746, #20352, #31233, #15670, #15826, #10128, #20694, #5145, #31053, #5300, #12994, #15478, #18010, #20842, #30564, #8309, #28364, #28698, #25373, #7652, #23204 ),
 .UNSPECIFIED., .F., .F.,
 ( 4, 3, 3, 3, 3, 3, 3, 4 ),
 ( 1.041059936534947552E-17, 0.0001461945829181783975, 0.0002459472205448162371, 0.0003138760397545359141, 0.0003818610883897723303, 0.0004082995574110840752, 0.0004281800295585239330, 0.0004357603615204788520 ),
 .UNSPECIFIED. ) ;
#6550 = APPROVAL ( #9110, 'UNSPECIFIED' ) ;
#6551 = CARTESIAN_POINT ( 'NONE',  ( -53.64896896705157303, 5.489213761225001598, 1.476102572572478344 ) ) ;
#6552 = ORIENTED_EDGE ( 'NONE', *, *, #5248, .F. ) ;
#6553 = CARTESIAN_POINT ( 'NONE',  ( 7.249760686538667009, 0.000000000000000000, 0.000000000000000000 ) ) ;
#6555 = ORIENTED_EDGE ( 'NONE', *, *, #24372, .F. ) ;
#6554 = CARTESIAN_POINT ( 'NONE',  ( 54.94556186992998192, -5.362550666240347041, -3.998506278715515005 ) ) ;
#6556 = ORIENTED_EDGE ( 'NONE', *, *, #12216, .F. ) ;
#6557 = CARTESIAN_POINT ( 'NONE',  ( 7.249760686538667009, 6.147671362329302447, -6.226446564517854831 ) ) ;
#6558 = CARTESIAN_POINT ( 'NONE',  ( 0.000000000000000000, 7.958834565716875531, -7.593217523260492818 ) ) ;
#6560 = ORIENTED_EDGE ( 'NONE', *, *, #24542, .T. ) ;
#6559 = CARTESIAN_POINT ( 'NONE',  ( 0.7632845268398871230, 0.000000000000000000, 0.000000000000000000 ) ) ;
#6561 = AXIS2_PLACEMENT_3D ( 'NONE', #16486, #6300, #16987 ) ;
#6562 = CARTESIAN_POINT ( 'NONE',  ( 13.32584843805069852, 6.791410140808786799, -1.050000000000000044 ) ) ;
#6563 = LINE ( 'NONE', #1547, #17586 ) ;
#6564 = AXIS2_PLACEMENT_3D ( 'NONE', #13716, #11550, #1027 ) ;
#6565 = LINE ( 'NONE', #26964, #9684 ) ;
#6566 = AXIS2_PLACEMENT_3D ( 'NONE', #24024, #13675, #3823 ) ;
#6567 = CARTESIAN_POINT ( 'NONE',  ( 9.126991456844553596, -11.32614230912571429, -1.000000000000000000 ) ) ;
#6569 = EDGE_LOOP ( 'NONE', ( #30161, #24456, #11194, #7851 ) ) ;
#6568 = CARTESIAN_POINT ( 'NONE',  ( 108.0265109756391553, -18.45111357072248737, -4.417761971609380112 ) ) ;
#6570 = DIRECTION ( 'NONE',  ( -1.000000000000000000, 8.574039729943017111E-17, -3.081487911019577365E-33 ) ) ;
#6571 = EDGE_CURVE ( 'NONE', #25432, #14457, #1863, .T. ) ;
#6572 = VECTOR ( 'NONE', #10905, 1000.000000000000000 ) ;
#6573 = VECTOR ( 'NONE', #28093, 1000.000000000000114 ) ;
#6574 = CARTESIAN_POINT ( 'NONE',  ( 24.99290772595112031, -0.1310194482076040834, -2.499999999999998668 ) ) ;
#6575 = CARTESIAN_POINT ( 'NONE',  ( 102.4237878418650638, -3.999739124950154157, 3.993434327388001748 ) ) ;
#6576 = PLANE ( 'NONE',  #10754 ) ;
#6577 = CARTESIAN_POINT ( 'NONE',  ( -50.60000000000000142, 0.000000000000000000, 1.000000000000000000 ) ) ;
#6578 = ORIENTED_EDGE ( 'NONE', *, *, #26574, .T. ) ;
#6579 = CARTESIAN_POINT ( 'NONE',  ( -6.300050800000000173, -2.983565686104819648, -0.3135853898029605791 ) ) ;
#6580 = CARTESIAN_POINT ( 'NONE',  ( 107.9275968081481238, 17.77499038371485440, 4.627610784060873783 ) ) ;
#6581 = CARTESIAN_POINT ( 'NONE',  ( 2.795120667416423732, -6.320583870820068562, -7.433119754668543244 ) ) ;
#6582 = ORIENTED_EDGE ( 'NONE', *, *, #26791, .T. ) ;
#6583 = AXIS2_PLACEMENT_3D ( 'NONE', #6918, #33015, #2258 ) ;
#6584 =( BOUNDED_CURVE ( )  B_SPLINE_CURVE ( 2, ( #21483, #19128, #31698, #13442, #8776, #10963, #18981, #3756, #29319, #13922, #3940, #18487, #21165, #595, #24141, #10786, #21001, #31216, #8293, #28680, #15952, #26171, #3277, #31363, #14612, #24313, #4433, #9261, #9759, #24625, #6598, #9076, #12105, #29675, #30001, #14261, #4594, #6906, #22463, #1574, #24457, #11601, #6754, #14769, #9573, #19633, #7259, #27646, #21797, #16795, #32360, #22302, #19483, #1932, #32512, #29831, #12252, #16945, #1755, #32680, #19300, #17103, #27141, #24813, #1424, #19793, #4242, #19984, #11952, #26992, #29501, #7092, #14414, #17297, #11761, #24967, #27313, #30185, #21964, #32189, #22149 ),
 .UNSPECIFIED., .F., .F. ) 
 B_SPLINE_CURVE_WITH_KNOTS ( ( 3, 2, 2, 2, 2, 2, 2, 2, 2, 2, 2, 2, 2, 2, 2, 2, 2, 2, 2, 2, 2, 2, 2, 2, 2, 2, 2, 2, 2, 2, 2, 2, 2, 2, 2, 2, 2, 2, 2, 2, 3 ),
 ( 0.007661791872508488463, 0.02500000000000000139, 0.05000000000000000278, 0.07499999999999999722, 0.1000000000000000056, 0.1250000000000000000, 0.1499999999999999944, 0.1749999999999999889, 0.2000000000000000111, 0.2250000000000000056, 0.2500000000000000000, 0.2750000000000000222, 0.2999999999999999889, 0.3250000000000000111, 0.3499999999999999778, 0.3750000000000000000, 0.4000000000000000222, 0.4249999999999999889, 0.4500000000000000111, 0.4749999999999999778, 0.5000000000000000000, 0.5250000000000000222, 0.5500000000000000444, 0.5749999999999999556, 0.5999999999999999778, 0.6250000000000000000, 0.6500000000000000222, 0.6750000000000000444, 0.6999999999999999556, 0.7249999999999999778, 0.7500000000000000000, 0.7750000000000000222, 0.8000000000000000444, 0.8249999999999999556, 0.8499999999999999778, 0.8750000000000000000, 0.9000000000000000222, 0.9249999999999999334, 0.9499999999999999556, 0.9749999999999999778, 1.000000000000000000 ),
 .UNSPECIFIED. ) 
 CURVE ( )  GEOMETRIC_REPRESENTATION_ITEM ( )  RATIONAL_B_SPLINE_CURVE ( ( 0.9676416783621932804, 0.9472082996767494656, 1.000000000000000000, 0.9238795325112867385, 1.000000000000000000, 0.9238795325112867385, 1.000000000000000000, 0.9238795325112867385, 1.000000000000000000, 0.9238795325112867385, 1.000000000000000000, 0.9238795325112867385, 1.000000000000000000, 0.9238795325112867385, 1.000000000000000000, 0.9238795325112867385, 1.000000000000000000, 0.9238795325112867385, 1.000000000000000000, 0.9238795325112867385, 1.000000000000000000, 0.9238795325112867385, 1.000000000000000000, 0.9238795325112867385, 1.000000000000000000, 0.9238795325112867385, 1.000000000000000000, 0.9238795325112867385, 1.000000000000000000, 0.9238795325112867385, 1.000000000000000000, 0.9238795325112867385, 1.000000000000000000, 0.9238795325112867385, 1.000000000000000000, 0.9238795325112867385, 1.000000000000000000, 0.9238795325112867385, 1.000000000000000000, 0.9238795325112867385, 1.000000000000000000, 0.9238795325112867385, 1.000000000000000000, 0.9238795325112867385, 1.000000000000000000, 0.9238795325112867385, 1.000000000000000000, 0.9238795325112867385, 1.000000000000000000, 0.9238795325112867385, 1.000000000000000000, 0.9238795325112867385, 1.000000000000000000, 0.9238795325112867385, 1.000000000000000000, 0.9238795325112867385, 1.000000000000000000, 0.9238795325112867385, 1.000000000000000000, 0.9238795325112867385, 1.000000000000000000, 0.9238795325112867385, 1.000000000000000000, 0.9238795325112867385, 1.000000000000000000, 0.9238795325112867385, 1.000000000000000000, 0.9238795325112867385, 1.000000000000000000, 0.9238795325112867385, 1.000000000000000000, 0.9238795325112867385, 1.000000000000000000, 0.9238795325112867385, 1.000000000000000000, 0.9238795325112867385, 1.000000000000000000, 0.9238795325112867385, 1.000000000000000000, 0.9238795325112867385, 1.000000000000000000 ) ) 
 REPRESENTATION_ITEM ( '' )  );
#6585 = CARTESIAN_POINT ( 'NONE',  ( -35.00000000000000000, 0.5000000000000000000, -2.482234843104710986 ) ) ;
#6586 = CARTESIAN_POINT ( 'NONE',  ( 20.55463713078601629, -21.58103817311699402, 1.582345582279547358 ) ) ;
#6588 = ORIENTED_EDGE ( 'NONE', *, *, #4956, .T. ) ;
#6587 = CIRCLE ( 'NONE', #10342, 11.00000000000000000 ) ;
#6589 = CARTESIAN_POINT ( 'NONE',  ( 2.382865613620175349, 0.5000000000000000000, -1.500000000000000000 ) ) ;
#6590 = ORIENTED_EDGE ( 'NONE', *, *, #9460, .F. ) ;
#6591 = AXIS2_PLACEMENT_3D ( 'NONE', #19240, #29439, #17040 ) ;
#6592 = AXIS2_PLACEMENT_3D ( 'NONE', #488, #10673, #16004 ) ;
#6593 = ORIENTED_EDGE ( 'NONE', *, *, #15276, .T. ) ;
#6594 = CARTESIAN_POINT ( 'NONE',  ( 5.489321606599602887, 2.874206582856514203, -7.593050043411082584 ) ) ;
#6596 = ORIENTED_EDGE ( 'NONE', *, *, #2532, .T. ) ;
#6595 = CARTESIAN_POINT ( 'NONE',  ( 21.36097421961356702, -21.76718868951428121, -1.410897148389125277 ) ) ;
#6597 = ORIENTED_EDGE ( 'NONE', *, *, #28548, .F. ) ;
#6598 = CARTESIAN_POINT ( 'NONE',  ( 23.92250000136559507, -1.913930629741527500, 2.363507492473149618 ) ) ;
#6599 = APPROVAL_PERSON_ORGANIZATION ( #13963, #29231, #16649 ) ;
#6600 = ORIENTED_EDGE ( 'NONE', *, *, #29229, .T. ) ;
#6601 = CARTESIAN_POINT ( 'NONE',  ( 16.36487458112951643, 19.37645981759113312, 4.629213727441584325 ) ) ;
#6602 = DIRECTION ( 'NONE',  ( 0.000000000000000000, 0.000000000000000000, 1.000000000000000000 ) ) ;
#6604 = VERTEX_POINT ( 'NONE', #1672 ) ;
#6603 = CARTESIAN_POINT ( 'NONE',  ( 47.88941090695973912, -4.233884984401246498, -1.873788949266955273 ) ) ;
#6605 = CARTESIAN_POINT ( 'NONE',  ( 21.64920974929931674, -21.84574742533145297, 1.293063406869986443 ) ) ;
#6606 = CARTESIAN_POINT ( 'NONE',  ( 2.274274201625327230, 0.000000000000000000, 0.000000000000000000 ) ) ;
#6607 = CARTESIAN_POINT ( 'NONE',  ( 101.8797206818347973, -5.166491396334524033, 2.184956718991889257 ) ) ;
#6608 = FACE_OUTER_BOUND ( 'NONE', #16797, .T. ) ;
#6609 = EDGE_CURVE ( 'NONE', #4684, #11449, #31012, .T. ) ;
#6610 = AXIS2_PLACEMENT_3D ( 'NONE', #7384, #1908, #19608 ) ;
#6611 = ADVANCED_FACE ( 'NONE', ( #6688 ), #19563, .F. ) ;
#6612 = DIRECTION ( 'NONE',  ( -1.000000000000000000, 0.000000000000000000, 0.000000000000000000 ) ) ;
#6613 = CYLINDRICAL_SURFACE ( 'NONE', #12357, 2.999999999999999112 ) ;
#6614 = CARTESIAN_POINT ( 'NONE',  ( 10.00000000000000000, -4.208382051008212166, 2.718385644597159256 ) ) ;
#6615 = B_SPLINE_CURVE_WITH_KNOTS ( 'NONE', 3,
 ( #20464, #17945, #20940, #25968 ),
 .UNSPECIFIED., .F., .F.,
 ( 4, 4 ),
 ( 2.049880227751699666E-07, 0.0008064882591616613769 ),
 .UNSPECIFIED. ) ;
#6616 = CARTESIAN_POINT ( 'NONE',  ( 7.249760686538667009, 6.940565734314653845, -4.007137495034738706 ) ) ;
#6617 = CARTESIAN_POINT ( 'NONE',  ( -5.390905497009061520, 2.994789822248785871, -3.164707540391768603 ) ) ;
#6618 = CARTESIAN_POINT ( 'NONE',  ( 9.999999999999998224, -4.681538312723522388, 0.8254815157535101422 ) ) ;
#6619 = APPROVAL_PERSON_ORGANIZATION ( #5501, #7982, #21197 ) ;
#6620 = CYLINDRICAL_SURFACE ( 'NONE', #20904, 4.999999999999997335 ) ;
#6621 = CARTESIAN_POINT ( 'NONE',  ( -6.300050802731188782, -2.853674364686378695, -1.549418761218566809 ) ) ;
#6622 = VERTEX_POINT ( 'NONE', #31940 ) ;
#6623 = CARTESIAN_POINT ( 'NONE',  ( -7.500050800000000351, 2.983565686104819648, 0.3135853898029609677 ) ) ;
#6624 = DIRECTION ( 'NONE',  ( 0.000000000000000000, -0.4226182617407104325, 0.9063077870366448296 ) ) ;
#6625 = CARTESIAN_POINT ( 'NONE',  ( 56.97280603064898941, -277.2763395528616002, 0.4463807625372899768 ) ) ;
#6626 = CARTESIAN_POINT ( 'NONE',  ( 8.706508904963646600, -1.271749511502713093, 1.500000000000000222 ) ) ;
#6627 = ORIENTED_EDGE ( 'NONE', *, *, #28906, .F. ) ;
#6628 = CARTESIAN_POINT ( 'NONE',  ( 9.836026323042709407, -12.51705112700696176, -1.500000000000000444 ) ) ;
#6629 = VECTOR ( 'NONE', #27505, 1000.000000000000000 ) ;
#6630 = VERTEX_POINT ( 'NONE', #32444 ) ;
#6631 = CARTESIAN_POINT ( 'NONE',  ( 0.1360978363991151296, -7.042592391184042455, 1.774497828403761579 ) ) ;
#6632 = DATE_AND_TIME ( #22181, #13556 ) ;
#6633 = DIRECTION ( 'NONE',  ( 0.1027947991993878873, -0.9947025833170223263, 0.000000000000000000 ) ) ;
#6634 = ORIENTED_EDGE ( 'NONE', *, *, #20016, .T. ) ;
#6635 = CARTESIAN_POINT ( 'NONE',  ( 8.862909208978498654, -0.2945138977690187065, -1.470869863057391980 ) ) ;
#6636 = DIRECTION ( 'NONE',  ( 0.000000000000000000, 0.000000000000000000, -1.000000000000000000 ) ) ;
#6637 = CARTESIAN_POINT ( 'NONE',  ( 8.911384905465308037, 0.2172754300403238470, -1.412391582772828169 ) ) ;
#6638 = CARTESIAN_POINT ( 'NONE',  ( 22.19921710918831081, -17.00655848932595049, -1.494769569001199727 ) ) ;
#6639 = CARTESIAN_POINT ( 'NONE',  ( 11.04311965146451158, 15.00000000000000178, -1.491740999229418829 ) ) ;
#6640 = ORIENTED_EDGE ( 'NONE', *, *, #8126, .F. ) ;
#6641 = EDGE_CURVE ( 'NONE', #12104, #27444, #26208, .T. ) ;
#6642 = CARTESIAN_POINT ( 'NONE',  ( 40.87146290594699849, -4.622005974785199811, 2.184956282062899380 ) ) ;
#6643 = ADVANCED_FACE ( 'NONE', ( #27421 ), #22076, .F. ) ;
#6644 = CARTESIAN_POINT ( 'NONE',  ( 8.870145747188287189, 0.000000000000000000, 1.000000000000000000 ) ) ;
#6645 = DIRECTION ( 'NONE',  ( -0.04852105321274703675, 0.4695180821586693587, -0.8815886103626627834 ) ) ;
#6646 = CARTESIAN_POINT ( 'NONE',  ( 34.98193025661426248, 0.5174497483512505713, -2.999999999999995559 ) ) ;
#6647 = ADVANCED_FACE ( 'NONE', ( #16716 ), #8039, .T. ) ;
#6649 = VERTEX_POINT ( 'NONE', #32293 ) ;
#6648 = DIRECTION ( 'NONE',  ( 0.000000000000000000, -0.8191520442889975717, 0.5735764363510378328 ) ) ;
#6650 = CARTESIAN_POINT ( 'NONE',  ( 108.1722781158648417, 19.13747245171689570, -4.846044801720160500 ) ) ;
#6651 = DIRECTION ( 'NONE',  ( 1.000000000000000000, 0.000000000000000000, 0.000000000000000000 ) ) ;
#6652 = CARTESIAN_POINT ( 'NONE',  ( -4.400050802731187538, 3.113457007523260156, -0.9222479816126439855 ) ) ;
#6653 = PLANE ( 'NONE',  #8065 ) ;
#6654 = FACE_OUTER_BOUND ( 'NONE', #3207, .T. ) ;
#6655 = LINE ( 'NONE', #28887, #23077 ) ;
#6656 = SHAPE_REPRESENTATION ( 'Part8_handle2Sleeve', ( #2865 ), #30610 ) ;
#6657 = AXIS2_PLACEMENT_3D ( 'NONE', #18859, #29062, #6296 ) ;
#6658 = CARTESIAN_POINT ( 'NONE',  ( -31.57659242536668032, 0.000000000000000000, -1.500000000000000000 ) ) ;
#6659 = FACE_OUTER_BOUND ( 'NONE', #30374, .T. ) ;
#6660 = CYLINDRICAL_SURFACE ( 'NONE', #20938, 5.010000000000000675 ) ;
#6661 = EDGE_LOOP ( 'NONE', ( #19006, #2074, #26066 ) ) ;
#6662 = FACE_OUTER_BOUND ( 'NONE', #3501, .T. ) ;
#6663 = ORIENTED_EDGE ( 'NONE', *, *, #12875, .F. ) ;
#6664 = CARTESIAN_POINT ( 'NONE',  ( -53.95513674679793326, 5.522463357794191730, 1.050000000000049116 ) ) ;
#6665 = CARTESIAN_POINT ( 'NONE',  ( 108.9099939950573912, 17.58789101224671469, 5.127064438068912544 ) ) ;
#6666 = CARTESIAN_POINT ( 'NONE',  ( 23.80135741154355244, -5.059951201419124800, -5.695980980372493008 ) ) ;
#6667 = CARTESIAN_POINT ( 'NONE',  ( 109.4476176138146002, 20.58159145763585940, -1.739510325230362309 ) ) ;
#6668 = DIRECTION ( 'NONE',  ( -1.000000000000000000, 0.000000000000000000, 0.000000000000000000 ) ) ;
#6669 = ORIENTED_EDGE ( 'NONE', *, *, #7184, .T. ) ;
#6670 = CARTESIAN_POINT ( 'NONE',  ( 25.75999999999999801, -2.208672634433321348E-15, 0.000000000000000000 ) ) ;
#6671 = ORIENTED_EDGE ( 'NONE', *, *, #8308, .F. ) ;
#6672 = DATE_TIME_ROLE ( 'creation_date' ) ;
#6673 = B_SPLINE_CURVE_WITH_KNOTS ( 'NONE', 3,
 ( #20452, #10408, #7555, #23118, #20271, #237, #20618, #18251, #30824, #15757 ),
 .UNSPECIFIED., .F., .F.,
 ( 4, 2, 2, 2, 4 ),
 ( 3.512955445812634541E-07, 0.0005479535487286800108, 0.001095555801912778812, 0.001643158055096877613, 0.002190760308280976631 ),
 .UNSPECIFIED. ) ;
#6674 = DIRECTION ( 'NONE',  ( 0.000000000000000000, 0.08715574274767322327, -0.9961946980917442129 ) ) ;
#6675 = ADVANCED_FACE ( 'NONE', ( #2012 ), #3859, .F. ) ;
#6676 = CARTESIAN_POINT ( 'NONE',  ( -3.750050802731187627, 0.3135853898029611342, -2.983565686104819648 ) ) ;
#6677 = CARTESIAN_POINT ( 'NONE',  ( 5.377543748152550762, 6.139290821770327256, -5.151476664237414127 ) ) ;
#6678 = VERTEX_POINT ( 'NONE', #9353 ) ;
#6679 = ORIENTED_EDGE ( 'NONE', *, *, #19361, .F. ) ;
#6680 = ADVANCED_FACE ( 'NONE', ( #9179 ), #24393, .T. ) ;
#6681 = DIRECTION ( 'NONE',  ( -8.281886410780517190E-17, -0.9659258262890689783, 0.2588190451025184080 ) ) ;
#6682 = CARTESIAN_POINT ( 'NONE',  ( 0.000000000000000000, 0.5000000000000000000, 1.500000000000000000 ) ) ;
#6683 = CARTESIAN_POINT ( 'NONE',  ( 23.79750000000001009, 0.7685399846772009713, -2.594547506269381909 ) ) ;
#6684 = CARTESIAN_POINT ( 'NONE',  ( 0.8808402398300805292, -9.175602370491700910, -1.499999999999930056 ) ) ;
#6686 = VERTEX_POINT ( 'NONE', #4346 ) ;
#6685 = LINE ( 'NONE', #16874, #13860 ) ;
#6687 = CARTESIAN_POINT ( 'NONE',  ( -4.987550801365594033, 0.3701630799359330593, -3.521866450007987037 ) ) ;
#6688 = FACE_OUTER_BOUND ( 'NONE', #19983, .T. ) ;
#6689 = EDGE_CURVE ( 'NONE', #3357, #29995, #20860, .T. ) ;
#6690 = FACE_OUTER_BOUND ( 'NONE', #8286, .T. ) ;
#6691 = CARTESIAN_POINT ( 'NONE',  ( -14.62340757463330654, -21.93932300455828255, -1.292893218813452538 ) ) ;
#6692 = ORIENTED_EDGE ( 'NONE', *, *, #1830, .F. ) ;
#6694 = ORIENTED_EDGE ( 'NONE', *, *, #25321, .F. ) ;
#6693 = CARTESIAN_POINT ( 'NONE',  ( 12.62463379335046376, 21.58553169041389452, 1.499999999999994449 ) ) ;
#6695 = CARTESIAN_POINT ( 'NONE',  ( 22.89575061816920254, 17.95407957496613705, 1.500000000000000222 ) ) ;
#6696 = FACE_OUTER_BOUND ( 'NONE', #19299, .T. ) ;
#6697 = EDGE_CURVE ( 'NONE', #136, #21332, #17115, .T. ) ;
#6698 = CARTESIAN_POINT ( 'NONE',  ( -23.54713438637984169, 18.46223496596754288, 1.773004750130224627 ) ) ;
#6699 = CARTESIAN_POINT ( 'NONE',  ( 3.744708216408842549, 0.000000000000000000, -1.000000000000000000 ) ) ;
#6700 = FACE_OUTER_BOUND ( 'NONE', #14369, .T. ) ;
#6701 = CARTESIAN_POINT ( 'NONE',  ( 2.274274201625327230, -1.975651141462315907, 10.82112760146735475 ) ) ;
#6702 = CARTESIAN_POINT ( 'NONE',  ( 19.00106589343894825, -3.165308183742224557, 1.169950778989204521 ) ) ;
#6703 = CARTESIAN_POINT ( 'NONE',  ( -3.437550801365593767, -1.088641768524163389, -3.675193018007246071 ) ) ;
#6704 = ORIENTED_EDGE ( 'NONE', *, *, #5130, .T. ) ;
#6705 = DIRECTION ( 'NONE',  ( 0.000000000000000000, 0.000000000000000000, 1.000000000000000000 ) ) ;
#6706 = ORIENTED_EDGE ( 'NONE', *, *, #30019, .T. ) ;
#6707 = CARTESIAN_POINT ( 'NONE',  ( 21.24324854073028490, -21.72960979489713651, 1.457811124649513346 ) ) ;
#6708 = EDGE_CURVE ( 'NONE', #32554, #28100, #7487, .T. ) ;
#6709 = DIRECTION ( 'NONE',  ( 0.000000000000000000, 1.000000000000000000, -1.224646799147353207E-16 ) ) ;
#6711 = FACE_OUTER_BOUND ( 'NONE', #4044, .T. ) ;
#6710 = DIRECTION ( 'NONE',  ( 0.000000000000000000, -0.9659258262890652036, -0.2588190451025326189 ) ) ;
#6712 = ORIENTED_EDGE ( 'NONE', *, *, #21718, .T. ) ;
#6713 = DIRECTION ( 'NONE',  ( 0.000000000000000000, 0.000000000000000000, 1.000000000000000000 ) ) ;
#6714 = ORIENTED_EDGE ( 'NONE', *, *, #13166, .F. ) ;
#6715 = CARTESIAN_POINT ( 'NONE',  ( 2.857987933995207896, -9.536462466387789050, 0.6743480930025419484 ) ) ;
#6717 = ORIENTED_EDGE ( 'NONE', *, *, #29954, .T. ) ;
#6716 = CARTESIAN_POINT ( 'NONE',  ( 102.3441463922209920, -2.857283636501866564, -3.997238528716361650 ) ) ;
#6718 = VERTEX_POINT ( 'NONE', #7497 ) ;
#6719 = ADVANCED_FACE ( 'NONE', ( #22569 ), #25236, .T. ) ;
#6720 = ADVANCED_FACE ( 'NONE', ( #7341 ), #2666, .T. ) ;
#6721 = CARTESIAN_POINT ( 'NONE',  ( 5.489321708267612898, 5.297846913781776301, -6.152096559282782984 ) ) ;
#6722 = DIRECTION ( 'NONE',  ( 0.4999999999999960587, -0.09052430460833682524, -0.8612812260087764349 ) ) ;
#6724 = ORIENTED_EDGE ( 'NONE', *, *, #11439, .F. ) ;
#6723 = CARTESIAN_POINT ( 'NONE',  ( -4.526546459660798938, -7.591509378209715386, -1.500000000000000888 ) ) ;
#6725 = CARTESIAN_POINT ( 'NONE',  ( 25.55085174366697487, 19.30847049843654162, -1.500000000000000000 ) ) ;
#6726 = DIRECTION ( 'NONE',  ( 0.000000000000000000, 0.8191520442889907994, 0.5735764363510474917 ) ) ;
#6727 = DIRECTION ( 'NONE',  ( -1.000000000000000000, 8.574039729943018344E-17, -0.000000000000000000 ) ) ;
#6728 = CARTESIAN_POINT ( 'NONE',  ( 7.168700580349904428, -6.410142746794999624, -1.000000000000000000 ) ) ;
#6729 = ADVANCED_FACE ( 'NONE', ( #5336 ), #32783, .F. ) ;
#6731 = VERTEX_POINT ( 'NONE', #17888 ) ;
#6730 = CARTESIAN_POINT ( 'NONE',  ( 107.4616889483734212, -17.52894894125598313, -4.827028120670242117 ) ) ;
#6732 = CARTESIAN_POINT ( 'NONE',  ( 0.000000000000000000, 8.572527594031471218E-16, 6.999999999999998224 ) ) ;
#6733 = CARTESIAN_POINT ( 'NONE',  ( 0.000000000000000000, -10.90201369670497478, -1.464956435139655566 ) ) ;
#6734 = CARTESIAN_POINT ( 'NONE',  ( 21.36097421961356702, -21.76718868951428121, -1.410897148389125277 ) ) ;
#6735 = EDGE_CURVE ( 'NONE', #10930, #28345, #33028, .T. ) ;
#6736 = CARTESIAN_POINT ( 'NONE',  ( 24.65887284179023453, -17.47660047452463772, -1.497285395512024442 ) ) ;
#6737 = CARTESIAN_POINT ( 'NONE',  ( -0.9232102171129843438, 0.000000000000000000, 4.522129901861158707 ) ) ;
#6738 = ORIENTED_EDGE ( 'NONE', *, *, #5279, .F. ) ;
#6739 = DIRECTION ( 'NONE',  ( 0.000000000000000000, 0.000000000000000000, -1.000000000000000000 ) ) ;
#6740 = DIRECTION ( 'NONE',  ( 0.000000000000000000, 0.000000000000000000, 1.000000000000000000 ) ) ;
#6741 = CARTESIAN_POINT ( 'NONE',  ( 2.970200582152834112, -5.831559621424813322, -7.065646041987135639 ) ) ;
#6742 = ORIENTED_EDGE ( 'NONE', *, *, #23281, .F. ) ;
#6743 = DIRECTION ( 'NONE',  ( 0.000000000000000000, 0.000000000000000000, 1.000000000000000000 ) ) ;
#6744 = CARTESIAN_POINT ( 'NONE',  ( 2.535833972131074976, -0.1672301947041132664, -1.432210082195892520 ) ) ;
#6745 = ORIENTED_EDGE ( 'NONE', *, *, #26662, .T. ) ;
#6746 = CARTESIAN_POINT ( 'NONE',  ( 1.449793745490414176, -2.781154674314748831, -1.500000000000000222 ) ) ;
#6747 = EDGE_CURVE ( 'NONE', #545, #2577, #24581, .T. ) ;
#6748 = ORIENTED_EDGE ( 'NONE', *, *, #12942, .F. ) ;
#6749 = VERTEX_POINT ( 'NONE', #15204 ) ;
#6750 = DIRECTION ( 'NONE',  ( -1.000000000000000000, 0.000000000000000000, 0.000000000000000000 ) ) ;
#6752 = ORIENTED_EDGE ( 'NONE', *, *, #16232, .T. ) ;
#6751 = CARTESIAN_POINT ( 'NONE',  ( 2.274274201625327230, -5.222868219166924675, 9.680994141368751471 ) ) ;
#6753 = ORIENTED_EDGE ( 'NONE', *, *, #30829, .T. ) ;
#6754 = CARTESIAN_POINT ( 'NONE',  ( 23.17250000136559862, -2.363507492473152283, -1.913930629741525280 ) ) ;
#6755 = EDGE_CURVE ( 'NONE', #17637, #31361, #175, .T. ) ;
#6756 = ORIENTED_EDGE ( 'NONE', *, *, #6689, .T. ) ;
#6757 = DIRECTION ( 'NONE',  ( 0.000000000000000000, 0.000000000000000000, 1.000000000000000000 ) ) ;
#6758 = DIRECTION ( 'NONE',  ( 1.000000000000000000, -8.574039729943018344E-17, -0.000000000000000000 ) ) ;
#6760 = ORIENTED_EDGE ( 'NONE', *, *, #31170, .F. ) ;
#6759 = CARTESIAN_POINT ( 'NONE',  ( 29.32642088969984329, -4.109531239335385777, -1.873788766282285856 ) ) ;
#6761 = CARTESIAN_POINT ( 'NONE',  ( 6.357667873252802693, -8.266402141659458636, 2.398098878660925859 ) ) ;
#6762 = LINE ( 'NONE', #1582, #15438 ) ;
#6763 = CARTESIAN_POINT ( 'NONE',  ( 101.8470492078815255, -4.696030299047205148, 2.942092770106637722 ) ) ;
#6764 = CARTESIAN_POINT ( 'NONE',  ( 24.79750000136559507, 0.3178988483021036315, 3.024605502323848949 ) ) ;
#6765 = CARTESIAN_POINT ( 'NONE',  ( 2.857987972553724720, 5.059832898189586814, -8.111531947331014791 ) ) ;
#6766 = PERSON ( 'UNSPECIFIED', 'UNSPECIFIED', 'UNSPECIFIED', ('UNSPECIFIED'), ('UNSPECIFIED'), ('UNSPECIFIED') ) ;
#6767 = CARTESIAN_POINT ( 'NONE',  ( -1.023266466338763614, -9.291661594692715909, -5.485967528433937979 ) ) ;
#6768 = CARTESIAN_POINT ( 'NONE',  ( 29.18511942701329787, -8.255514837367675440, -0.8105614686289663862 ) ) ;
#6769 = CARTESIAN_POINT ( 'NONE',  ( 7.249760686538667009, 4.007137495034909236, -6.940565734314555257 ) ) ;
#6770 = ADVANCED_FACE ( 'NONE', ( #15355 ), #7689, .F. ) ;
#6771 = DIRECTION ( 'NONE',  ( -0.005016709653754841333, -0.9993908270190956511, 0.03453704524619621158 ) ) ;
#6772 = DIRECTION ( 'NONE',  ( 1.000000000000000000, 0.000000000000000000, 0.000000000000000000 ) ) ;
#6773 = FACE_OUTER_BOUND ( 'NONE', #24834, .T. ) ;
#6774 =( BOUNDED_CURVE ( )  B_SPLINE_CURVE ( 2, ( #26355, #12974, #13135 ),
 .UNSPECIFIED., .F., .F. ) 
 B_SPLINE_CURVE_WITH_KNOTS ( ( 3, 3 ),
 ( 0.9966116191895003640, 1.000000000000000000 ),
 .UNSPECIFIED. ) 
 CURVE ( )  GEOMETRIC_REPRESENTATION_ITEM ( )  RATIONAL_B_SPLINE_CURVE ( ( 0.9821626249036858880, 0.9896829947469992783, 1.000000000000000000 ) ) 
 REPRESENTATION_ITEM ( '' )  );
#6775 = DIRECTION ( 'NONE',  ( -0.000000000000000000, -1.000000000000000000, -0.000000000000000000 ) ) ;
#6776 = CARTESIAN_POINT ( 'NONE',  ( -4.950050802731188249, -0.3135853898029607456, 2.983565686104819648 ) ) ;
#6777 = ORIENTED_EDGE ( 'NONE', *, *, #11575, .F. ) ;
#6778 = CARTESIAN_POINT ( 'NONE',  ( -7.437550801365595099, -1.088641768524163389, -3.675193018007246071 ) ) ;
#6779 = CARTESIAN_POINT ( 'NONE',  ( 108.0068349480237515, 18.21621961241920573, -4.398253369385427547 ) ) ;
#6780 = FACE_OUTER_BOUND ( 'NONE', #12585, .T. ) ;
#6781 = LINE ( 'NONE', #22175, #19977 ) ;
#6782 = ORIENTED_EDGE ( 'NONE', *, *, #23043, .F. ) ;
#6783 = CARTESIAN_POINT ( 'NONE',  ( -2.162942409646512854, 4.884725290497410777E-15, -2.999999999999999556 ) ) ;
#6784 = DIRECTION ( 'NONE',  ( 0.4999999999999981681, 0.8660254037844395958, 0.000000000000000000 ) ) ;
#6785 = EDGE_CURVE ( 'NONE', #773, #5629, #27265, .T. ) ;
#6786 = ORIENTED_EDGE ( 'NONE', *, *, #12471, .F. ) ;
#6787 = CARTESIAN_POINT ( 'NONE',  ( 12.23122861076465817, -15.17374145964417842, 1.499999999999998668 ) ) ;
#6788 = EDGE_CURVE ( 'NONE', #21638, #14302, #28348, .T. ) ;
#6789 = CALENDAR_DATE ( 2026, 6, 10 ) ;
#6790 = DIRECTION ( 'NONE',  ( 0.000000000000000000, 0.000000000000000000, 1.000000000000000000 ) ) ;
#6791 = EDGE_LOOP ( 'NONE', ( #8027, #26067, #5099, #27609 ) ) ;
#6792 = CARTESIAN_POINT ( 'NONE',  ( 9.350000000000004974, 2.117582368135760237E-19, -1.049909311857671668 ) ) ;
#6793 = CARTESIAN_POINT ( 'NONE',  ( 21.39732310845265673, 16.45281003597622416, -1.050000000000000044 ) ) ;
#6794 = CARTESIAN_POINT ( 'NONE',  ( 102.4145990881584254, -3.874303363244021359, -4.155404932454223932 ) ) ;
#6795 = FACE_OUTER_BOUND ( 'NONE', #15768, .T. ) ;
#6796 = CARTESIAN_POINT ( 'NONE',  ( 4.749760686538667009, -7.530955069117495349, -2.741043480755002371 ) ) ;
#6797 = ORIENTED_EDGE ( 'NONE', *, *, #90, .T. ) ;
#6798 = CARTESIAN_POINT ( 'NONE',  ( 8.930755659325139817, 0.4999999999999980571, -1.500000000000000000 ) ) ;
#6799 = CARTESIAN_POINT ( 'NONE',  ( 23.19643008672645124, -21.93767770566458353, -1.043375197815119115 ) ) ;
#6800 = DIRECTION ( 'NONE',  ( 0.000000000000000000, -0.4067366430757887175, -0.9135454576426059736 ) ) ;
#6802 = ORIENTED_EDGE ( 'NONE', *, *, #23782, .T. ) ;
#6801 = DIRECTION ( 'NONE',  ( -1.000000000000000000, -0.000000000000000000, -0.000000000000000000 ) ) ;
#6803 = CARTESIAN_POINT ( 'NONE',  ( 2.652619124157556740, 0.000000000000000000, -1.000000000000000000 ) ) ;
#6804 = FACE_OUTER_BOUND ( 'NONE', #1722, .T. ) ;
#6805 = CARTESIAN_POINT ( 'NONE',  ( -4.550050802731187005, 0.3135853898029611342, -2.983565686104819648 ) ) ;
#6806 = CARTESIAN_POINT ( 'NONE',  ( 25.89197189428493218, 19.03682222646506261, 1.281348668662838586 ) ) ;
#6807 = CARTESIAN_POINT ( 'NONE',  ( 0.7632845268448539278, 8.734705317657757817, 0.4999240074866477257 ) ) ;
#6808 = DIRECTION ( 'NONE',  ( -1.000000000000000000, 0.000000000000000000, 0.000000000000000000 ) ) ;
#6809 = CARTESIAN_POINT ( 'NONE',  ( -1.773875666770781789, -0.3178988483021056854, 3.024605502323848949 ) ) ;
#6810 = CARTESIAN_POINT ( 'NONE',  ( 0.000000000000000000, 0.000000000000000000, 4.137834579201376428 ) ) ;
#6811 = DIRECTION ( 'NONE',  ( 1.000000000000000000, -0.000000000000000000, -0.000000000000000000 ) ) ;
#6812 = VERTEX_POINT ( 'NONE', #12683 ) ;
#6813 = DIRECTION ( 'NONE',  ( 0.000000000000000000, 0.000000000000000000, -1.000000000000000000 ) ) ;
#6814 = ORIENTED_EDGE ( 'NONE', *, *, #23034, .T. ) ;
#6815 = CARTESIAN_POINT ( 'NONE',  ( -7.004531657079158258, -1.883076972206379818, -2.325406398514292761 ) ) ;
#6816 = DIRECTION ( 'NONE',  ( 1.000000000000000000, 0.000000000000000000, -0.000000000000000000 ) ) ;
#6817 = LINE ( 'NONE', #7170, #6070 ) ;
#6818 = DIRECTION ( 'NONE',  ( -1.000000000000000000, 0.000000000000000000, 0.000000000000000000 ) ) ;
#6819 = CARTESIAN_POINT ( 'NONE',  ( 10.56870887191539587, -4.787500056513357194, -1.476463073999686015 ) ) ;
#6820 = VERTEX_POINT ( 'NONE', #15517 ) ;
#6821 = EDGE_CURVE ( 'NONE', #18655, #16275, #14429, .T. ) ;
#6822 = FACE_OUTER_BOUND ( 'NONE', #19671, .T. ) ;
#6823 = ADVANCED_FACE ( 'NONE', ( #23673 ), #13457, .T. ) ;
#6824 = B_SPLINE_CURVE_WITH_KNOTS ( 'NONE', 3,
 ( #25387, #12327, #17367, #25030, #20204, #10145 ),
 .UNSPECIFIED., .F., .F.,
 ( 4, 2, 4 ),
 ( 0.000000000000000000, 0.001111101129503269625, 0.002222202259006539251 ),
 .UNSPECIFIED. ) ;
#6825 = ORIENTED_EDGE ( 'NONE', *, *, #18960, .F. ) ;
#6826 = ADVANCED_FACE ( 'NONE', ( #4678 ), #14848, .T. ) ;
#6827 = APPLICATION_PROTOCOL_DEFINITION ( 'international standard', 'config_control_design', 1994, #29135 ) ;
#6828 = CARTESIAN_POINT ( 'NONE',  ( 102.4229585137539686, -3.994976765484275827, 4.001040673959716187 ) ) ;
#6829 = DIRECTION ( 'NONE',  ( 0.4999999999999977796, 0.8660254037844398178, 0.000000000000000000 ) ) ;
#6830 = DIRECTION ( 'NONE',  ( -1.000000000000000000, 0.000000000000000000, 0.000000000000000000 ) ) ;
#6831 = ORIENTED_EDGE ( 'NONE', *, *, #995, .T. ) ;
#6832 = ORIENTED_EDGE ( 'NONE', *, *, #12853, .F. ) ;
#6833 = CARTESIAN_POINT ( 'NONE',  ( 10.52034268205830614, -3.055657119358777152, -3.641590349731960163 ) ) ;
#6834 = FACE_OUTER_BOUND ( 'NONE', #10356, .T. ) ;
#6835 = CARTESIAN_POINT ( 'NONE',  ( 23.98499999999999943, 2.486304738420679783, -0.2613211581691337604 ) ) ;
#6836 = CARTESIAN_POINT ( 'NONE',  ( 1.306676087840223266, -9.318305894662934463, -1.500000000000000000 ) ) ;
#6838 = EDGE_LOOP ( 'NONE', ( #15264, #13668, #13693, #6409 ) ) ;
#6837 = CYLINDRICAL_SURFACE ( 'NONE', #10682, 8.749000000000002331 ) ;
#6839 = CARTESIAN_POINT ( 'NONE',  ( -4.687550801365594211, 2.228590825266444142, 2.752080473201636845 ) ) ;
#6840 = DIRECTION ( 'NONE',  ( -0.000000000000000000, 0.000000000000000000, 1.000000000000000000 ) ) ;
#6841 = CARTESIAN_POINT ( 'NONE',  ( -59.41331340564917696, -5.243606251429877574, 5.221013976802370671 ) ) ;
#6842 = CARTESIAN_POINT ( 'NONE',  ( 33.00303921916322736, -0.1219419795969453463, -1.272152312594962087 ) ) ;
#6843 = VERTEX_POINT ( 'NONE', #21174 ) ;
#6845 = ORIENTED_EDGE ( 'NONE', *, *, #13133, .F. ) ;
#6844 = DIRECTION ( 'NONE',  ( 0.000000000000000000, 0.000000000000000000, 1.000000000000000000 ) ) ;
#6846 = DIRECTION ( 'NONE',  ( 1.000000000000000000, 0.000000000000000000, 0.000000000000000000 ) ) ;
#6847 = CARTESIAN_POINT ( 'NONE',  ( 32.99878091140235625, 0.000000000000000000, -1.268467860057141294 ) ) ;
#6848 = CARTESIAN_POINT ( 'NONE',  ( 24.48500000136559507, 0.9349337715887185984, -3.156283516753368268 ) ) ;
#6849 = CARTESIAN_POINT ( 'NONE',  ( -26.97068441990215959, 17.65690804191583396, 1.500000000000000000 ) ) ;
#6850 = CARTESIAN_POINT ( 'NONE',  ( -4.067282153467298045, -9.772827192342422364, -1.500000000000000000 ) ) ;
#6851 = ADVANCED_FACE ( 'NONE', ( #24324 ), #18202, .F. ) ;
#6852 = DIRECTION ( 'NONE',  ( 0.000000000000000000, 0.000000000000000000, 1.000000000000000000 ) ) ;
#6853 = CARTESIAN_POINT ( 'NONE',  ( 84.89549059757896998, -2.934676561234464742, 2.184955970506698542 ) ) ;
#6854 = CARTESIAN_POINT ( 'NONE',  ( -2.337550801365593678, 3.368539882008727115, 1.828967928396026954 ) ) ;
#6855 = VERTEX_POINT ( 'NONE', #18826 ) ;
#6856 = DIRECTION ( 'NONE',  ( -1.000000000000000000, 0.000000000000000000, 0.000000000000000000 ) ) ;
#6857 = VERTEX_POINT ( 'NONE', #26656 ) ;
#6858 = DIRECTION ( 'NONE',  ( 0.1736481776669307198, 0.000000000000000000, -0.9848077530122080203 ) ) ;
#6859 = DIRECTION ( 'NONE',  ( 1.000000000000000000, 0.000000000000000000, 0.000000000000000000 ) ) ;
#6860 = CARTESIAN_POINT ( 'NONE',  ( 3.249999999999999556, 3.174628368996190719, -8.152713396088728359 ) ) ;
#6861 = CYLINDRICAL_SURFACE ( 'NONE', #25133, 8.749000000000002331 ) ;
#6862 = EDGE_LOOP ( 'NONE', ( #27717, #15991, #24479, #18268 ) ) ;
#6863 = CARTESIAN_POINT ( 'NONE',  ( 17.32050807568873552, 10.00000000000002309, 4.629213727441584325 ) ) ;
#6864 = EDGE_LOOP ( 'NONE', ( #1038, #19327, #9749, #6012, #12226 ) ) ;
#6865 = CARTESIAN_POINT ( 'NONE',  ( 8.930755659325141593, 0.5000000000000008882, 1.500000000000000000 ) ) ;
#6867 = ORIENTED_EDGE ( 'NONE', *, *, #3895, .F. ) ;
#6866 = CARTESIAN_POINT ( 'NONE',  ( 28.69360035299894918, -5.615748452712411520, -3.993434336011448593 ) ) ;
#6868 = ORIENTED_EDGE ( 'NONE', *, *, #13651, .F. ) ;
#6869 = CARTESIAN_POINT ( 'NONE',  ( -50.81000000000000227, -10.96999999999998643, 5.700000000000000178 ) ) ;
#6870 = CARTESIAN_POINT ( 'NONE',  ( 23.93581954902093756, -2.707668749987983237, 1.915219082070892531 ) ) ;
#6872 = ORIENTED_EDGE ( 'NONE', *, *, #10127, .T. ) ;
#6871 = CARTESIAN_POINT ( 'NONE',  ( 107.7536796087345294, 16.80655079293032017, 1.395761063491601783 ) ) ;
#6873 = CARTESIAN_POINT ( 'NONE',  ( 5.612718761614564400, 4.279483796479024882, 7.013540705848194001 ) ) ;
#6874 = CARTESIAN_POINT ( 'NONE',  ( 9.065183082710470686, 0.01785380481418076190, -1.195037335522168176 ) ) ;
#6875 = ADVANCED_FACE ( 'NONE', ( #3767 ), #32016, .F. ) ;
#6876 = CARTESIAN_POINT ( 'NONE',  ( 0.000000000000000000, -1.471047635026823786, -6.892461014225975013 ) ) ;
#6877 = CARTESIAN_POINT ( 'NONE',  ( 8.996310305901872084, 0.3994363609773625701, -1.500000000000000000 ) ) ;
#6879 = ORIENTED_EDGE ( 'NONE', *, *, #30380, .T. ) ;
#6878 = CARTESIAN_POINT ( 'NONE',  ( 107.4976397712979690, -18.05149321335032297, -5.137684681196807546 ) ) ;
#6880 = DIRECTION ( 'NONE',  ( 1.000000000000000000, 0.000000000000000000, -0.000000000000000000 ) ) ;
#6881 = ADVANCED_FACE ( 'NONE', ( #29026 ), #8908, .T. ) ;
#6882 = FACE_OUTER_BOUND ( 'NONE', #4806, .T. ) ;
#6883 = CARTESIAN_POINT ( 'NONE',  ( 23.17250000136559862, -2.363507492473152283, -1.913930629741525280 ) ) ;
#6884 = CARTESIAN_POINT ( 'NONE',  ( 2.274274201625327230, -7.958834565716822240, 7.593217523260554103 ) ) ;
#6885 = B_SPLINE_CURVE_WITH_KNOTS ( 'NONE', 3,
 ( #20181, #32903, #30555, #17650, #25519, #14810, #11996, #32556, #14660, #12301 ),
 .UNSPECIFIED., .F., .F.,
 ( 4, 2, 2, 2, 4 ),
 ( 0.000000000000000000, 0.0003410365069723375565, 0.0006820730139446751130, 0.001023109520917012561, 0.001364146027889350226 ),
 .UNSPECIFIED. ) ;
#6886 = FACE_OUTER_BOUND ( 'NONE', #25031, .T. ) ;
#6887 = DIRECTION ( 'NONE',  ( 0.000000000000000000, 0.2588190451025318417, -0.9659258262890653146 ) ) ;
#6888 = VERTEX_POINT ( 'NONE', #29630 ) ;
#6889 = DIRECTION ( 'NONE',  ( -8.281886410780492538E-17, -0.9659258262890664248, -0.2588190451025276229 ) ) ;
#6890 = EDGE_CURVE ( 'NONE', #23561, #30055, #23924, .T. ) ;
#6891 = CARTESIAN_POINT ( 'NONE',  ( -2.242109179563498866, -0.3178988483021057410, 3.024605502323848949 ) ) ;
#6892 = ADVANCED_FACE ( 'NONE', ( #6711 ), #27095, .F. ) ;
#6893 = CARTESIAN_POINT ( 'NONE',  ( -23.35000000000000142, -10.96966150227469505, -11.00000000000000000 ) ) ;
#6894 = ORIENTED_EDGE ( 'NONE', *, *, #5540, .F. ) ;
#6895 = DIRECTION ( 'NONE',  ( -1.000000000000000000, -0.000000000000000000, -0.000000000000000000 ) ) ;
#6896 = CARTESIAN_POINT ( 'NONE',  ( 2.692942092879388127, -0.02443046219423555473, -1.307625729273671933 ) ) ;
#6897 = ORIENTED_EDGE ( 'NONE', *, *, #13405, .F. ) ;
#6898 = CARTESIAN_POINT ( 'NONE',  ( 7.153595758147059946, -6.747833800172327479, 1.000000000000000222 ) ) ;
#6899 = EDGE_CURVE ( 'NONE', #3652, #1130, #16562, .T. ) ;
#6900 = ORIENTED_EDGE ( 'NONE', *, *, #28690, .T. ) ;
#6901 = VERTEX_POINT ( 'NONE', #14365 ) ;
#6902 = DIRECTION ( 'NONE',  ( 0.000000000000000000, 0.000000000000000000, -1.000000000000000000 ) ) ;
#6904 = VERTEX_POINT ( 'NONE', #26765 ) ;
#6903 = DIRECTION ( 'NONE',  ( 0.9896144216807900573, 8.583536847274380671E-16, 0.1437473352845037577 ) ) ;
#6905 = VERTEX_POINT ( 'NONE', #1382 ) ;
#6906 = CARTESIAN_POINT ( 'NONE',  ( 23.48500000136559862, 2.892927487894327410, -1.570731468192931635 ) ) ;
#6907 = EDGE_CURVE ( 'NONE', #140, #697, #11110, .T. ) ;
#6909 = ORIENTED_EDGE ( 'NONE', *, *, #25996, .F. ) ;
#6908 = VECTOR ( 'NONE', #2607, 1000.000000000000000 ) ;
#6910 = FACE_OUTER_BOUND ( 'NONE', #2400, .T. ) ;
#6911 = CARTESIAN_POINT ( 'NONE',  ( -4.317168503051449946, -7.715934794172482292, 1.500000000000000000 ) ) ;
#6913 = ORIENTED_EDGE ( 'NONE', *, *, #10816, .F. ) ;
#6912 = CARTESIAN_POINT ( 'NONE',  ( 29.33166896510681099, -3.955587949931513858, -1.529339504155426743 ) ) ;
#6914 = VECTOR ( 'NONE', #22868, 1000.000000000000000 ) ;
#6915 = CARTESIAN_POINT ( 'NONE',  ( 0.000000000000000000, 0.000000000000000000, 0.000000000000000000 ) ) ;
#6916 = CARTESIAN_POINT ( 'NONE',  ( 26.05774446050084237, 21.87587288138687214, -4.999054092451833853 ) ) ;
#6917 = CARTESIAN_POINT ( 'NONE',  ( 22.86000000136559507, -0.9349337715887248157, 3.156283516753367824 ) ) ;
#6918 = CARTESIAN_POINT ( 'NONE',  ( 3.499999999999999556, -2.861184399891040009, 6.440778198864103743 ) ) ;
#6919 = CIRCLE ( 'NONE', #5314, 5.010000000000000675 ) ;
#6920 = DIRECTION ( 'NONE',  ( 0.000000000000000000, 0.000000000000000000, 1.000000000000000000 ) ) ;
#6921 = DIRECTION ( 'NONE',  ( -1.000000000000000000, 4.336808689942013792E-15, 0.000000000000000000 ) ) ;
#6922 = LINE ( 'NONE', #17118, #22131 ) ;
#6923 = EDGE_CURVE ( 'NONE', #6099, #23179, #23545, .T. ) ;
#6924 = CARTESIAN_POINT ( 'NONE',  ( 21.50111451137534146, -3.256483526998273983E-15, 2.499999999999998668 ) ) ;
#6925 = EDGE_CURVE ( 'NONE', #1564, #32584, #21425, .T. ) ;
#6926 = CARTESIAN_POINT ( 'NONE',  ( -5.834205823644825095, 18.00000000000000355, -2.241549108841658366 ) ) ;
#6927 = LINE ( 'NONE', #24167, #17210 ) ;
#6928 = EDGE_CURVE ( 'NONE', #5778, #32283, #21912, .T. ) ;
#6929 = CARTESIAN_POINT ( 'NONE',  ( 102.8580990270160385, -4.820463887425400884, 4.522129901861163148 ) ) ;
#6930 = EDGE_CURVE ( 'NONE', #25757, #11409, #1211, .T. ) ;
#6931 = CARTESIAN_POINT ( 'NONE',  ( -6.100050802731187716, 1.549418761218566143, -2.853674364686379583 ) ) ;
#6932 = VERTEX_POINT ( 'NONE', #31642 ) ;
#6933 = CARTESIAN_POINT ( 'NONE',  ( -4.100050799999999995, -0.3135853898029607456, 2.983565686104819648 ) ) ;
#6934 = AXIS2_PLACEMENT_3D ( 'NONE', #21801, #32007, #14266 ) ;
#6935 = CARTESIAN_POINT ( 'NONE',  ( 21.97279447062591018, -21.86582820552294493, -1.264434309188650518 ) ) ;
#6936 = CARTESIAN_POINT ( 'NONE',  ( 10.55147673363119232, -2.376879293651037006, -4.116875700062107235 ) ) ;
#6937 = ORIENTED_EDGE ( 'NONE', *, *, #7108, .F. ) ;
#6938 = DIRECTION ( 'NONE',  ( -1.000000000000000000, 8.574039729943019576E-17, -0.000000000000000000 ) ) ;
#6939 = DIRECTION ( 'NONE',  ( -1.000000000000000000, 0.000000000000000000, -0.000000000000000000 ) ) ;
#6940 = AXIS2_PLACEMENT_3D ( 'NONE', #25327, #17798, #9770 ) ;
#6941 = ORIENTED_EDGE ( 'NONE', *, *, #24802, .F. ) ;
#6942 = CARTESIAN_POINT ( 'NONE',  ( 7.167971118698460486, -13.96529319322445062, 1.755547229797913333 ) ) ;
#6943 = SHAPE_DEFINITION_REPRESENTATION ( #24407, #27351 ) ;
#6944 = CARTESIAN_POINT ( 'NONE',  ( 10.52034268205830614, 3.055657119358800244, 3.641590349731939735 ) ) ;
#6945 = ORIENTED_EDGE ( 'NONE', *, *, #19183, .T. ) ;
#6946 = CARTESIAN_POINT ( 'NONE',  ( -4.497573025205830355, -5.387589684568504289, 1.499999999999999556 ) ) ;
#6947 = EDGE_CURVE ( 'NONE', #30847, #20064, #17878, .T. ) ;
#6948 = CC_DESIGN_DATE_AND_TIME_ASSIGNMENT ( #19548, #12171, ( #26353 ) ) ;
#6949 = DIRECTION ( 'NONE',  ( 0.4999999999999978906, 0.8660254037844398178, 0.000000000000000000 ) ) ;
#6950 = CARTESIAN_POINT ( 'NONE',  ( 28.66730804928445764, -6.639321322089450916, -4.155404940063424313 ) ) ;
#6951 = CARTESIAN_POINT ( 'NONE',  ( 56.97280603064898941, -277.2763395528616002, -2.806473568333505142 ) ) ;
#6952 = LINE ( 'NONE', #25004, #2719 ) ;
#6953 = ORIENTED_EDGE ( 'NONE', *, *, #235, .T. ) ;
#6954 = VECTOR ( 'NONE', #24187, 1000.000000000000000 ) ;
#6955 = CARTESIAN_POINT ( 'NONE',  ( -2.775371991354582679, -0.000000000000000000, 1.260159510457126819 ) ) ;
#6956 = CARTESIAN_POINT ( 'NONE',  ( 23.00622743562070482, -21.91302709721476205, -1.171678142438169701 ) ) ;
#6957 = CYLINDRICAL_SURFACE ( 'NONE', #17260, 0.5000000000000000000 ) ;
#6959 = VERTEX_POINT ( 'NONE', #31807 ) ;
#6958 = DIRECTION ( 'NONE',  ( 0.9896144216807900573, -1.102680533460266556E-16, 0.1437473352845034802 ) ) ;
#6960 = CARTESIAN_POINT ( 'NONE',  ( 26.29336354336542314, 19.59588486419538711, -5.471072653611049219 ) ) ;
#6961 = AXIS2_PLACEMENT_3D ( 'NONE', #10432, #17961, #7262 ) ;
#6962 = CARTESIAN_POINT ( 'NONE',  ( -2.386718424894326063, -9.330009425477191698, -4.522129901861166701 ) ) ;
#6963 = DIRECTION ( 'NONE',  ( 0.000000000000000000, -0.8191520442889844711, -0.5735764363510564845 ) ) ;
#6964 = DIRECTION ( 'NONE',  ( 1.387778780781445676E-14, 0.000000000000000000, -1.000000000000000000 ) ) ;
#6965 = AXIS2_PLACEMENT_3D ( 'NONE', #6796, #22341, #16983 ) ;
#6966 = EDGE_CURVE ( 'NONE', #2672, #7938, #4051, .T. ) ;
#6967 = CARTESIAN_POINT ( 'NONE',  ( 6.037141812302426302, -1.028012177296142582, 8.411869123983613861 ) ) ;
#6968 = CARTESIAN_POINT ( 'NONE',  ( 25.29730119701314450, -17.51801463888119059, -1.124408821416490900 ) ) ;
#6969 = PLANE ( 'NONE',  #18812 ) ;
#6970 = FACE_OUTER_BOUND ( 'NONE', #21958, .T. ) ;
#6971 = ORIENTED_EDGE ( 'NONE', *, *, #10989, .T. ) ;
#6972 = CARTESIAN_POINT ( 'NONE',  ( -56.28351068137280322, 0.4500000000000000111, 0.000000000000000000 ) ) ;
#6973 = ORIENTED_EDGE ( 'NONE', *, *, #13108, .T. ) ;
#6974 = CARTESIAN_POINT ( 'NONE',  ( -5.654531657079158613, -1.545410377633946286, 2.846291840500174697 ) ) ;
#6975 = CARTESIAN_POINT ( 'NONE',  ( 4.749760686538667009, -5.151476664237435443, -6.139290821770307716 ) ) ;
#6976 = AXIS2_PLACEMENT_3D ( 'NONE', #2356, #17697, #27912 ) ;
#6977 = CARTESIAN_POINT ( 'NONE',  ( 85.25075202023842280, -3.924039320687039645, -5.695980980372493008 ) ) ;
#6978 = AXIS2_PLACEMENT_3D ( 'NONE', #20826, #18327, #17998 ) ;
#6979 = CARTESIAN_POINT ( 'NONE',  ( 10.00000000000000178, 2.718385644597235196, -4.208382051008164204 ) ) ;
#6980 = DIRECTION ( 'NONE',  ( 0.000000000000000000, -0.9961946980917449901, -0.08715574274766552110 ) ) ;
#6981 = ORIENTED_EDGE ( 'NONE', *, *, #1744, .F. ) ;
#6982 = CARTESIAN_POINT ( 'NONE',  ( -48.50000000000000000, -10.96966150227468972, 7.500000000000000000 ) ) ;
#6983 = AXIS2_PLACEMENT_3D ( 'NONE', #16670, #30067, #17166 ) ;
#6984 = VECTOR ( 'NONE', #11011, 1000.000000000000000 ) ;
#6985 = CIRCLE ( 'NONE', #13910, 5.009999999999999787 ) ;
#6986 = ORIENTED_EDGE ( 'NONE', *, *, #29059, .T. ) ;
#6987 = PERSON_AND_ORGANIZATION_ROLE ( 'creator' ) ;
#6988 = CARTESIAN_POINT ( 'NONE',  ( 69.07013463293527877, -6.110056736244218634, 4.003575175709323197 ) ) ;
#6989 = ADVANCED_FACE ( 'NONE', ( #26189, #29525 ), #16312, .T. ) ;
#6990 = AXIS2_PLACEMENT_3D ( 'NONE', #28598, #10531, #501 ) ;
#6991 = DIRECTION ( 'NONE',  ( 0.000000000000000000, 0.000000000000000000, -1.000000000000000000 ) ) ;
#6993 = CARTESIAN_POINT ( 'NONE',  ( 7.249760686538667009, 8.385837730238846314E-14, -8.014274990069656823 ) ) ;
#6992 = DIRECTION ( 'NONE',  ( -1.000000000000000000, 0.000000000000000000, 0.000000000000000000 ) ) ;
#6994 = ORIENTED_EDGE ( 'NONE', *, *, #13624, .T. ) ;
#6995 = CARTESIAN_POINT ( 'NONE',  ( 56.97280603064898941, -277.2763395528616002, 2.806473568333438084 ) ) ;
#6996 = DIRECTION ( 'NONE',  ( -1.000000000000000000, 0.000000000000000000, 0.000000000000000000 ) ) ;
#6997 = CARTESIAN_POINT ( 'NONE',  ( 24.17250000136559507, -3.024605502323851169, 0.3178988483021052969 ) ) ;
#6998 = CARTESIAN_POINT ( 'NONE',  ( 6.555809470822123508, -13.70807884655583742, -1.755773249082955623 ) ) ;
#7000 = VERTEX_POINT ( 'NONE', #11619 ) ;
#6999 = DIRECTION ( 'NONE',  ( -1.000000000000000000, 0.000000000000000000, -0.000000000000000000 ) ) ;
#7001 = CARTESIAN_POINT ( 'NONE',  ( -3.887550801365593500, 2.228590825266444142, 2.752080473201636845 ) ) ;
#7002 = FACE_OUTER_BOUND ( 'NONE', #18663, .T. ) ;
#7003 = CIRCLE ( 'NONE', #29978, 5.009999999999999787 ) ;
#7004 = CARTESIAN_POINT ( 'NONE',  ( 2.357329895872517511, -10.75444571268657334, -1.335530315079643593 ) ) ;
#7005 = DIRECTION ( 'NONE',  ( 0.000000000000000000, 1.687538997430237626E-14, 1.000000000000000000 ) ) ;
#7006 = ORIENTED_EDGE ( 'NONE', *, *, #15477, .F. ) ;
#7007 = EDGE_CURVE ( 'NONE', #31320, #31825, #21944, .T. ) ;
#7009 = ORIENTED_EDGE ( 'NONE', *, *, #22399, .F. ) ;
#7008 = CARTESIAN_POINT ( 'NONE',  ( 21.08401840680222961, -16.78474387324145667, 1.499999999999999556 ) ) ;
#7010 = EDGE_CURVE ( 'NONE', #30724, #1352, #6428, .T. ) ;
#7011 = VECTOR ( 'NONE', #23159, 1000.000000000000000 ) ;
#7012 = CIRCLE ( 'NONE', #28380, 8.749000000000002331 ) ;
#7014 = AXIS2_PLACEMENT_3D ( 'NONE', #32402, #29366, #12604 ) ;
#7013 = CARTESIAN_POINT ( 'NONE',  ( 3.063284526839887167, 5.538577986808899567, 6.772677083992407532 ) ) ;
#7015 = EDGE_CURVE ( 'NONE', #11567, #15410, #31039, .T. ) ;
#7016 = CARTESIAN_POINT ( 'NONE',  ( 5.612974044843318744, 8.054452210044761529, 1.622927203279369346 ) ) ;
#7017 = AXIS2_PLACEMENT_3D ( 'NONE', #23616, #3091, #5097 ) ;
#7018 = CARTESIAN_POINT ( 'NONE',  ( -18.23565129703368726, 15.66456206417224806, 1.840856759657562680 ) ) ;
#7019 = VECTOR ( 'NONE', #21953, 1000.000000000000114 ) ;
#7020 = CARTESIAN_POINT ( 'NONE',  ( 14.53974964220209110, -20.67385035929880743, -1.499999999999056088 ) ) ;
#7021 = CIRCLE ( 'NONE', #5440, 10.99999999999999822 ) ;
#7022 = CARTESIAN_POINT ( 'NONE',  ( 0.9499999999999995115, 0.000000000000000000, 0.000000000000000000 ) ) ;
#7023 = DIRECTION ( 'NONE',  ( -1.000000000000000000, -0.000000000000000000, -0.000000000000000000 ) ) ;
#7024 = DIRECTION ( 'NONE',  ( 1.000000000000000000, -0.000000000000000000, -0.000000000000000000 ) ) ;
#7025 = ORIENTED_EDGE ( 'NONE', *, *, #22706, .T. ) ;
#7026 = CARTESIAN_POINT ( 'NONE',  ( 0.000000000000000000, 9.915734732513282523, -4.762163868918167786 ) ) ;
#7027 = ORIENTED_EDGE ( 'NONE', *, *, #11089, .F. ) ;
#7028 = CARTESIAN_POINT ( 'NONE',  ( 0.000000000000000000, 19.50000000000000000, 0.000000000000000000 ) ) ;
#7030 = VECTOR ( 'NONE', #2721, 1000.000000000000000 ) ;
#7029 =( LENGTH_UNIT ( ) NAMED_UNIT ( * ) SI_UNIT ( .MILLI., .METRE. ) );
#7031 = CARTESIAN_POINT ( 'NONE',  ( 2.661997627134204070, 6.664939678585267480, -7.629706518865775777 ) ) ;
#7032 = ORIENTED_EDGE ( 'NONE', *, *, #10444, .T. ) ;
#7033 = AXIS2_PLACEMENT_3D ( 'NONE', #10483, #10129, #25693 ) ;
#7034 = VECTOR ( 'NONE', #3778, 1000.000000000000114 ) ;
#7035 =( BOUNDED_SURFACE ( )  B_SPLINE_SURFACE ( 1, 3, ( 
 ( #32839, #9738, #19966, #22785 ),
 ( #10061, #20274, #12235, #12411 ) ),
 .UNSPECIFIED., .F., .F., .F. ) 
 B_SPLINE_SURFACE_WITH_KNOTS ( ( 2, 2 ),
 ( 4, 4 ),
 ( 0.000000000000000000, 1.000000000000000000 ),
 ( 0.000000000000000000, 1.000000000000000000 ),
 .UNSPECIFIED. ) 
 GEOMETRIC_REPRESENTATION_ITEM ( )  RATIONAL_B_SPLINE_SURFACE ( (
 ( 1.000000000000000000, 0.9917560313531952332, 0.9917560313531952332, 1.000000000000000000),
 ( 1.000000000000000000, 0.9917560313531952332, 0.9917560313531952332, 1.000000000000000000) ) ) 
 REPRESENTATION_ITEM ( '' )  SURFACE ( )  );
#7036 = DIRECTION ( 'NONE',  ( 0.000000000000000000, 0.000000000000000000, 1.000000000000000000 ) ) ;
#7037 = VECTOR ( 'NONE', #30778, 1000.000000000000000 ) ;
#7038 = ORIENTED_EDGE ( 'NONE', *, *, #1877, .F. ) ;
#7039 = DIRECTION ( 'NONE',  ( -0.06927878976713691683, 0.9975973382524639943, 0.000000000000000000 ) ) ;
#7041 = ORIENTED_EDGE ( 'NONE', *, *, #14680, .T. ) ;
#7040 = CARTESIAN_POINT ( 'NONE',  ( 84.96637968728258272, -4.072042218960389093, -4.013697180992776836 ) ) ;
#7042 = ORIENTED_EDGE ( 'NONE', *, *, #13830, .F. ) ;
#7043 = AXIS2_PLACEMENT_3D ( 'NONE', #7844, #5516, #20565 ) ;
#7044 = CARTESIAN_POINT ( 'NONE',  ( 2.990310703069061216, -7.668352627376187058, 4.902153806112375278 ) ) ;
#7045 = CIRCLE ( 'NONE', #24157, 8.750000000000000000 ) ;
#7047 = AXIS2_PLACEMENT_3D ( 'NONE', #20379, #7679, #5168 ) ;
#7046 = DIRECTION ( 'NONE',  ( -0.4999999999999977240, -0.8660254037844399289, 0.000000000000000000 ) ) ;
#7048 = EDGE_CURVE ( 'NONE', #10288, #28142, #22502, .T. ) ;
#7050 = ORIENTED_EDGE ( 'NONE', *, *, #1744, .T. ) ;
#7049 = DIRECTION ( 'NONE',  ( -0.000000000000000000, -0.2588190451025252359, 0.9659258262890669799 ) ) ;
#7051 = DIRECTION ( 'NONE',  ( 0.000000000000000000, 0.000000000000000000, 1.000000000000000000 ) ) ;
#7052 = CARTESIAN_POINT ( 'NONE',  ( -3.672954038633582391E-13, 4.709950686175357504, 9.884132761439534676 ) ) ;
#7053 = CARTESIAN_POINT ( 'NONE',  ( -4.184188163278487416, -5.072310292433697576, 1.499999999999960254 ) ) ;
#7054 = CARTESIAN_POINT ( 'NONE',  ( 7.637044423815050109, -3.948987408040151248, -1.000000000000000000 ) ) ;
#7055 = EDGE_CURVE ( 'NONE', #10039, #20330, #14130, .T. ) ;
#7057 = VERTEX_POINT ( 'NONE', #1289 ) ;
#7056 = CARTESIAN_POINT ( 'NONE',  ( 107.9522086517191468, -17.38117859037711810, -4.648913506406474383 ) ) ;
#7058 = CARTESIAN_POINT ( 'NONE',  ( 7.249760686538667009, 6.735557395310442023E-16, -5.500000000000000000 ) ) ;
#7059 = EDGE_CURVE ( 'NONE', #25696, #14457, #8792, .T. ) ;
#7060 = AXIS2_PLACEMENT_3D ( 'NONE', #247, #18440, #2569 ) ;
#7061 = VECTOR ( 'NONE', #18788, 1000.000000000000227 ) ;
#7062 = DIRECTION ( 'NONE',  ( -1.000000000000000000, 8.574039729943017111E-17, -3.081487911019577365E-33 ) ) ;
#7063 = CARTESIAN_POINT ( 'NONE',  ( 24.73500000136559507, 1.570731468192929858, 2.892927487894329186 ) ) ;
#7064 = AXIS2_PLACEMENT_3D ( 'NONE', #28918, #31780, #20907 ) ;
#7065 = AXIS2_PLACEMENT_3D ( 'NONE', #6869, #9386, #2201 ) ;
#7066 = CARTESIAN_POINT ( 'NONE',  ( 108.1156589233279135, 18.82219444680288589, -4.397958565568439226 ) ) ;
#7067 = AXIS2_PLACEMENT_3D ( 'NONE', #12653, #25020, #10131 ) ;
#7068 = CARTESIAN_POINT ( 'NONE',  ( 9.999999999999998224, -4.753758587302148619, 3.462581523170091167E-33 ) ) ;
#7069 = CARTESIAN_POINT ( 'NONE',  ( 0.000000000000000000, -25.93932300454937945, 11.00000000000000000 ) ) ;
#7070 = VERTEX_POINT ( 'NONE', #23684 ) ;
#7071 = DIRECTION ( 'NONE',  ( 8.541412920197216117E-17, 0.9961946980917452121, 0.08715574274766195451 ) ) ;
#7072 = B_SPLINE_CURVE_WITH_KNOTS ( 'NONE', 3,
 ( #29116, #13557, #1369, #26752, #3697, #5860, #31308, #11545 ),
 .UNSPECIFIED., .F., .F.,
 ( 4, 2, 2, 4 ),
 ( 0.000000000000000000, 0.0002326964511452904059, 0.0004653929022905808118, 0.0009307858045811711646 ),
 .UNSPECIFIED. ) ;
#7073 = CLOSED_SHELL ( 'NONE', ( #28326, #18885, #32916, #8247, #28388, #8330, #7790, #11076, #6680, #8150, #21838, #18049, #6875, #17947, #396, #631, #12147, #27412, #8862, #7631, #30758, #32373, #30820, #12768, #22754, #5876, #11722, #7548, #31460, #14262, #1461, #24447, #14483, #10796, #23327, #24257, #17525, #31274, #31513, #32275, #25989, #4385, #22427, #28189, #26720, #17540, #16723, #6826, #567, #32500, #10097, #3182, #558, #10226, #17170, #32207, #4483, #12440, #20586, #10755, #24076, #13608, #5291, #16514, #2428, #29476, #32929, #23517, #13579, #8678 ) ) ;
#7074 = AXIS2_PLACEMENT_3D ( 'NONE', #4814, #28211, #5313 ) ;
#7075 = PLANE ( 'NONE',  #4402 ) ;
#7076 = CARTESIAN_POINT ( 'NONE',  ( -5.187550801365593323, -3.521866450007987037, -0.3701630799359323931 ) ) ;
#7077 = ORIENTED_EDGE ( 'NONE', *, *, #15541, .F. ) ;
#7078 = CONICAL_SURFACE ( 'NONE', #14001, 8.000000000000000000, 0.03490658503988666728 ) ;
#7079 = CARTESIAN_POINT ( 'NONE',  ( -50.81000000000000227, -10.96999999999998643, 1.500000000000000000 ) ) ;
#7080 = CARTESIAN_POINT ( 'NONE',  ( 1.386174007446685286, -9.662292653395718744, -0.9788672205888330202 ) ) ;
#7081 = ORIENTED_EDGE ( 'NONE', *, *, #2150, .F. ) ;
#7082 = CARTESIAN_POINT ( 'NONE',  ( -32.37020706055090358, 18.00000000000000355, 0.7246014581832563861 ) ) ;
#7083 = EDGE_LOOP ( 'NONE', ( #8512, #5227, #32262, #4383, #7950, #26476, #29095, #6745 ) ) ;
#7084 = VECTOR ( 'NONE', #11959, 1000.000000000000000 ) ;
#7085 = ORIENTED_EDGE ( 'NONE', *, *, #7324, .T. ) ;
#7086 = DIRECTION ( 'NONE',  ( -1.000000000000000000, 8.574039729943018344E-17, -0.000000000000000000 ) ) ;
#7087 = EDGE_CURVE ( 'NONE', #18253, #11141, #29418, .T. ) ;
#7088 = VECTOR ( 'NONE', #24914, 1000.000000000000000 ) ;
#7090 = ORIENTED_EDGE ( 'NONE', *, *, #19773, .F. ) ;
#7089 = DIRECTION ( 'NONE',  ( -0.000000000000000000, -0.000000000000000000, -1.000000000000000000 ) ) ;
#7091 = ORIENTED_EDGE ( 'NONE', *, *, #21484, .F. ) ;
#7092 = CARTESIAN_POINT ( 'NONE',  ( 21.36000000136559507, 0.9349337715887185984, -3.156283516753368268 ) ) ;
#7093 = CONICAL_SURFACE ( 'NONE', #23113, 2.499999999999996891, 1.029744258676653867 ) ;
#7094 = CIRCLE ( 'NONE', #23630, 8.500000000000000000 ) ;
#7095 = VERTEX_POINT ( 'NONE', #13633 ) ;
#7096 = CARTESIAN_POINT ( 'NONE',  ( 108.1288400433390393, -19.92462668933126579, -1.384270303710054328 ) ) ;
#7097 = EDGE_CURVE ( 'NONE', #20949, #33081, #1955, .T. ) ;
#7099 = ORIENTED_EDGE ( 'NONE', *, *, #4743, .T. ) ;
#7098 = CYLINDRICAL_SURFACE ( 'NONE', #16545, 2.099999999999997868 ) ;
#7100 = DIRECTION ( 'NONE',  ( -1.000000000000000000, 0.000000000000000000, 0.000000000000000000 ) ) ;
#7101 = EDGE_CURVE ( 'NONE', #937, #8978, #20361, .T. ) ;
#7102 =( GEOMETRIC_REPRESENTATION_CONTEXT ( 3 ) GLOBAL_UNCERTAINTY_ASSIGNED_CONTEXT ( ( #25882 ) ) GLOBAL_UNIT_ASSIGNED_CONTEXT ( ( #7029, #25074, #11267 ) ) REPRESENTATION_CONTEXT ( 'NONE', 'WORKASPACE' ) );
#7103 = CARTESIAN_POINT ( 'NONE',  ( 5.865515302491369987, 15.00000000000000178, -1.491740999229417941 ) ) ;
#7104 = CARTESIAN_POINT ( 'NONE',  ( 21.23500000136559507, -3.156283516753370044, -0.9349337715887220401 ) ) ;
#7105 = DIRECTION ( 'NONE',  ( -1.000000000000000000, 0.000000000000000000, -0.000000000000000000 ) ) ;
#7106 = CIRCLE ( 'NONE', #2238, 8.749000000000002331 ) ;
#7107 = CARTESIAN_POINT ( 'NONE',  ( -1.694237876702965329, -1.500727999663087564, -4.522129901861166701 ) ) ;
#7108 = EDGE_CURVE ( 'NONE', #16352, #10254, #31380, .T. ) ;
#7109 = CARTESIAN_POINT ( 'NONE',  ( -34.48223484310472031, 0.5000000000000000000, 2.552009564962238741 ) ) ;
#7110 = CARTESIAN_POINT ( 'NONE',  ( -50.81000000000000227, -10.96999999999998643, 5.500000000000000000 ) ) ;
#7111 = DIRECTION ( 'NONE',  ( -0.000000000000000000, -0.3746065934159164001, 0.9271838545667856479 ) ) ;
#7112 = CARTESIAN_POINT ( 'NONE',  ( 6.270432871727738444, -15.60322400927903175, 5.485967528433933538 ) ) ;
#7113 = AXIS2_PLACEMENT_3D ( 'NONE', #31371, #5936, #5294 ) ;
#7114 = FACE_OUTER_BOUND ( 'NONE', #23484, .T. ) ;
#7115 = CARTESIAN_POINT ( 'NONE',  ( 19.01480233880806381, -3.011762293215139330, -0.02339150518254430253 ) ) ;
#7116 = AXIS2_PLACEMENT_3D ( 'NONE', #23848, #465, #23357 ) ;
#7117 = ADVANCED_FACE ( 'NONE', ( #948 ), #18649, .F. ) ;
#7118 = AXIS2_PLACEMENT_3D ( 'NONE', #27668, #20012, #25496 ) ;
#7119 = CARTESIAN_POINT ( 'NONE',  ( 0.1606232872981965543, -2.144970499001195297, -10.41111328665008529 ) ) ;
#7120 = CARTESIAN_POINT ( 'NONE',  ( -2.800050802731187005, 3.113457007523260156, -0.9222479816126439855 ) ) ;
#7121 = ORIENTED_EDGE ( 'NONE', *, *, #18571, .T. ) ;
#7122 = VECTOR ( 'NONE', #5193, 1000.000000000000000 ) ;
#7124 = EDGE_CURVE ( 'NONE', #8068, #13727, #21662, .T. ) ;
#7123 = AXIS2_PLACEMENT_3D ( 'NONE', #2372, #20089, #32307 ) ;
#7125 = CARTESIAN_POINT ( 'NONE',  ( -3.300050800000000173, -0.3135853898029607456, 2.983565686104819648 ) ) ;
#7126 = LINE ( 'NONE', #4617, #17266 ) ;
#7127 = CARTESIAN_POINT ( 'NONE',  ( -4.500050800000000351, 0.3135853898029611342, -2.983565686104819648 ) ) ;
#7128 = SECURITY_CLASSIFICATION ( '', '', #21565 ) ;
#7129 = ORIENTED_EDGE ( 'NONE', *, *, #26945, .T. ) ;
#7130 = DIRECTION ( 'NONE',  ( 1.000000000000000000, 0.000000000000000000, 0.000000000000000000 ) ) ;
#7131 =( NAMED_UNIT ( * ) SI_UNIT ( $, .STERADIAN. ) SOLID_ANGLE_UNIT ( ) );
#7132 = EDGE_CURVE ( 'NONE', #11567, #3025, #28849, .T. ) ;
#7133 = VERTEX_POINT ( 'NONE', #29334 ) ;
#7134 = CARTESIAN_POINT ( 'NONE',  ( 10.91172402966645905, -15.11896842049539380, 1.500000000000139000 ) ) ;
#7135 = SECURITY_CLASSIFICATION_LEVEL ( 'unclassified' ) ;
#7136 = CARTESIAN_POINT ( 'NONE',  ( -2.912942406915326909, 4.884725290497410777E-15, -2.999999999999999556 ) ) ;
#7137 = VERTEX_POINT ( 'NONE', #11299 ) ;
#7138 = CARTESIAN_POINT ( 'NONE',  ( -4.526559146999415972, -7.591385338581535969, 1.500000000000000222 ) ) ;
#7139 = ORIENTED_EDGE ( 'NONE', *, *, #921, .F. ) ;
#7140 = CARTESIAN_POINT ( 'NONE',  ( 7.249760686538667009, 6.139290821770327256, -5.151476664237414127 ) ) ;
#7141 = VECTOR ( 'NONE', #15431, 1000.000000000000227 ) ;
#7142 = CARTESIAN_POINT ( 'NONE',  ( 9.302055952181040865, 0.2457637073014105056, -1.050000000000000044 ) ) ;
#7143 = CARTESIAN_POINT ( 'NONE',  ( 3.499999999999999556, 1.418488851014406693, 6.085876303339381899 ) ) ;
#7144 = PLANE ( 'NONE',  #6965 ) ;
#7145 = ORIENTED_EDGE ( 'NONE', *, *, #4088, .F. ) ;
#7146 = EDGE_CURVE ( 'NONE', #6630, #115, #16632, .T. ) ;
#7147 = VECTOR ( 'NONE', #11438, 1000.000000000000000 ) ;
#7148 = EDGE_CURVE ( 'NONE', #32996, #10544, #30197, .T. ) ;
#7149 = CIRCLE ( 'NONE', #25847, 5.009999999999999787 ) ;
#7150 = CARTESIAN_POINT ( 'NONE',  ( 108.5619817448483531, 15.65002148400673754, 0.4463807625373211185 ) ) ;
#7152 = ORIENTED_EDGE ( 'NONE', *, *, #2840, .F. ) ;
#7151 = CARTESIAN_POINT ( 'NONE',  ( -7.077711312404582636E-17, -0.8254815157535566605, 4.681538312723514395 ) ) ;
#7153 = CARTESIAN_POINT ( 'NONE',  ( 3.499999999999999556, 0.000000000000000000, 0.000000000000000000 ) ) ;
#7154 = CARTESIAN_POINT ( 'NONE',  ( 21.50111451137534146, -3.256483526998273983E-15, 2.499999999999998668 ) ) ;
#7155 = DIRECTION ( 'NONE',  ( -1.000000000000000000, -0.000000000000000000, -0.000000000000000000 ) ) ;
#7156 = FACE_OUTER_BOUND ( 'NONE', #19474, .T. ) ;
#7157 = CARTESIAN_POINT ( 'NONE',  ( -50.60000000000000142, -0.5000000000000000000, -1.000000000000000000 ) ) ;
#7158 = LOCAL_TIME ( 16, 7, 10.00000000000000000, #10149 ) ;
#7159 = EDGE_CURVE ( 'NONE', #4619, #32326, #18683, .T. ) ;
#7160 = DIRECTION ( 'NONE',  ( -1.000000000000000000, 8.574039729943018344E-17, -0.000000000000000000 ) ) ;
#7161 = CARTESIAN_POINT ( 'NONE',  ( 2.274274201625327230, 0.000000000000000000, 0.000000000000000000 ) ) ;
#7162 = CARTESIAN_POINT ( 'NONE',  ( -56.32730583845947336, 0.4233724216868345325, -1.495526720789816189 ) ) ;
#7163 = DIRECTION ( 'NONE',  ( 0.4999999999999978351, 0.8660254037844398178, 0.000000000000000000 ) ) ;
#7164 = ORIENTED_EDGE ( 'NONE', *, *, #740, .F. ) ;
#7165 = DIRECTION ( 'NONE',  ( -1.000000000000000000, 8.574039729943018344E-17, -0.000000000000000000 ) ) ;
#7166 = VERTEX_POINT ( 'NONE', #11969 ) ;
#7167 = EDGE_CURVE ( 'NONE', #13750, #4019, #11286, .T. ) ;
#7168 = CARTESIAN_POINT ( 'NONE',  ( -7.704531657079157547, 0.3127741368606810068, -2.975847129947406522 ) ) ;
#7169 = CARTESIAN_POINT ( 'NONE',  ( 109.0480074564792261, 18.35640442295476404, 5.421406144741463429 ) ) ;
#7170 = CARTESIAN_POINT ( 'NONE',  ( 10.52034268205830614, -3.407865132560155885, -3.672404558090073490 ) ) ;
#7171 = DIRECTION ( 'NONE',  ( 0.000000000000000000, 0.000000000000000000, 1.000000000000000000 ) ) ;
#7172 = CARTESIAN_POINT ( 'NONE',  ( 10.52034268205830614, -3.055657119358777152, -3.641590349731960163 ) ) ;
#7173 = ORIENTED_EDGE ( 'NONE', *, *, #6276, .F. ) ;
#7174 = DIRECTION ( 'NONE',  ( -0.000000000000000000, 0.5735764363510448272, -0.8191520442889927978 ) ) ;
#7175 = ORIENTED_EDGE ( 'NONE', *, *, #17737, .F. ) ;
#7176 = APPROVAL_ROLE ( '' ) ;
#7178 = CARTESIAN_POINT ( 'NONE',  ( 40.88397423554524579, -6.893404915994589821, 3.998505783848317119 ) ) ;
#7177 = CC_DESIGN_APPROVAL ( #28809, ( #25875 ) ) ;
#7179 = EDGE_CURVE ( 'NONE', #17909, #29021, #27659, .T. ) ;
#7180 = CARTESIAN_POINT ( 'NONE',  ( 5.887530180601099339, 4.515817126386108882, -7.076866030741268077 ) ) ;
#7182 = FACE_OUTER_BOUND ( 'NONE', #15059, .T. ) ;
#7181 = CARTESIAN_POINT ( 'NONE',  ( 6.356382399260308347, 7.723816458760347281, 3.797266095948507836 ) ) ;
#7183 = ORIENTED_EDGE ( 'NONE', *, *, #29930, .F. ) ;
#7184 = EDGE_CURVE ( 'NONE', #26383, #31932, #22166, .T. ) ;
#7185 = CARTESIAN_POINT ( 'NONE',  ( -42.24752261775680040, -15.91354862156815031, 5.049999999999999822 ) ) ;
#7186 = CARTESIAN_POINT ( 'NONE',  ( -2.612550801365594033, -3.368539882008727115, -1.828967928396027842 ) ) ;
#7187 = CARTESIAN_POINT ( 'NONE',  ( 24.04750000136559507, -1.913930629741527500, 2.363507492473149618 ) ) ;
#7188 = CARTESIAN_POINT ( 'NONE',  ( 4.970124631802561588, -12.47916550509082612, -1.500000000000001332 ) ) ;
#7190 = ORIENTED_EDGE ( 'NONE', *, *, #22372, .T. ) ;
#7189 = CARTESIAN_POINT ( 'NONE',  ( 5.489321486716459475, 8.012877392144810429, -1.307389195612895572 ) ) ;
#7191 = AXIS2_PLACEMENT_3D ( 'NONE', #453, #15476, #10633 ) ;
#7192 = CARTESIAN_POINT ( 'NONE',  ( -2.587550801365593678, 0.3701630799359330593, -3.521866450007987037 ) ) ;
#7193 = DIRECTION ( 'NONE',  ( 0.000000000000000000, 0.000000000000000000, 1.000000000000000000 ) ) ;
#7194 = DIRECTION ( 'NONE',  ( -1.000000000000000000, -0.000000000000000000, -0.000000000000000000 ) ) ;
#7195 = FACE_OUTER_BOUND ( 'NONE', #1643, .T. ) ;
#7196 = ORIENTED_EDGE ( 'NONE', *, *, #130, .F. ) ;
#7198 = ORIENTED_EDGE ( 'NONE', *, *, #16741, .F. ) ;
#7197 = CARTESIAN_POINT ( 'NONE',  ( 0.7212197813471269425, 3.259817272365183705, -8.337493976377229998 ) ) ;
#7199 = CARTESIAN_POINT ( 'NONE',  ( 10.07348277749544074, 2.217756237939506381, 1.500000000000000000 ) ) ;
#7200 = DIRECTION ( 'NONE',  ( -1.000000000000000000, -0.000000000000000000, -0.000000000000000000 ) ) ;
#7201 = CARTESIAN_POINT ( 'NONE',  ( -19.46330280939116619, 17.00757181511099603, 1.808020238517410672 ) ) ;
#7202 = EDGE_CURVE ( 'NONE', #23972, #18705, #28891, .T. ) ;
#7203 = CARTESIAN_POINT ( 'NONE',  ( -23.54713438637982748, 4.195786794269684705, 1.499999999999999112 ) ) ;
#7204 = CARTESIAN_POINT ( 'NONE',  ( 2.087757557787927265, -16.81476909109668938, -1.499999999999999112 ) ) ;
#7205 = CC_DESIGN_DATE_AND_TIME_ASSIGNMENT ( #3184, #997, ( #21105 ) ) ;
#7206 = CARTESIAN_POINT ( 'NONE',  ( 5.612974384376776094, 7.013635602076208286, 4.279837954023495428 ) ) ;
#7207 = CARTESIAN_POINT ( 'NONE',  ( 41.34400607036577924, -3.938209558062384374, 0.8105618912856630276 ) ) ;
#7208 = CARTESIAN_POINT ( 'NONE',  ( 29.25343337322282622, -7.426690278353109242, 4.522129901861162260 ) ) ;
#7209 = ORIENTED_EDGE ( 'NONE', *, *, #4260, .T. ) ;
#7210 = DIRECTION ( 'NONE',  ( -0.9816271834476628655, 0.000000000000000000, 0.1908089953765502444 ) ) ;
#7211 = ORIENTED_EDGE ( 'NONE', *, *, #6240, .F. ) ;
#7212 = AXIS2_PLACEMENT_3D ( 'NONE', #9512, #7200, #19728 ) ;
#7213 = DIRECTION ( 'NONE',  ( 0.000000000000000000, 1.000000000000000000, 0.000000000000000000 ) ) ;
#7214 = CARTESIAN_POINT ( 'NONE',  ( -23.33713438637985860, 7.058241526941188226, 11.61334752734206255 ) ) ;
#7215 = DIRECTION ( 'NONE',  ( -1.000000000000000000, 0.000000000000000000, -0.000000000000000000 ) ) ;
#7216 = EDGE_LOOP ( 'NONE', ( #28250, #1829, #13328, #14731 ) ) ;
#7217 = ADVANCED_FACE ( 'NONE', ( #9280 ), #17313, .T. ) ;
#7218 = CARTESIAN_POINT ( 'NONE',  ( 108.0972248732595631, 18.71954638228143253, -5.110367419609437967 ) ) ;
#7219 = VERTEX_POINT ( 'NONE', #32208 ) ;
#7220 = CARTESIAN_POINT ( 'NONE',  ( -3.958196854299239160E-16, -4.616489984850518091, -1.946309384392639119 ) ) ;
#7221 = EDGE_CURVE ( 'NONE', #23082, #30095, #8603, .T. ) ;
#7223 = ORIENTED_EDGE ( 'NONE', *, *, #5321, .T. ) ;
#7222 = CARTESIAN_POINT ( 'NONE',  ( 18.86011488185538454, -4.740857608533977086, -4.001040682675098381 ) ) ;
#7224 = VERTEX_POINT ( 'NONE', #32698 ) ;
#7225 = DIRECTION ( 'NONE',  ( -0.000000000000000000, 0.000000000000000000, 1.000000000000000000 ) ) ;
#7226 = CARTESIAN_POINT ( 'NONE',  ( 47.98568197278774505, -2.821418575600922019, 0.07017451552782173751 ) ) ;
#7228 = ORIENTED_EDGE ( 'NONE', *, *, #14811, .F. ) ;
#7227 = CARTESIAN_POINT ( 'NONE',  ( 0.000000000000000000, -8.475820894092944258, -4.057423117305486215 ) ) ;
#7229 = CARTESIAN_POINT ( 'NONE',  ( 7.064423659272771161, 4.973063321325294162, 7.199384779417516533 ) ) ;
#7230 = DIRECTION ( 'NONE',  ( 1.000000000000000000, -0.000000000000000000, -0.000000000000000000 ) ) ;
#7231 = CARTESIAN_POINT ( 'NONE',  ( -4.075891499408641642E-16, -4.753758587302147731, 0.000000000000000000 ) ) ;
#7232 = CARTESIAN_POINT ( 'NONE',  ( 7.249760686538667009, 0.000000000000000000, 0.000000000000000000 ) ) ;
#7234 = EDGE_LOOP ( 'NONE', ( #24876, #16215, #10616, #6588 ) ) ;
#7233 = CARTESIAN_POINT ( 'NONE',  ( 108.0225149428689377, -18.39357169291826466, -4.507139740279709095 ) ) ;
#7235 = DIRECTION ( 'NONE',  ( -1.000000000000000000, 0.000000000000000000, 0.000000000000000000 ) ) ;
#7236 = CARTESIAN_POINT ( 'NONE',  ( 6.883866557622098092, -2.328663417917384848, -8.415306967752700373 ) ) ;
#7237 = CARTESIAN_POINT ( 'NONE',  ( 23.23500000136559862, -1.570731468192933633, -2.892927487894330074 ) ) ;
#7238 = CARTESIAN_POINT ( 'NONE',  ( 108.3798353887421655, 20.29323324528482431, -1.257911982557052832 ) ) ;
#7239 = CARTESIAN_POINT ( 'NONE',  ( 0.000000000000000000, 0.000000000000000000, 0.000000000000000000 ) ) ;
#7240 = DIRECTION ( 'NONE',  ( 0.000000000000000000, 1.000000000000000000, 0.000000000000000000 ) ) ;
#7241 = VERTEX_POINT ( 'NONE', #19498 ) ;
#7242 = FACE_OUTER_BOUND ( 'NONE', #2102, .T. ) ;
#7243 = FACE_OUTER_BOUND ( 'NONE', #2144, .T. ) ;
#7244 = CARTESIAN_POINT ( 'NONE',  ( -7.287550801365593856, 2.752080473201636845, -2.228590825266444142 ) ) ;
#7245 = VERTEX_POINT ( 'NONE', #24828 ) ;
#7246 =( BOUNDED_SURFACE ( )  B_SPLINE_SURFACE ( 3, 2, ( 
 ( #12242, #32179, #24611 ),
 ( #9916, #19972, #25115 ),
 ( #1563, #6744, #14759 ),
 ( #16935, #6896, #9563 ),
 ( #27130, #24956, #22139 ),
 ( #4231, #1923, #9748 ),
 ( #14401, #7397, #30175 ),
 ( #32349, #7248, #17439 ),
 ( #9412, #4906, #12421 ),
 ( #30326, #29820, #17090 ) ),
 .UNSPECIFIED., .F., .F., .F. ) 
 B_SPLINE_SURFACE_WITH_KNOTS ( ( 4, 2, 2, 2, 4 ),
 ( 3, 3 ),
 ( 0.003636727685402253371, 0.004103800047000620739, 0.004570872408598988107, 0.005037944770197356342, 0.005505017131795723710 ),
 ( 0.000000000000000000, 1.000000000000000000 ),
 .UNSPECIFIED. ) 
 GEOMETRIC_REPRESENTATION_ITEM ( )  RATIONAL_B_SPLINE_SURFACE ( (
 ( 1.000000000000000000, 0.8449619147701442623, 1.000000000000000000),
 ( 1.000000000000000000, 0.8255905392900951822, 1.000000000000000000),
 ( 1.000000000000000000, 0.8027571906105874788, 1.000000000000000000),
 ( 1.000000000000000000, 0.7529839109803941888, 1.000000000000000000),
 ( 1.000000000000000000, 0.7260803501548076522, 1.000000000000000000),
 ( 1.000000000000000000, 0.6677408092241539084, 1.000000000000000000),
 ( 1.000000000000000000, 0.6373774895459817236, 1.000000000000000000),
 ( 1.000000000000000000, 0.5732936775528050255, 1.000000000000000000),
 ( 1.000000000000000000, 0.5402556527143969056, 1.000000000000000000),
 ( 1.000000000000000000, 0.5090209295198725448, 1.000000000000000000) ) ) 
 REPRESENTATION_ITEM ( '' )  SURFACE ( )  );
#7247 = DIRECTION ( 'NONE',  ( 0.4999999999999978351, 0.8660254037844399289, 0.000000000000000000 ) ) ;
#7248 = CARTESIAN_POINT ( 'NONE',  ( 3.066081126419267111, 0.08824576070990676480, -0.7648597189984557287 ) ) ;
#7249 = ORIENTED_EDGE ( 'NONE', *, *, #31592, .T. ) ;
#7250 = CARTESIAN_POINT ( 'NONE',  ( 1.206392348548081639, -3.371890407423572267, -1.499999999999999334 ) ) ;
#7251 = EDGE_CURVE ( 'NONE', #16750, #16397, #16833, .T. ) ;
#7252 = ORIENTED_EDGE ( 'NONE', *, *, #1132, .T. ) ;
#7253 = ADVANCED_FACE ( 'NONE', ( #14436 ), #9778, .F. ) ;
#7254 = ORIENTED_EDGE ( 'NONE', *, *, #23933, .F. ) ;
#7255 = DIRECTION ( 'NONE',  ( 0.000000000000000000, 0.000000000000000000, 1.000000000000000000 ) ) ;
#7257 = VERTEX_POINT ( 'NONE', #6616 ) ;
#7256 = DIRECTION ( 'NONE',  ( 1.000000000000000000, 0.000000000000000000, 0.000000000000000000 ) ) ;
#7258 = VERTEX_POINT ( 'NONE', #2268 ) ;
#7259 = CARTESIAN_POINT ( 'NONE',  ( 22.92250000136559862, -1.913930629741527500, 2.363507492473149618 ) ) ;
#7260 = ORIENTED_EDGE ( 'NONE', *, *, #20402, .T. ) ;
#7261 = CARTESIAN_POINT ( 'NONE',  ( 108.1296380701674593, -19.93611807713620010, -1.386936492580776559 ) ) ;
#7263 = EDGE_LOOP ( 'NONE', ( #29765, #16999, #24033, #32810 ) ) ;
#7262 = DIRECTION ( 'NONE',  ( 0.000000000000000000, 0.9945218953682729568, 0.1045284632676570374 ) ) ;
#7264 = LINE ( 'NONE', #32368, #28807 ) ;
#7265 = CARTESIAN_POINT ( 'NONE',  ( 2.274274201625317016, -1.975651141462152482, -10.82112760146740982 ) ) ;
#7266 = DIRECTION ( 'NONE',  ( -1.000000000000000000, 0.000000000000000000, 0.000000000000000000 ) ) ;
#7267 = CARTESIAN_POINT ( 'NONE',  ( 5.377543748152548986, 8.014274990069656823, -8.669741416787380218E-17 ) ) ;
#7268 = CARTESIAN_POINT ( 'NONE',  ( 56.97280603064898941, -277.2763395528616002, -2.334455007174276009 ) ) ;
#7269 = CARTESIAN_POINT ( 'NONE',  ( 24.76851591958510213, -17.41692718791932748, 1.262548836151062615 ) ) ;
#7270 = DIRECTION ( 'NONE',  ( -0.000000000000000000, -0.000000000000000000, -1.000000000000000000 ) ) ;
#7271 = CARTESIAN_POINT ( 'NONE',  ( -1.033057378353323452, -8.048844657540879410, 4.522129901861156931 ) ) ;
#7272 = CARTESIAN_POINT ( 'NONE',  ( 0.1255855353822278031, 9.314797388872380068, 5.239665997526921970 ) ) ;
#7273 = CARTESIAN_POINT ( 'NONE',  ( -12.44989959798873791, 0.5000000000000000000, -2.482234843104710986 ) ) ;
#7274 = DIRECTION ( 'NONE',  ( -1.000000000000000000, -0.000000000000000000, 0.000000000000000000 ) ) ;
#7275 = CARTESIAN_POINT ( 'NONE',  ( -2.200050802731187360, -0.9222479816126459840, -3.113457007523259268 ) ) ;
#7276 = EDGE_LOOP ( 'NONE', ( #10836, #31248, #17836, #11711 ) ) ;
#7277 = CARTESIAN_POINT ( 'NONE',  ( -8.037550801365592079, 3.675193018007247403, -1.088641768524161391 ) ) ;
#7278 = EDGE_CURVE ( 'NONE', #23785, #20668, #13381, .T. ) ;
#7279 = DIRECTION ( 'NONE',  ( 0.7071067811865449082, 0.000000000000000000, -0.7071067811865501263 ) ) ;
#7280 = CARTESIAN_POINT ( 'NONE',  ( 3.063284526839887167, 0.000000000000000000, 8.749000000000002331 ) ) ;
#7281 = VERTEX_POINT ( 'NONE', #6924 ) ;
#7282 = CARTESIAN_POINT ( 'NONE',  ( -61.78000000000001535, -10.96999999999998820, 1.500000000000000000 ) ) ;
#7283 = DIRECTION ( 'NONE',  ( 0.000000000000000000, 0.000000000000000000, -1.000000000000000000 ) ) ;
#7284 = ORIENTED_EDGE ( 'NONE', *, *, #11546, .T. ) ;
#7285 = DIRECTION ( 'NONE',  ( 1.000000000000000000, 0.000000000000000000, 0.000000000000000000 ) ) ;
#7286 = CALENDAR_DATE ( 2026, 6, 10 ) ;
#7288 = EDGE_CURVE ( 'NONE', #13848, #5480, #17124, .T. ) ;
#7287 = CARTESIAN_POINT ( 'NONE',  ( -2.600000000000000089, 0.000000000000000000, -1.499999999999999556 ) ) ;
#7289 = ORIENTED_EDGE ( 'NONE', *, *, #12921, .F. ) ;
#7290 = LINE ( 'NONE', #2111, #24617 ) ;
#7291 = ORIENTED_EDGE ( 'NONE', *, *, #12199, .T. ) ;
#7292 = FACE_OUTER_BOUND ( 'NONE', #18594, .T. ) ;
#7293 = CARTESIAN_POINT ( 'NONE',  ( 28.67557137524228850, -6.315853537160169395, -4.312042181587000478 ) ) ;
#7294 = LINE ( 'NONE', #17485, #7515 ) ;
#7295 = PLANE ( 'NONE',  #1108 ) ;
#7296 = LINE ( 'NONE', #5251, #24153 ) ;
#7297 = EDGE_CURVE ( 'NONE', #2621, #21989, #6443, .T. ) ;
#7298 = CARTESIAN_POINT ( 'NONE',  ( 21.57350866840246439, -21.75854512865358714, -1.480343326970304130 ) ) ;
#7299 = CARTESIAN_POINT ( 'NONE',  ( -50.60000000000000142, -10.96966150227468972, 1.000000000000000000 ) ) ;
#7301 = VERTEX_POINT ( 'NONE', #32870 ) ;
#7300 = DIRECTION ( 'NONE',  ( -1.000000000000000000, -0.000000000000000000, -0.000000000000000000 ) ) ;
#7302 = CARTESIAN_POINT ( 'NONE',  ( 21.36000000273118715, 1.942864903642424146, 1.573300977624592534 ) ) ;
#7303 = CARTESIAN_POINT ( 'NONE',  ( 18.65791233782715963, -7.001076235476726417, 2.184956778830005497 ) ) ;
#7304 = ADVANCED_FACE ( 'NONE', ( #30023 ), #26231, .F. ) ;
#7305 = CARTESIAN_POINT ( 'NONE',  ( 0.000000000000000000, -1.699438267350438014, 9.241976615262153416 ) ) ;
#7306 = CARTESIAN_POINT ( 'NONE',  ( 101.6768137521178943, -2.244682085303995045, -2.942177603107532402 ) ) ;
#7307 = CARTESIAN_POINT ( 'NONE',  ( 6.356381451270081584, 0.5733789922931242788, 8.587653982362816407 ) ) ;
#7308 = CARTESIAN_POINT ( 'NONE',  ( 0.7632845268398871230, 3.174628368996073924, 8.152713396088772768 ) ) ;
#7309 = CARTESIAN_POINT ( 'NONE',  ( -56.77769102277633095, 0.5030464795276023970, -1.499999999999993117 ) ) ;
#7310 = CARTESIAN_POINT ( 'NONE',  ( 22.98163386837131839, -21.92547295135293695, 1.118948288781482558 ) ) ;
#7311 = B_SPLINE_CURVE_WITH_KNOTS ( 'NONE', 3,
 ( #3715, #13393, #18759, #21758 ),
 .UNSPECIFIED., .F., .F.,
 ( 4, 4 ),
 ( 0.000000000000000000, 0.0001149031832736470529 ),
 .UNSPECIFIED. ) ;
#7312 = ORIENTED_EDGE ( 'NONE', *, *, #23281, .T. ) ;
#7313 = EDGE_CURVE ( 'NONE', #16210, #24347, #12270, .T. ) ;
#7314 = CARTESIAN_POINT ( 'NONE',  ( -5.662550801365592967, 0.3701630799359330593, -3.521866450007987037 ) ) ;
#7315 = ORIENTED_EDGE ( 'NONE', *, *, #22254, .T. ) ;
#7316 = CARTESIAN_POINT ( 'NONE',  ( -7.954531657079159324, -3.105402419394638791, 0.9198621039125867149 ) ) ;
#7317 = CARTESIAN_POINT ( 'NONE',  ( 109.1472041058641196, 18.90877050785844204, 4.999054092451761022 ) ) ;
#7318 = CARTESIAN_POINT ( 'NONE',  ( 108.0381133239749687, 18.39038995157331158, 4.615673165465349115 ) ) ;
#7319 = ADVANCED_FACE ( 'NONE', ( #4762 ), #25147, .T. ) ;
#7320 = CARTESIAN_POINT ( 'NONE',  ( 3.707192301029357484, -12.18036120888841722, 1.758115348676513534 ) ) ;
#7321 = DIRECTION ( 'NONE',  ( 0.000000000000000000, 0.000000000000000000, 1.000000000000000000 ) ) ;
#7322 = ORIENTED_EDGE ( 'NONE', *, *, #20839, .F. ) ;
#7323 = FACE_OUTER_BOUND ( 'NONE', #12666, .T. ) ;
#7324 = EDGE_CURVE ( 'NONE', #10078, #30308, #2309, .T. ) ;
#7325 = VERTEX_POINT ( 'NONE', #2445 ) ;
#7326 = CARTESIAN_POINT ( 'NONE',  ( 3.063284526843530919, -7.360373001715506014, -4.729683950890343880 ) ) ;
#7327 = SECURITY_CLASSIFICATION_LEVEL ( 'unclassified' ) ;
#7328 = CARTESIAN_POINT ( 'NONE',  ( 28.66418304177962284, -6.762113744407424853, 3.998506281448072741 ) ) ;
#7329 = DIRECTION ( 'NONE',  ( 1.000000000000000000, -0.000000000000000000, 0.000000000000000000 ) ) ;
#7331 = DIRECTION ( 'NONE',  ( -0.000000000000000000, -0.000000000000000000, -1.000000000000000000 ) ) ;
#7330 = CARTESIAN_POINT ( 'NONE',  ( 25.24521618911088794, -7.644457093038323125E-15, 2.510216189110891172 ) ) ;
#7332 = VERTEX_POINT ( 'NONE', #20494 ) ;
#7333 = CARTESIAN_POINT ( 'NONE',  ( -8.000050800000000351, -1.817871341476558600, -2.391135792897344903 ) ) ;
#7334 = DIRECTION ( 'NONE',  ( -1.000000000000000000, -0.000000000000000000, 0.000000000000000000 ) ) ;
#7335 = CARTESIAN_POINT ( 'NONE',  ( 23.98500000136559507, -0.9349337715887248157, 3.156283516753367824 ) ) ;
#7336 = EDGE_CURVE ( 'NONE', #18871, #21569, #16057, .T. ) ;
#7337 = CARTESIAN_POINT ( 'NONE',  ( 0.3600058077333471163, -8.266758618787918067, -1.772551491157698278 ) ) ;
#7339 = ORIENTED_EDGE ( 'NONE', *, *, #27309, .T. ) ;
#7338 = CARTESIAN_POINT ( 'NONE',  ( 72.52374898132006820, -19.78015497542561008, 4.522129901861157819 ) ) ;
#7340 = CARTESIAN_POINT ( 'NONE',  ( -4.037550801365593856, 3.675193018007247403, -1.088641768524161391 ) ) ;
#7341 = FACE_OUTER_BOUND ( 'NONE', #24054, .T. ) ;
#7342 = DIRECTION ( 'NONE',  ( 1.000000000000000000, 0.000000000000000000, 0.000000000000000000 ) ) ;
#7343 = CARTESIAN_POINT ( 'NONE',  ( 21.85999999999999943, 1.573300977624590313, -1.942864903642426144 ) ) ;
#7344 = ORIENTED_EDGE ( 'NONE', *, *, #9454, .F. ) ;
#7346 = ORIENTED_EDGE ( 'NONE', *, *, #11783, .F. ) ;
#7345 = CARTESIAN_POINT ( 'NONE',  ( 23.32053031413205701, -17.41627278853337657, 1.661539697405882032 ) ) ;
#7347 = CARTESIAN_POINT ( 'NONE',  ( 2.970200582150003488, 5.831559621433202167, 7.065646041994309456 ) ) ;
#7348 = CARTESIAN_POINT ( 'NONE',  ( -15.71515769256210504, -10.96966150227469505, -11.09540449768827308 ) ) ;
#7349 =( REPRESENTATION_RELATIONSHIP ('NONE','NONE', #1085, #6656 ) REPRESENTATION_RELATIONSHIP_WITH_TRANSFORMATION ( #10463 )SHAPE_REPRESENTATION_RELATIONSHIP( ) );
#7350 = ADVANCED_FACE ( 'NONE', ( #23316 ), #85, .F. ) ;
#7351 = CARTESIAN_POINT ( 'NONE',  ( 0.7632845268398871230, 0.000000000000000000, 0.000000000000000000 ) ) ;
#7352 = CARTESIAN_POINT ( 'NONE',  ( -28.75976233758147771, 6.805598625774648802, 1.499999999998557820 ) ) ;
#7353 = CARTESIAN_POINT ( 'NONE',  ( -3.674149904271398537, -10.80265656036293720, -1.500000000000000000 ) ) ;
#7354 = CARTESIAN_POINT ( 'NONE',  ( 10.00000000000000178, -1.476463073999608300, -4.787500056513382951 ) ) ;
#7355 = PRODUCT_DEFINITION_SHAPE ( 'NONE', 'NONE',  #31711 ) ;
#7356 = EDGE_CURVE ( 'NONE', #15944, #27411, #418, .T. ) ;
#7357 = LINE ( 'NONE', #22750, #15634 ) ;
#7358 = CARTESIAN_POINT ( 'NONE',  ( 2.274274201627372705, 7.593217523255878731, 7.958834565715730669 ) ) ;
#7359 = VERTEX_POINT ( 'NONE', #25837 ) ;
#7360 = DIRECTION ( 'NONE',  ( 0.000000000000000000, 0.000000000000000000, 1.000000000000000000 ) ) ;
#7361 = EDGE_CURVE ( 'NONE', #27059, #8703, #28316, .T. ) ;
#7362 = APPROVAL_STATUS ( 'not_yet_approved' ) ;
#7363 = DIRECTION ( 'NONE',  ( -0.000000000000000000, -0.000000000000000000, -1.000000000000000000 ) ) ;
#7364 = ORIENTED_EDGE ( 'NONE', *, *, #29647, .T. ) ;
#7365 = CARTESIAN_POINT ( 'NONE',  ( -2.500050800000000351, -0.3135853898029607456, 2.983565686104819648 ) ) ;
#7366 = EDGE_LOOP ( 'NONE', ( #10033, #7041, #27811, #5882 ) ) ;
#7367 = CARTESIAN_POINT ( 'NONE',  ( -17.53440904309154647, 8.148348245851819271, 2.033243229306796351 ) ) ;
#7369 = ORIENTED_EDGE ( 'NONE', *, *, #2900, .T. ) ;
#7368 = CARTESIAN_POINT ( 'NONE',  ( 18.85812681186292750, -4.763080241043835095, -4.033870043650071402 ) ) ;
#7370 = ORIENTED_EDGE ( 'NONE', *, *, #4060, .T. ) ;
#7371 = CARTESIAN_POINT ( 'NONE',  ( -7.262550801365593500, 0.3701630799359330593, -3.521866450007987037 ) ) ;
#7372 = DIRECTION ( 'NONE',  ( -1.000000000000000000, 8.574039729943022041E-17, -1.232595164407830946E-32 ) ) ;
#7373 = ADVANCED_FACE ( 'NONE', ( #31008 ), #8091, .F. ) ;
#7374 = CARTESIAN_POINT ( 'NONE',  ( 102.5305753040692736, -0.1042037546421159255, 0.07017451552782173751 ) ) ;
#7375 = APPROVAL ( #8638, 'UNSPECIFIED' ) ;
#7377 = ORIENTED_EDGE ( 'NONE', *, *, #25300, .F. ) ;
#7376 = CARTESIAN_POINT ( 'NONE',  ( 7.249760686538667009, -2.318425219014174754, -8.437262856154184476 ) ) ;
#7378 = CARTESIAN_POINT ( 'NONE',  ( 7.249760686538667009, 4.973063321323876629, 7.199384779417138169 ) ) ;
#7379 = CARTESIAN_POINT ( 'NONE',  ( -0.3880080537174205313, -2.647099810593992242, 4.522129901861156931 ) ) ;
#7380 = DIRECTION ( 'NONE',  ( 0.000000000000000000, 0.000000000000000000, -1.000000000000000000 ) ) ;
#7381 = CARTESIAN_POINT ( 'NONE',  ( 8.060276135842835643, -2.738905749622889019, -1.500000000000000888 ) ) ;
#7383 = ORIENTED_EDGE ( 'NONE', *, *, #15380, .F. ) ;
#7382 = CARTESIAN_POINT ( 'NONE',  ( 107.5622791870681993, -18.99089674742949541, -4.502190851498308888 ) ) ;
#7384 = CARTESIAN_POINT ( 'NONE',  ( 10.00000000000000178, -8.574039729943018837E-16, 0.000000000000000000 ) ) ;
#7385 = CARTESIAN_POINT ( 'NONE',  ( 24.54750000136559507, 3.024605502323846729, -0.3178988483021056854 ) ) ;
#7386 = EDGE_CURVE ( 'NONE', #32142, #4411, #7003, .T. ) ;
#7387 = LINE ( 'NONE', #2219, #1756 ) ;
#7388 = DIRECTION ( 'NONE',  ( 0.000000000000000000, 0.000000000000000000, 1.000000000000000000 ) ) ;
#7389 = DIRECTION ( 'NONE',  ( 0.9947025833170223263, 0.1027947991993880261, 0.000000000000000000 ) ) ;
#7390 = ORIENTED_EDGE ( 'NONE', *, *, #1809, .F. ) ;
#7391 = CARTESIAN_POINT ( 'NONE',  ( 6.530491712438077911, -4.859093986587904368, 7.168846788212674070 ) ) ;
#7392 = FACE_OUTER_BOUND ( 'NONE', #14086, .T. ) ;
#7393 = CARTESIAN_POINT ( 'NONE',  ( -7.987550801365593145, 3.521866450007987037, 0.3701630799359328372 ) ) ;
#7394 = EDGE_LOOP ( 'NONE', ( #19378, #9466, #28339, #27795 ) ) ;
#7395 = DIRECTION ( 'NONE',  ( 0.000000000000000000, 0.000000000000000000, -1.000000000000000000 ) ) ;
#7396 = CARTESIAN_POINT ( 'NONE',  ( 1.750000000000000000, -5.522688772756352726, -6.461416928141300531 ) ) ;
#7397 = CARTESIAN_POINT ( 'NONE',  ( 2.974466146320791093, 0.1107971263338030782, -0.9540093664866172718 ) ) ;
#7398 = VERTEX_POINT ( 'NONE', #28506 ) ;
#7399 = CARTESIAN_POINT ( 'NONE',  ( 3.063284526839887167, 0.000000000000000000, 0.000000000000000000 ) ) ;
#7400 = VERTEX_POINT ( 'NONE', #5429 ) ;
#7401 = CARTESIAN_POINT ( 'NONE',  ( 10.56183597391177464, -5.003758587302149508, 0.2499999999999991951 ) ) ;
#7402 = VERTEX_POINT ( 'NONE', #5613 ) ;
#7403 = CARTESIAN_POINT ( 'NONE',  ( -2.753702574461988295, -0.2727682784858956322, 1.454428814729294972 ) ) ;
#7404 = ORIENTED_EDGE ( 'NONE', *, *, #1191, .T. ) ;
#7405 = ORIENTED_EDGE ( 'NONE', *, *, #15000, .F. ) ;
#7406 = FACE_OUTER_BOUND ( 'NONE', #32849, .T. ) ;
#7407 = EDGE_CURVE ( 'NONE', #16905, #11786, #602, .T. ) ;
#7408 = EDGE_LOOP ( 'NONE', ( #124, #24687, #30320, #7081, #2464 ) ) ;
#7409 = CARTESIAN_POINT ( 'NONE',  ( 0.000000000000000000, -10.90201369670499609, 1.464956435139502355 ) ) ;
#7411 = ORIENTED_EDGE ( 'NONE', *, *, #31869, .F. ) ;
#7410 = DIRECTION ( 'NONE',  ( 0.4999999999999967804, 0.8660254037844405950, 0.000000000000000000 ) ) ;
#7412 = CARTESIAN_POINT ( 'NONE',  ( -5.400050800000000706, -1.887961173149512062, -2.331437884370912261 ) ) ;
#7413 = CARTESIAN_POINT ( 'NONE',  ( 3.063284526842894540, -6.772677083981750279, 5.538577986799005259 ) ) ;
#7414 = DIRECTION ( 'NONE',  ( 1.000000000000000000, 0.000000000000000000, 0.000000000000000000 ) ) ;
#7415 = FACE_OUTER_BOUND ( 'NONE', #6862, .T. ) ;
#7416 = CARTESIAN_POINT ( 'NONE',  ( 10.56870887191539587, -4.467071865485484850, 1.625881193364682620 ) ) ;
#7417 = EDGE_CURVE ( 'NONE', #448, #14334, #9111, .T. ) ;
#7418 = ADVANCED_FACE ( 'NONE', ( #17617 ), #5724, .T. ) ;
#7419 = DIRECTION ( 'NONE',  ( 8.574039729943018344E-17, 1.000000000000000000, 0.000000000000000000 ) ) ;
#7420 = CARTESIAN_POINT ( 'NONE',  ( -0.3880080537174205313, -2.647099810593992242, 4.522129901861156931 ) ) ;
#7421 = CARTESIAN_POINT ( 'NONE',  ( 5.612718383992090665, 8.123482740191969143, 1.229942497144064451 ) ) ;
#7422 = CARTESIAN_POINT ( 'NONE',  ( 107.6641948605100083, -20.45809826282308208, 1.500000000000000000 ) ) ;
#7423 = EDGE_CURVE ( 'NONE', #20990, #26613, #18099, .T. ) ;
#7424 = CARTESIAN_POINT ( 'NONE',  ( 3.499999999999999556, 2.871924938129968741, -6.435996203144479288 ) ) ;
#7425 = CARTESIAN_POINT ( 'NONE',  ( -3.050050802731187449, -1.887961173149512062, -2.331437884370912261 ) ) ;
#7426 = ORIENTED_EDGE ( 'NONE', *, *, #7179, .T. ) ;
#7427 = CARTESIAN_POINT ( 'NONE',  ( -3.850050799999999995, -2.853674364686378695, -1.549418761218566809 ) ) ;
#7428 = FACE_OUTER_BOUND ( 'NONE', #10074, .T. ) ;
#7429 = DIRECTION ( 'NONE',  ( 0.000000000000000000, 0.000000000000000000, 1.000000000000000000 ) ) ;
#7430 = ORIENTED_EDGE ( 'NONE', *, *, #15819, .T. ) ;
#7431 = CARTESIAN_POINT ( 'NONE',  ( -2.000050802731187627, 3.113457007523260156, -0.9222479816126439855 ) ) ;
#7432 = LINE ( 'NONE', #9608, #19931 ) ;
#7433 = CARTESIAN_POINT ( 'NONE',  ( 107.9814001905993734, -17.80152948830060211, 4.369786445662967367 ) ) ;
#7434 = CIRCLE ( 'NONE', #12774, 297.9387600756452912 ) ;
#7435 = ORIENTED_EDGE ( 'NONE', *, *, #6038, .F. ) ;
#7436 = CARTESIAN_POINT ( 'NONE',  ( -12.44989959798873791, 0.000000000000000000, -2.482234843104710986 ) ) ;
#7437 = APPROVAL_STATUS ( 'not_yet_approved' ) ;
#7438 = CARTESIAN_POINT ( 'NONE',  ( 3.608283490412332364E-16, 4.208382051008191738, 2.718385644597189454 ) ) ;
#7439 = ORIENTED_EDGE ( 'NONE', *, *, #28088, .T. ) ;
#7440 = CARTESIAN_POINT ( 'NONE',  ( 0.6620495146783516027, -15.34493536057754248, 1.745995208913456720 ) ) ;
#7441 = ORIENTED_EDGE ( 'NONE', *, *, #24039, .T. ) ;
#7442 = CARTESIAN_POINT ( 'NONE',  ( 24.97738509828242925, 18.93945643846228677, -1.491740999229418829 ) ) ;
#7444 = ORIENTED_EDGE ( 'NONE', *, *, #6106, .F. ) ;
#7443 = CYLINDRICAL_SURFACE ( 'NONE', #26164, 11.00000000000000000 ) ;
#7445 = CARTESIAN_POINT ( 'NONE',  ( 7.249760686538667009, 5.151476664237477188, 6.139290821770273077 ) ) ;
#7446 = CARTESIAN_POINT ( 'NONE',  ( 7.249760686538667009, -3.647351267791519636, -7.953573330858250579 ) ) ;
#7447 =( BOUNDED_CURVE ( )  B_SPLINE_CURVE ( 2, ( #11960, #27319, #21971 ),
 .UNSPECIFIED., .F., .F. ) 
 B_SPLINE_CURVE_WITH_KNOTS ( ( 3, 3 ),
 ( 0.9353822619934377691, 0.9375000000000000000 ),
 .UNSPECIFIED. ) 
 CURVE ( )  GEOMETRIC_REPRESENTATION_ITEM ( )  RATIONAL_B_SPLINE_CURVE ( ( 0.9821626249036861100, 0.9896829947469995004, 1.000000000000000000 ) ) 
 REPRESENTATION_ITEM ( '' )  );
#7448 = CARTESIAN_POINT ( 'NONE',  ( 21.36097421961356702, -21.76718868951428121, -1.410897148389125277 ) ) ;
#7449 = DIRECTION ( 'NONE',  ( -1.000000000000000000, -0.000000000000000000, -0.000000000000000000 ) ) ;
#7450 = EDGE_CURVE ( 'NONE', #19201, #2610, #9675, .T. ) ;
#7451 = ORIENTED_EDGE ( 'NONE', *, *, #9113, .T. ) ;
#7452 = FACE_BOUND ( 'NONE', #33006, .T. ) ;
#7453 = DIRECTION ( 'NONE',  ( 0.000000000000000000, 0.000000000000000000, -1.000000000000000000 ) ) ;
#7454 = CARTESIAN_POINT ( 'NONE',  ( 7.577572045913244736, 15.00000000000000178, 4.629213727441584325 ) ) ;
#7455 = DIRECTION ( 'NONE',  ( 0.000000000000000000, -0.000000000000000000, 1.000000000000000000 ) ) ;
#7456 = CIRCLE ( 'NONE', #18657, 5.009999999999999787 ) ;
#7457 = B_SPLINE_CURVE_WITH_KNOTS ( 'NONE', 3,
 ( #17349, #26883, #24360, #1632, #9470, #1476, #16843, #11821, #9315, #2126, #6962, #27040, #12307, #19530, #24862, #11652 ),
 .UNSPECIFIED., .F., .F.,
 ( 4, 2, 2, 2, 2, 2, 2, 4 ),
 ( 0.01324599089037892946, 0.5000000000000001110, 0.6250000000000000000, 0.7500000000000000000, 0.8125000000000000000, 0.8750000000000000000, 0.9375000000000000000, 1.000000000000000000 ),
 .UNSPECIFIED. ) ;
#7458 = CARTESIAN_POINT ( 'NONE',  ( 5.377543748152548098, -2.789499415801756586E-14, 8.014274990069656823 ) ) ;
#7459 = CARTESIAN_POINT ( 'NONE',  ( 23.71271855738292800, -17.43088677775545392, -1.604577790254563485 ) ) ;
#7460 = CARTESIAN_POINT ( 'NONE',  ( -56.36676944933713429, 0.006999862979873096649, -1.006932307331389609 ) ) ;
#7462 = CARTESIAN_POINT ( 'NONE',  ( 22.68241379554079629, -21.87740465772228049, 1.258814731509616758 ) ) ;
#7461 = DESIGN_CONTEXT ( 'detailed design', #29135, 'design' ) ;
#7463 = ORIENTED_EDGE ( 'NONE', *, *, #31794, .T. ) ;
#7464 = CARTESIAN_POINT ( 'NONE',  ( -7.812550801365593323, 3.368539882008727115, 1.828967928396026954 ) ) ;
#7465 = EDGE_LOOP ( 'NONE', ( #13176, #16599, #25351 ) ) ;
#7466 = CARTESIAN_POINT ( 'NONE',  ( -5.704531657079157547, -0.3127741368606806738, 2.975847129947406522 ) ) ;
#7467 = CIRCLE ( 'NONE', #11739, 8.750000000000000000 ) ;
#7468 = CARTESIAN_POINT ( 'NONE',  ( 23.79750000136559507, 2.363507492473148286, 1.913930629741525058 ) ) ;
#7469 = CARTESIAN_POINT ( 'NONE',  ( 108.0821972398986617, -20.20655521172211166, 1.448620529800545897 ) ) ;
#7470 = DIRECTION ( 'NONE',  ( -1.000000000000000000, -0.000000000000000000, -0.000000000000000000 ) ) ;
#7471 = DIRECTION ( 'NONE',  ( 0.000000000000000000, 0.000000000000000000, 1.000000000000000000 ) ) ;
#7472 = VERTEX_POINT ( 'NONE', #3735 ) ;
#7473 = CARTESIAN_POINT ( 'NONE',  ( 7.249760686538667009, 8.711672189281426171, 0.8180878109962165246 ) ) ;
#7474 = CARTESIAN_POINT ( 'NONE',  ( 85.20563808598696198, -3.194259795296082061, -4.522129901861162260 ) ) ;
#7475 = ORIENTED_EDGE ( 'NONE', *, *, #15715, .T. ) ;
#7476 = CARTESIAN_POINT ( 'NONE',  ( 7.064423669210280643, -5.064320921489739113, 7.135485519863445703 ) ) ;
#7477 = COORDINATED_UNIVERSAL_TIME_OFFSET ( 0, 0, .AHEAD. ) ;
#7478 = CIRCLE ( 'NONE', #14966, 2.999999999999998224 ) ;
#7479 = CARTESIAN_POINT ( 'NONE',  ( 40.88392054027885791, -6.883494307245545230, 4.013697493832091290 ) ) ;
#7480 = EDGE_CURVE ( 'NONE', #22295, #6678, #13410, .T. ) ;
#7481 = AXIS2_PLACEMENT_3D ( 'NONE', #8178, #5670, #25909 ) ;
#7482 = CARTESIAN_POINT ( 'NONE',  ( 4.749760686538667009, 5.151476664237558900, -6.139290821770204687 ) ) ;
#7483 = AXIS2_PLACEMENT_3D ( 'NONE', #7227, #22769, #19943 ) ;
#7485 = DIRECTION ( 'NONE',  ( -1.000000000000000000, -0.000000000000000000, -0.000000000000000000 ) ) ;
#7484 = CARTESIAN_POINT ( 'NONE',  ( 7.249760686538667009, 7.906491560603665647, 3.748318449932320107 ) ) ;
#7486 = EDGE_CURVE ( 'NONE', #23391, #30204, #20976, .T. ) ;
#7487 = B_SPLINE_CURVE_WITH_KNOTS ( 'NONE', 3,
 ( #22385, #14032, #1361, #11536, #21731, #18041, #23051, #10012, #30269, #20389, #30116, #25405, #17385 ),
 .UNSPECIFIED., .F., .F.,
 ( 4, 3, 3, 3, 4 ),
 ( 1.301042606982605321E-18, 0.0006642486831287936454, 0.001556668540121195800, 0.002449088397071176593, 0.003341508253979123301 ),
 .UNSPECIFIED. ) ;
#7488 = VERTEX_POINT ( 'NONE', #5902 ) ;
#7489 = CARTESIAN_POINT ( 'NONE',  ( -8.000050800000000351, -2.570627647327130116, -1.572659124966501620 ) ) ;
#7490 = DIRECTION ( 'NONE',  ( 8.574039729943018344E-17, 1.000000000000000000, 0.000000000000000000 ) ) ;
#7491 = CARTESIAN_POINT ( 'NONE',  ( 22.48500000136559507, 0.9349337715887185984, -3.156283516753368268 ) ) ;
#7492 = CARTESIAN_POINT ( 'NONE',  ( 0.000000000000000000, 0.000000000000000000, 0.000000000000000000 ) ) ;
#7493 = AXIS2_PLACEMENT_3D ( 'NONE', #25871, #21016, #10975 ) ;
#7495 = ORIENTED_EDGE ( 'NONE', *, *, #20871, .T. ) ;
#7494 = CARTESIAN_POINT ( 'NONE',  ( 107.6696042164950740, 19.18437618895796248, 4.906253902711251058 ) ) ;
#7496 = CARTESIAN_POINT ( 'NONE',  ( -7.512550801365593500, -3.675193018007246071, 1.088641768524163167 ) ) ;
#7497 = CARTESIAN_POINT ( 'NONE',  ( 2.866494652520772846, -9.241976615239517301, 2.300561732649529123 ) ) ;
#7498 = DIRECTION ( 'NONE',  ( 0.000000000000000000, 0.08715574274765452989, 0.9961946980917458783 ) ) ;
#7500 = EDGE_CURVE ( 'NONE', #31355, #27203, #11830, .T. ) ;
#7499 = CARTESIAN_POINT ( 'NONE',  ( 10.00000000000000000, -4.971152295393299170, -0.6226916219172567990 ) ) ;
#7501 = VERTEX_POINT ( 'NONE', #26146 ) ;
#7503 = ORIENTED_EDGE ( 'NONE', *, *, #9493, .T. ) ;
#7502 = CARTESIAN_POINT ( 'NONE',  ( 2.274274201625315239, -10.82112760146740449, 1.975651141462185789 ) ) ;
#7504 = EDGE_CURVE ( 'NONE', #6218, #26130, #12374, .T. ) ;
#7505 = CARTESIAN_POINT ( 'NONE',  ( 12.61464622672343516, 16.97301654637829671, -1.491740999229419273 ) ) ;
#7506 = CARTESIAN_POINT ( 'NONE',  ( 3.063284526839890276, 0.4999240074895630048, -8.734705317681616066 ) ) ;
#7507 = AXIS2_PLACEMENT_3D ( 'NONE', #12185, #16532, #4528 ) ;
#7508 = VECTOR ( 'NONE', #8691, 1000.000000000000000 ) ;
#7509 = EDGE_CURVE ( 'NONE', #33081, #16776, #11471, .T. ) ;
#7510 = CARTESIAN_POINT ( 'NONE',  ( 22.86000000136559862, 1.570731468192929858, 2.892927487894329630 ) ) ;
#7511 = VECTOR ( 'NONE', #8229, 1000.000000000000000 ) ;
#7512 = CARTESIAN_POINT ( 'NONE',  ( 84.91897426280726791, -3.309433673477568671, 2.787781823999374797 ) ) ;
#7513 = CARTESIAN_POINT ( 'NONE',  ( -2.559200518355241094, -12.25278053493027031, -1.499999999999920064 ) ) ;
#7514 = DIRECTION ( 'NONE',  ( 8.541412920197227210E-17, 0.9961946980917464334, -0.08715574274764853469 ) ) ;
#7515 = VECTOR ( 'NONE', #4971, 1000.000000000000000 ) ;
#7516 = CARTESIAN_POINT ( 'NONE',  ( 0.000000000000000000, 0.000000000000000000, 0.000000000000000000 ) ) ;
#7517 = CARTESIAN_POINT ( 'NONE',  ( 85.38119660046028514, -6.034158634444421132, 4.522129901861162260 ) ) ;
#7518 = EDGE_LOOP ( 'NONE', ( #26450, #10575, #14186, #28645 ) ) ;
#7519 = CARTESIAN_POINT ( 'NONE',  ( -23.54713438637982748, 10.61651369059875272, 9.545881648375194928 ) ) ;
#7520 = ADVANCED_FACE ( 'NONE', ( #27120 ), #6576, .F. ) ;
#7521 = VECTOR ( 'NONE', #25426, 1000.000000000000000 ) ;
#7522 = APPROVAL_DATE_TIME ( #32961, #5764 ) ;
#7523 = LINE ( 'NONE', #12702, #13897 ) ;
#7524 = VERTEX_POINT ( 'NONE', #14898 ) ;
#7525 = CARTESIAN_POINT ( 'NONE',  ( 7.249760686538667009, -7.135485519861965109, -5.064320921489893657 ) ) ;
#7526 = VERTEX_POINT ( 'NONE', #17077 ) ;
#7527 = CARTESIAN_POINT ( 'NONE',  ( -21.12071669798443452, 17.96555046547580048, 1.784921029145990046 ) ) ;
#7529 = VERTEX_POINT ( 'NONE', #19963 ) ;
#7528 = CARTESIAN_POINT ( 'NONE',  ( 102.3444260579792058, -2.861320725351368832, -4.003574673598517819 ) ) ;
#7530 = AXIS2_PLACEMENT_3D ( 'NONE', #32377, #1591, #2092 ) ;
#7531 = ORIENTED_EDGE ( 'NONE', *, *, #25545, .F. ) ;
#7532 = FACE_OUTER_BOUND ( 'NONE', #6503, .T. ) ;
#7533 = CARTESIAN_POINT ( 'NONE',  ( -6.812550801365595099, -1.828967928396026732, 3.368539882008728004 ) ) ;
#7534 = CIRCLE ( 'NONE', #8606, 10.94895958125474245 ) ;
#7535 = CARTESIAN_POINT ( 'NONE',  ( 25.75999999999999801, -2.208672634433321348E-15, -2.499999999999997780 ) ) ;
#7536 = CIRCLE ( 'NONE', #31580, 0.9999999999999991118 ) ;
#7537 = CARTESIAN_POINT ( 'NONE',  ( -7.000050800000000351, 0.000000000000000000, -6.000000000000000888 ) ) ;
#7539 = VERTEX_POINT ( 'NONE', #32493 ) ;
#7538 = CARTESIAN_POINT ( 'NONE',  ( 0.7632845268398882332, -4.729683950898921019, 7.360373001730893705 ) ) ;
#7540 = CARTESIAN_POINT ( 'NONE',  ( 0.000000000000000000, -9.314797388894881180, -1.239665997526989027 ) ) ;
#7541 = VECTOR ( 'NONE', #4294, 1000.000000000000227 ) ;
#7542 = CARTESIAN_POINT ( 'NONE',  ( 107.4500373638809947, -17.36019379023286646, 4.522129901861156931 ) ) ;
#7543 = CARTESIAN_POINT ( 'NONE',  ( 0.5106493704296974911, -15.23275403072758216, 1.745873292837237800 ) ) ;
#7544 = EDGE_CURVE ( 'NONE', #30805, #11692, #9238, .T. ) ;
#7545 = DIRECTION ( 'NONE',  ( 0.000000000000000000, 0.000000000000000000, 1.000000000000000000 ) ) ;
#7547 = ORIENTED_EDGE ( 'NONE', *, *, #28090, .T. ) ;
#7546 = DIRECTION ( 'NONE',  ( -0.000000000000000000, -1.000000000000000000, -0.000000000000000000 ) ) ;
#7548 = ADVANCED_FACE ( 'NONE', ( #9552 ), #24947, .F. ) ;
#7549 = CARTESIAN_POINT ( 'NONE',  ( 7.249760686538667009, -3.748318449932352081, 7.906491560603652324 ) ) ;
#7550 = AXIS2_PLACEMENT_3D ( 'NONE', #5414, #17785, #4920 ) ;
#7551 = CARTESIAN_POINT ( 'NONE',  ( 2.387425658415018415, 10.57543975281068249, 2.081220874697345291 ) ) ;
#7552 = DIRECTION ( 'NONE',  ( -1.000000000000000000, 0.000000000000000000, -0.000000000000000000 ) ) ;
#7553 = EDGE_CURVE ( 'NONE', #13056, #4840, #622, .T. ) ;
#7554 = DIRECTION ( 'NONE',  ( 0.000000000000000000, 0.000000000000000000, 1.000000000000000000 ) ) ;
#7555 = CARTESIAN_POINT ( 'NONE',  ( 5.612717990268488499, 8.213645783354285967, -0.1993707932846307540 ) ) ;
#7556 = DIRECTION ( 'NONE',  ( -0.000000000000000000, -0.000000000000000000, -1.000000000000000000 ) ) ;
#7557 = ORIENTED_EDGE ( 'NONE', *, *, #986, .F. ) ;
#7558 = DIRECTION ( 'NONE',  ( -0.02413862388702650921, -0.9993908270190956511, -0.02520519206291740172 ) ) ;
#7559 = AXIS2_PLACEMENT_3D ( 'NONE', #20120, #20769, #9907 ) ;
#7560 = B_SPLINE_CURVE_WITH_KNOTS ( 'NONE', 3,
 ( #8785, #3284, #18989, #11284, #5934, #16132, #21171, #8928, #29175, #31520 ),
 .UNSPECIFIED., .F., .F.,
 ( 4, 2, 2, 2, 4 ),
 ( 1.968338519002106713E-07, 0.0005467930078056959303, 0.001093389181759491522, 0.001639985355713287222, 0.002186581529667083138 ),
 .UNSPECIFIED. ) ;
#7561 = DIRECTION ( 'NONE',  ( 0.000000000000000000, 0.000000000000000000, 1.000000000000000000 ) ) ;
#7562 = CARTESIAN_POINT ( 'NONE',  ( -6.787550801365593856, -3.521866450007987037, -0.3701630799359323931 ) ) ;
#7563 = EDGE_LOOP ( 'NONE', ( #7475, #22925, #23293, #7173 ) ) ;
#7564 = CIRCLE ( 'NONE', #32691, 297.4345239564032681 ) ;
#7566 = EDGE_CURVE ( 'NONE', #23561, #27019, #4729, .T. ) ;
#7565 = VECTOR ( 'NONE', #21287, 1000.000000000000000 ) ;
#7567 = APPROVAL ( #14799, 'UNKNOWN' ) ;
#7568 = CIRCLE ( 'NONE', #31099, 5.010000000000000675 ) ;
#7569 = CARTESIAN_POINT ( 'NONE',  ( 4.013969549054193054E-16, 4.681538312723529494, -0.8254815157534771686 ) ) ;
#7570 = FACE_OUTER_BOUND ( 'NONE', #28000, .T. ) ;
#7571 = CARTESIAN_POINT ( 'NONE',  ( 6.037141752603385036, -8.462586328878536790, 0.4483113388088767470 ) ) ;
#7572 = ORIENTED_EDGE ( 'NONE', *, *, #7921, .T. ) ;
#7574 = CARTESIAN_POINT ( 'NONE',  ( 23.57316428367674277, -9.051964865549241068, -0.07017451552783579571 ) ) ;
#7573 = VECTOR ( 'NONE', #25942, 999.9999999999998863 ) ;
#7575 = ORIENTED_EDGE ( 'NONE', *, *, #23084, .T. ) ;
#7576 = VECTOR ( 'NONE', #20132, 1000.000000000000000 ) ;
#7577 = CIRCLE ( 'NONE', #30558, 5.010000000000000675 ) ;
#7578 = CARTESIAN_POINT ( 'NONE',  ( -41.04909327648282158, -14.04690330772141316, 5.700934511681481354 ) ) ;
#7579 = ORIENTED_EDGE ( 'NONE', *, *, #31759, .F. ) ;
#7580 = CARTESIAN_POINT ( 'NONE',  ( 48.08400536259535585, -8.675012021211058411, 2.713652344655544724 ) ) ;
#7582 = ORIENTED_EDGE ( 'NONE', *, *, #25393, .F. ) ;
#7581 = CARTESIAN_POINT ( 'NONE',  ( -2.971049596204458076, -0.1846667992746918174, 1.395223860601304100 ) ) ;
#7583 = ORIENTED_EDGE ( 'NONE', *, *, #26769, .T. ) ;
#7584 = CARTESIAN_POINT ( 'NONE',  ( 6.880159396099833735, -4.949130873693328603, -7.192972099401679920 ) ) ;
#7585 = ORIENTED_EDGE ( 'NONE', *, *, #491, .T. ) ;
#7586 = CARTESIAN_POINT ( 'NONE',  ( 0.1574692293610884808, 9.672096048331027873, -4.391622967208299144 ) ) ;
#7588 = ORIENTED_EDGE ( 'NONE', *, *, #7824, .T. ) ;
#7587 = DIRECTION ( 'NONE',  ( 1.000000000000000000, 0.000000000000000000, 0.000000000000000000 ) ) ;
#7589 = AXIS2_PLACEMENT_3D ( 'NONE', #7028, #19741, #29781 ) ;
#7590 = CARTESIAN_POINT ( 'NONE',  ( -56.33890164103149800, 0.003417460827233314170, -1.001984214669649820 ) ) ;
#7591 = LINE ( 'NONE', #8081, #14463 ) ;
#7592 = EDGE_CURVE ( 'NONE', #24987, #12982, #13953, .T. ) ;
#7593 = VECTOR ( 'NONE', #9355, 999.9999999999998863 ) ;
#7594 = DIRECTION ( 'NONE',  ( 1.000000000000000000, 0.000000000000000000, 0.000000000000000000 ) ) ;
#7595 = CARTESIAN_POINT ( 'NONE',  ( -0.9801757370192266672, 20.00000000000000000, 6.747923662139668544 ) ) ;
#7596 = CIRCLE ( 'NONE', #4406, 0.4499999999999999001 ) ;
#7597 = AXIS2_PLACEMENT_3D ( 'NONE', #19864, #10325, #2817 ) ;
#7598 = VECTOR ( 'NONE', #18042, 1000.000000000000000 ) ;
#7599 = DIRECTION ( 'NONE',  ( 6.938893903907222067E-15, 0.000000000000000000, 1.000000000000000000 ) ) ;
#7600 = CARTESIAN_POINT ( 'NONE',  ( 10.00000000000000178, -8.574039729943018837E-16, 0.000000000000000000 ) ) ;
#7601 = DIRECTION ( 'NONE',  ( 0.000000000000000000, 0.000000000000000000, 1.000000000000000000 ) ) ;
#7602 = VECTOR ( 'NONE', #7086, 1000.000000000000000 ) ;
#7603 = CARTESIAN_POINT ( 'NONE',  ( -2.889143798718842415, 0.000000000000000000, 0.9788672205877712029 ) ) ;
#7604 = CARTESIAN_POINT ( 'NONE',  ( -15.12340757463330654, -27.93932300454937590, -1.000000000000000000 ) ) ;
#7605 = CARTESIAN_POINT ( 'NONE',  ( 0.1921710002436126385, 9.148850822275088390, 5.239665997525987606 ) ) ;
#7606 = CARTESIAN_POINT ( 'NONE',  ( 54.64624227588102201, -3.635739347938791610, 0.07017451550800275772 ) ) ;
#7607 = CARTESIAN_POINT ( 'NONE',  ( 69.18703749905368738, -4.112663945019823686, 4.522129901861162260 ) ) ;
#7608 = CARTESIAN_POINT ( 'NONE',  ( -2.450050802731187360, -2.331437884370912705, 1.887961173149512062 ) ) ;
#7609 = ORIENTED_EDGE ( 'NONE', *, *, #19997, .F. ) ;
#7610 = CARTESIAN_POINT ( 'NONE',  ( -4.237550801365593145, -1.088641768524163389, -3.675193018007246071 ) ) ;
#7611 = EDGE_CURVE ( 'NONE', #31571, #32878, #4409, .T. ) ;
#7612 = CIRCLE ( 'NONE', #158, 4.000000000000001776 ) ;
#7613 = AXIS2_PLACEMENT_3D ( 'NONE', #20275, #30830, #2411 ) ;
#7614 = CARTESIAN_POINT ( 'NONE',  ( 9.282537329959909655, 0.2172754300399158400, -1.041239158277187160 ) ) ;
#7615 = CARTESIAN_POINT ( 'NONE',  ( 24.72695737054825926, 18.91229966141139229, 1.500000000000000000 ) ) ;
#7617 = ORIENTED_EDGE ( 'NONE', *, *, #27309, .F. ) ;
#7616 = VECTOR ( 'NONE', #4407, 1000.000000000000000 ) ;
#7618 = CYLINDRICAL_SURFACE ( 'NONE', #28822, 6.248999999999999666 ) ;
#7619 = DIRECTION ( 'NONE',  ( 0.000000000000000000, 0.000000000000000000, 1.000000000000000000 ) ) ;
#7620 = AXIS2_PLACEMENT_3D ( 'NONE', #18738, #28941, #16242 ) ;
#7621 = AXIS2_PLACEMENT_3D ( 'NONE', #3586, #8758, #6739 ) ;
#7622 = ORIENTED_EDGE ( 'NONE', *, *, #22115, .T. ) ;
#7623 = DIRECTION ( 'NONE',  ( 0.06927878976713819359, -0.9975973382524637723, 0.000000000000000000 ) ) ;
#7624 = APPROVAL_STATUS ( 'not_yet_approved' ) ;
#7625 = AXIS2_PLACEMENT_3D ( 'NONE', #5561, #28, #17746 ) ;
#7627 = ORIENTED_EDGE ( 'NONE', *, *, #12144, .F. ) ;
#7626 = LINE ( 'NONE', #15302, #22934 ) ;
#7628 = ORIENTED_EDGE ( 'NONE', *, *, #14685, .F. ) ;
#7629 = DIRECTION ( 'NONE',  ( 0.000000000000000000, 0.9848077530122081313, 0.1736481776669305255 ) ) ;
#7630 =( GEOMETRIC_REPRESENTATION_CONTEXT ( 3 ) GLOBAL_UNCERTAINTY_ASSIGNED_CONTEXT ( ( #4801 ) ) GLOBAL_UNIT_ASSIGNED_CONTEXT ( ( #20670, #25662, #15640 ) ) REPRESENTATION_CONTEXT ( 'NONE', 'WORKASPACE' ) );
#7631 = ADVANCED_FACE ( 'NONE', ( #6886 ), #14591, .T. ) ;
#7632 = VERTEX_POINT ( 'NONE', #19462 ) ;
#7633 = CARTESIAN_POINT ( 'NONE',  ( 25.75999999999999801, 0.8512451026088739825, 2.902758476911987628 ) ) ;
#7635 = ORIENTED_EDGE ( 'NONE', *, *, #31428, .F. ) ;
#7634 = CARTESIAN_POINT ( 'NONE',  ( 3.499999999999999556, 0.000000000000000000, 0.000000000000000000 ) ) ;
#7636 = CARTESIAN_POINT ( 'NONE',  ( 17.44299375779232264, 12.90469621563894798, 1.049999999999999378 ) ) ;
#7637 = FACE_OUTER_BOUND ( 'NONE', #31058, .T. ) ;
#7638 = EDGE_CURVE ( 'NONE', #21332, #9995, #14391, .T. ) ;
#7639 = CARTESIAN_POINT ( 'NONE',  ( 21.49636748197312386, -21.75484023020513646, -1.469027763226378847 ) ) ;
#7640 = LINE ( 'NONE', #7150, #29526 ) ;
#7641 = VECTOR ( 'NONE', #29249, 1000.000000000000000 ) ;
#7642 = ORIENTED_EDGE ( 'NONE', *, *, #6001, .T. ) ;
#7643 = VECTOR ( 'NONE', #30739, 1000.000000000000000 ) ;
#7644 = VECTOR ( 'NONE', #27053, 1000.000000000000227 ) ;
#7645 = DIRECTION ( 'NONE',  ( 1.000000000000000000, 0.000000000000000000, 0.000000000000000000 ) ) ;
#7646 = CARTESIAN_POINT ( 'NONE',  ( -31.85664627820676387, -0.0003384977252905707612, 1.731076043996917724 ) ) ;
#7647 = DIRECTION ( 'NONE',  ( 0.000000000000000000, 1.000000000000000000, 0.000000000000000000 ) ) ;
#7648 = CARTESIAN_POINT ( 'NONE',  ( 23.90742340928847653, -3.204431202321702088, -2.713652344655540727 ) ) ;
#7649 = CIRCLE ( 'NONE', #19922, 4.999999999999997335 ) ;
#7650 = VECTOR ( 'NONE', #22214, 1000.000000000000000 ) ;
#7651 = CIRCLE ( 'NONE', #30632, 0.5000000000000000000 ) ;
#7652 = CARTESIAN_POINT ( 'NONE',  ( 24.39739546318580565, -17.41185525199284001, 1.419135974561906099 ) ) ;
#7653 = CARTESIAN_POINT ( 'NONE',  ( 0.6728000631899144768, -0.5626559339043585295, 9.133409206477402620 ) ) ;
#7654 = CARTESIAN_POINT ( 'NONE',  ( -56.77769102277633806, 0.5030464795276025081, -1.050000000000000044 ) ) ;
#7655 = CARTESIAN_POINT ( 'NONE',  ( 22.90158751868941778, -21.92087667321492006, 1.135468510342883652 ) ) ;
#7656 = VERTEX_POINT ( 'NONE', #24600 ) ;
#7657 = CC_DESIGN_APPROVAL ( #12272, ( #17797 ) ) ;
#7658 = CARTESIAN_POINT ( 'NONE',  ( -6.262550801365593500, 3.521866450007987037, 0.3701630799359328372 ) ) ;
#7659 = ORIENTED_EDGE ( 'NONE', *, *, #18586, .T. ) ;
#7660 = CARTESIAN_POINT ( 'NONE',  ( -2.604531657079157903, 1.883076972206379374, 2.325406398514293205 ) ) ;
#7661 = CARTESIAN_POINT ( 'NONE',  ( 23.54750000136559862, 1.913930629741522838, -2.363507492473150062 ) ) ;
#7662 = CARTESIAN_POINT ( 'NONE',  ( 4.749760686538667009, -8.014274990069656823, 8.669741416787380218E-17 ) ) ;
#7663 = CARTESIAN_POINT ( 'NONE',  ( 1.055238632343717731, -2.663178554379440399, 1.761001113085417957 ) ) ;
#7664 = DIRECTION ( 'NONE',  ( -0.000000000000000000, -0.000000000000000000, -1.000000000000000000 ) ) ;
#7665 = ORIENTED_EDGE ( 'NONE', *, *, #15349, .T. ) ;
#7666 = LINE ( 'NONE', #30584, #26828 ) ;
#7667 =( BOUNDED_CURVE ( )  B_SPLINE_CURVE ( 2, ( #11309, #13305, #5800, #15978, #23993, #20852, #13481, #3146, #31729, #8464, #21517 ),
 .UNSPECIFIED., .F., .F. ) 
 B_SPLINE_CURVE_WITH_KNOTS ( ( 3, 2, 2, 2, 2, 3 ),
 ( 0.4978822619934377136, 0.5000000000000000000, 0.5156250000000000000, 0.5312500000000000000, 0.5468750000000000000, 0.5603822619934377691 ),
 .UNSPECIFIED. ) 
 CURVE ( )  GEOMETRIC_REPRESENTATION_ITEM ( )  RATIONAL_B_SPLINE_CURVE ( ( 0.9821626249036857770, 0.9896829947469991673, 1.000000000000000000, 0.9238795325112867385, 1.000000000000000000, 0.9238795325112867385, 1.000000000000000000, 0.9238795325112867385, 1.000000000000000000, 0.9341965377642872381, 0.9821626249036861100 ) ) 
 REPRESENTATION_ITEM ( '' )  );
#7668 = DIRECTION ( 'NONE',  ( -0.1413077769430314268, 0.9899657126261587337, 0.000000000000000000 ) ) ;
#7669 = ORIENTED_EDGE ( 'NONE', *, *, #26525, .F. ) ;
#7670 = LINE ( 'NONE', #17870, #4912 ) ;
#7671 = APPLICATION_PROTOCOL_DEFINITION ( 'international standard', 'config_control_design', 1994, #9686 ) ;
#7672 = CARTESIAN_POINT ( 'NONE',  ( 28.66498257487024048, -6.730694557050681759, 4.043900693851640860 ) ) ;
#7673 = AXIS2_PLACEMENT_3D ( 'NONE', #3921, #19618, #31990 ) ;
#7674 = EDGE_CURVE ( 'NONE', #4392, #10617, #13800, .T. ) ;
#7676 = EDGE_CURVE ( 'NONE', #29447, #16073, #9993, .T. ) ;
#7675 = VECTOR ( 'NONE', #32758, 1000.000000000000000 ) ;
#7677 = CARTESIAN_POINT ( 'NONE',  ( -29.24402871571405882, 0.000000000000000000, 11.00000000000000000 ) ) ;
#7679 = DIRECTION ( 'NONE',  ( -2.219124775574928185E-17, -0.2588190451025209060, -0.9659258262890682012 ) ) ;
#7678 = CARTESIAN_POINT ( 'NONE',  ( 25.23836956833649836, 0.1740941550253437553, 2.498860794741531777 ) ) ;
#7680 = ORIENTED_EDGE ( 'NONE', *, *, #11185, .T. ) ;
#7681 = LOCAL_TIME ( 16, 7, 10.00000000000000000, #31395 ) ;
#7682 = CARTESIAN_POINT ( 'NONE',  ( -8.000050800000000351, -0.5569032332065858570, -2.961701699052899261 ) ) ;
#7683 = CARTESIAN_POINT ( 'NONE',  ( 0.000000000000000000, 1.459547570502463198, -6.894905428400257996 ) ) ;
#7684 = CARTESIAN_POINT ( 'NONE',  ( 25.04750000136559507, -1.913930629741527500, 2.363507492473149618 ) ) ;
#7685 = DIRECTION ( 'NONE',  ( -0.8660254037844442587, 0.4999999999999902300, 0.000000000000000000 ) ) ;
#7687 = VERTEX_POINT ( 'NONE', #27628 ) ;
#7686 = CARTESIAN_POINT ( 'NONE',  ( 0.1962428234089072521, -6.885380501030516243, 1.500000000000000444 ) ) ;
#7688 = CARTESIAN_POINT ( 'NONE',  ( -5.862550801365593145, -3.521866450007987037, -0.3701630799359323931 ) ) ;
#7689 = PLANE ( 'NONE',  #25678 ) ;
#7690 = B_SPLINE_CURVE_WITH_KNOTS ( 'NONE', 3,
 ( #17061, #4391, #14573, #12073, #22268, #31817, #24278, #1392, #30152, #17417 ),
 .UNSPECIFIED., .F., .F.,
 ( 4, 3, 3, 4 ),
 ( 2.540777767531316248E-16, 0.001000000000058556262, 0.002000000000115103715, 0.003363950672707366474 ),
 .UNSPECIFIED. ) ;
#7691 = CARTESIAN_POINT ( 'NONE',  ( 4.749760686538667009, -6.139290821770219786, -5.151476664237539360 ) ) ;
#7692 = DIRECTION ( 'NONE',  ( 0.000000000000000000, -0.8191520442889975717, 0.5735764363510378328 ) ) ;
#7693 = ORIENTED_EDGE ( 'NONE', *, *, #5999, .T. ) ;
#7695 = ORIENTED_EDGE ( 'NONE', *, *, #30179, .T. ) ;
#7694 = CARTESIAN_POINT ( 'NONE',  ( 24.31705961743306332, -17.33693665021637287, 1.331050360517170850 ) ) ;
#7696 = CIRCLE ( 'NONE', #23188, 8.749000000000002331 ) ;
#7697 = AXIS2_PLACEMENT_3D ( 'NONE', #15817, #11118, #8447 ) ;
#7698 = CARTESIAN_POINT ( 'NONE',  ( 21.08401840680096129, -16.78474387324269657, -1.500000000000000000 ) ) ;
#7699 = CARTESIAN_POINT ( 'NONE',  ( 107.9622325421415212, 20.81773585569407459, -1.491740999229417941 ) ) ;
#7700 = CIRCLE ( 'NONE', #31716, 10.43371088333262087 ) ;
#7701 = CARTESIAN_POINT ( 'NONE',  ( 21.29750000136559507, -2.363507492473152283, -1.913930629741525280 ) ) ;
#7702 = CARTESIAN_POINT ( 'NONE',  ( -30.19835004250544586, 10.24026612823149662, 1.500000000000003109 ) ) ;
#7703 = CARTESIAN_POINT ( 'NONE',  ( 0.5690620474499710202, -15.77263461755453910, -1.499999999999999112 ) ) ;
#7704 = B_SPLINE_CURVE_WITH_KNOTS ( 'NONE', 3,
 ( #15007, #32935, #10005, #31400, #645, #30918 ),
 .UNSPECIFIED., .F., .F.,
 ( 4, 2, 4 ),
 ( -1.393543241286607919E-05, 0.0003807901956958054720, 0.0007755158238044769503 ),
 .UNSPECIFIED. ) ;
#7705 = DIRECTION ( 'NONE',  ( -1.000000000000000000, 0.000000000000000000, 0.000000000000000000 ) ) ;
#7706 = PRODUCT_DEFINITION_FORMATION_WITH_SPECIFIED_SOURCE ( 'ANY', '', #22028, .NOT_KNOWN. ) ;
#7707 = LINE ( 'NONE', #28420, #1751 ) ;
#7708 = CARTESIAN_POINT ( 'NONE',  ( 69.38611993481310947, -8.080330187051606217, 2.713652344655544724 ) ) ;
#7709 = VERTEX_POINT ( 'NONE', #19613 ) ;
#7710 = CARTESIAN_POINT ( 'NONE',  ( 3.249999999999999556, 0.000000000000000000, 0.000000000000000000 ) ) ;
#7711 = ADVANCED_FACE ( 'NONE', ( #29811 ), #27289, .T. ) ;
#7712 = APPLICATION_PROTOCOL_DEFINITION ( 'international standard', 'config_control_design', 1994, #16282 ) ;
#7713 = CARTESIAN_POINT ( 'NONE',  ( -32.37020706055090358, 18.00000000000000355, -0.3702070605508915868 ) ) ;
#7714 = VERTEX_POINT ( 'NONE', #7068 ) ;
#7715 = EDGE_CURVE ( 'NONE', #4279, #1557, #27320, .T. ) ;
#7716 = VECTOR ( 'NONE', #13114, 1000.000000000000000 ) ;
#7717 = CARTESIAN_POINT ( 'NONE',  ( 10.52034268205830259, -3.024842911000718892, 3.993798362933297597 ) ) ;
#7718 = ORIENTED_EDGE ( 'NONE', *, *, #31689, .T. ) ;
#7719 = CARTESIAN_POINT ( 'NONE',  ( -17.30305273768104612, 8.786760116294463074, 2.016332066590946770 ) ) ;
#7721 = EDGE_LOOP ( 'NONE', ( #31047, #5452, #3450, #22937 ) ) ;
#7720 = CARTESIAN_POINT ( 'NONE',  ( 18.85746438010532700, -4.770484898610086510, -4.043900693820822845 ) ) ;
#7722 = EDGE_CURVE ( 'NONE', #30399, #27411, #10057, .T. ) ;
#7723 = ORIENTED_EDGE ( 'NONE', *, *, #7179, .F. ) ;
#7724 = FACE_OUTER_BOUND ( 'NONE', #12786, .T. ) ;
#7725 = DIRECTION ( 'NONE',  ( 0.000000000000000000, 0.9063077870366514910, -0.4226182617406961106 ) ) ;
#7726 = CARTESIAN_POINT ( 'NONE',  ( 20.86000000136559152, 0.2613211581691317065, 2.486304738420681559 ) ) ;
#7727 = DIRECTION ( 'NONE',  ( 0.000000000000000000, 0.000000000000000000, -1.000000000000000000 ) ) ;
#7729 = VERTEX_POINT ( 'NONE', #30473 ) ;
#7728 = DIRECTION ( 'NONE',  ( -1.000000000000000000, 8.574039729943018344E-17, 0.000000000000000000 ) ) ;
#7730 = DIRECTION ( 'NONE',  ( -0.4999999999999978906, -0.8660254037844397068, -9.233562054644581322E-18 ) ) ;
#7731 = CARTESIAN_POINT ( 'NONE',  ( 26.23173791223905837, 19.12152673998438601, 1.050000000000000044 ) ) ;
#7732 = EDGE_CURVE ( 'NONE', #25433, #14402, #6673, .T. ) ;
#7733 = CARTESIAN_POINT ( 'NONE',  ( -2.787252791270956376, -12.40549665431308846, 1.499999999999999556 ) ) ;
#7734 = CARTESIAN_POINT ( 'NONE',  ( 25.23500000136559507, -1.570731468192933633, -2.892927487894330074 ) ) ;
#7735 = CARTESIAN_POINT ( 'NONE',  ( 21.79750000136559507, 2.363507492473148286, 1.913930629741525058 ) ) ;
#7736 = DIRECTION ( 'NONE',  ( 0.000000000000000000, 0.8191520442889883569, 0.5735764363510510444 ) ) ;
#7738 = ORIENTED_EDGE ( 'NONE', *, *, #8704, .T. ) ;
#7737 = CARTESIAN_POINT ( 'NONE',  ( 107.5620253939523820, -18.98724223319534232, -4.512175692148537642 ) ) ;
#7739 = DIRECTION ( 'NONE',  ( 0.000000000000000000, 0.9056868434498948073, 0.4239473335235944829 ) ) ;
#7740 = CARTESIAN_POINT ( 'NONE',  ( -26.98657589828505721, 17.41894840571574576, 1.798104102373871971 ) ) ;
#7741 = CARTESIAN_POINT ( 'NONE',  ( 23.67250000273118360, -2.378061970571983430, 1.291182301015471712 ) ) ;
#7742 = EDGE_CURVE ( 'NONE', #15410, #29829, #23053, .T. ) ;
#7743 = DIRECTION ( 'NONE',  ( 0.000000000000000000, 0.000000000000000000, 1.000000000000000000 ) ) ;
#7744 = DIRECTION ( 'NONE',  ( -8.281886410780519655E-17, -0.9659258262890698665, 0.2588190451025149663 ) ) ;
#7745 = DIRECTION ( 'NONE',  ( 0.000000000000000000, -0.8660254037844432595, 0.4999999999999918954 ) ) ;
#7746 = CIRCLE ( 'NONE', #13083, 11.18125977723849296 ) ;
#7747 = ORIENTED_EDGE ( 'NONE', *, *, #15037, .F. ) ;
#7748 = LINE ( 'NONE', #386, #31121 ) ;
#7749 = EDGE_CURVE ( 'NONE', #26914, #11692, #17176, .T. ) ;
#7750 = LINE ( 'NONE', #20935, #1229 ) ;
#7751 = CARTESIAN_POINT ( 'NONE',  ( -5.037550801365593856, -1.088641768524163611, -3.675193018007245627 ) ) ;
#7752 = ORIENTED_EDGE ( 'NONE', *, *, #6708, .F. ) ;
#7753 = CARTESIAN_POINT ( 'NONE',  ( 20.64125000204838756, 0.2896100032356176412, 2.755455120372265476 ) ) ;
#7754 = CARTESIAN_POINT ( 'NONE',  ( 6.038145208238977268, 7.553619661406968611, -3.842870190353619542 ) ) ;
#7755 = ADVANCED_FACE ( 'NONE', ( #30970 ), #32987, .T. ) ;
#7756 = CARTESIAN_POINT ( 'NONE',  ( 1.565787006715317453, -2.348723853601462075, -0.9788672205888330202 ) ) ;
#7757 = CARTESIAN_POINT ( 'NONE',  ( 102.9885081044300534, -6.698322160490901567, 0.07017451552781736601 ) ) ;
#7758 = EDGE_CURVE ( 'NONE', #20668, #10785, #22930, .T. ) ;
#7759 = VERTEX_POINT ( 'NONE', #10228 ) ;
#7760 = CARTESIAN_POINT ( 'NONE',  ( 0.7632845268398871230, 0.000000000000000000, 0.000000000000000000 ) ) ;
#7761 = ORIENTED_EDGE ( 'NONE', *, *, #302, .F. ) ;
#7762 = CARTESIAN_POINT ( 'NONE',  ( 107.4811514614839325, -17.81167296463705085, 5.070933786246803798 ) ) ;
#7764 = ORIENTED_EDGE ( 'NONE', *, *, #1425, .F. ) ;
#7763 = CARTESIAN_POINT ( 'NONE',  ( 10.52034268205830259, 3.641590349731929077, 3.055657119358814011 ) ) ;
#7765 = ORIENTED_EDGE ( 'NONE', *, *, #22450, .F. ) ;
#7766 = CARTESIAN_POINT ( 'NONE',  ( 7.064423659272771161, -4.973063321325243535, -7.199384779417551172 ) ) ;
#7767 = EDGE_CURVE ( 'NONE', #1536, #9966, #10284, .T. ) ;
#7768 = VERTEX_POINT ( 'NONE', #2406 ) ;
#7769 = CARTESIAN_POINT ( 'NONE',  ( 6.880159396099833735, -7.192972099401662156, 4.949130873693353472 ) ) ;
#7771 = VERTEX_POINT ( 'NONE', #27969 ) ;
#7770 = CARTESIAN_POINT ( 'NONE',  ( 10.00000000000000178, 4.208382051008192626, 2.718385644597191231 ) ) ;
#7772 = CARTESIAN_POINT ( 'NONE',  ( 0.1764088899269929123, -7.476879701952443114, -1.774401973390820952 ) ) ;
#7773 = DIRECTION ( 'NONE',  ( -1.000000000000000000, 0.000000000000000000, 0.000000000000000000 ) ) ;
#7774 = CARTESIAN_POINT ( 'NONE',  ( 19.46384663066824672, -15.80031286499690069, -0.9999999999998614442 ) ) ;
#7775 = CARTESIAN_POINT ( 'NONE',  ( 107.9409393647361668, -17.21890366125716199, 3.165031064497942470 ) ) ;
#7776 = ADVANCED_FACE ( 'NONE', ( #12895 ), #5576, .F. ) ;
#7777 = CARTESIAN_POINT ( 'NONE',  ( 5.612973690782940395, 8.213905076232780544, 0.1996300861631225554 ) ) ;
#7778 = DIRECTION ( 'NONE',  ( 8.541412920197206256E-17, 0.9961946980917449901, 0.08715574274766552110 ) ) ;
#7779 = CARTESIAN_POINT ( 'NONE',  ( 11.04311965146451335, 15.00000000000000355, 1.500000000000000000 ) ) ;
#7780 = CARTESIAN_POINT ( 'NONE',  ( 56.97280603064898941, -277.2763395528616002, 2.334455007174201402 ) ) ;
#7781 = CARTESIAN_POINT ( 'NONE',  ( 47.75999538435722513, -8.435302152663906483, -0.07017451552783579571 ) ) ;
#7782 = CARTESIAN_POINT ( 'NONE',  ( -3.830085165118302378E-16, -4.467071865485461757, -1.625881193364742572 ) ) ;
#7783 = DIRECTION ( 'NONE',  ( 0.000000000000000000, 0.000000000000000000, -1.000000000000000000 ) ) ;
#7784 = LINE ( 'NONE', #92, #14513 ) ;
#7785 = EDGE_CURVE ( 'NONE', #9508, #17100, #22782, .T. ) ;
#7786 = CARTESIAN_POINT ( 'NONE',  ( -2.750050802731187627, 2.983565686104819648, 0.3135853898029609677 ) ) ;
#7787 = VERTEX_POINT ( 'NONE', #2561 ) ;
#7788 = CARTESIAN_POINT ( 'NONE',  ( -6.587550801365593678, 0.3701630799359330593, -3.521866450007987037 ) ) ;
#7789 = CARTESIAN_POINT ( 'NONE',  ( 9.038457413085614789, 1.187263343935665344E-16, -1.016831166589732938 ) ) ;
#7790 = ADVANCED_FACE ( 'NONE', ( #28126 ), #5387, .T. ) ;
#7791 = CARTESIAN_POINT ( 'NONE',  ( -18.35000000000000142, -10.96966150227469505, 1.500000000000000000 ) ) ;
#7792 = ORIENTED_EDGE ( 'NONE', *, *, #29662, .T. ) ;
#7793 = CARTESIAN_POINT ( 'NONE',  ( 18.84751037367278315, -4.881750713116288054, -4.171867820445587682 ) ) ;
#7794 =( LENGTH_UNIT ( ) NAMED_UNIT ( * ) SI_UNIT ( .MILLI., .METRE. ) );
#7795 = ADVANCED_FACE ( 'NONE', ( #25608 ), #22627, .T. ) ;
#7796 = ORIENTED_EDGE ( 'NONE', *, *, #20179, .F. ) ;
#7797 = CARTESIAN_POINT ( 'NONE',  ( 0.000000000000000000, 7.008469740302810891, 2.257469275785292329 ) ) ;
#7798 = PERSON_AND_ORGANIZATION ( #6766, #25292 ) ;
#7800 = EDGE_LOOP ( 'NONE', ( #20540, #28435, #28031, #15230 ) ) ;
#7799 = CARTESIAN_POINT ( 'NONE',  ( 3.566513200368869096, -17.47573827932033197, -1.499999999999999556 ) ) ;
#7801 = EDGE_LOOP ( 'NONE', ( #13920, #16520, #9221, #1662, #17269, #10732, #18904, #9259, #21243, #2031, #15103, #3672, #21670, #6279, #19785, #10305, #17369, #28034, #2332, #23968, #30902, #5028, #20290, #21339, #21267, #32706, #26252, #20782, #27401, #13496, #5877, #25439, #31561, #1866, #10250, #9100, #7680, #11668, #7572, #16609, #10422, #16607, #18429, #16768, #25241, #5509 ) ) ;
#7802 = DIRECTION ( 'NONE',  ( 1.000000000000000000, -0.000000000000000000, -0.000000000000000000 ) ) ;
#7803 = ORIENTED_EDGE ( 'NONE', *, *, #4230, .F. ) ;
#7804 = CARTESIAN_POINT ( 'NONE',  ( 5.887529311434773760, 0.3723788567094480362, -8.386653846779015709 ) ) ;
#7806 = ORIENTED_EDGE ( 'NONE', *, *, #31710, .T. ) ;
#7805 = CARTESIAN_POINT ( 'NONE',  ( -2.473317512238808025, -0.04024842339950747416, 3.068583371689424855 ) ) ;
#7807 = DIRECTION ( 'NONE',  ( 0.8528685319524443864, -0.4924038765061020118, 0.1736481776669307753 ) ) ;
#7808 = DIRECTION ( 'NONE',  ( 8.281886410780482677E-17, 0.9659258262890646485, 0.2588190451025343397 ) ) ;
#7809 = DIRECTION ( 'NONE',  ( -0.000000000000000000, 0.000000000000000000, 1.000000000000000000 ) ) ;
#7810 = DIRECTION ( 'NONE',  ( 6.062761635205612732E-17, 0.7071067811865510144, -0.7071067811865441310 ) ) ;
#7811 = EDGE_CURVE ( 'NONE', #19163, #4533, #19051, .T. ) ;
#7812 = VERTEX_POINT ( 'NONE', #31309 ) ;
#7813 = DIRECTION ( 'NONE',  ( -1.000000000000000000, -0.000000000000000000, -0.000000000000000000 ) ) ;
#7814 = FACE_OUTER_BOUND ( 'NONE', #26893, .T. ) ;
#7815 = DIRECTION ( 'NONE',  ( 0.000000000000000000, 0.000000000000000000, 1.000000000000000000 ) ) ;
#7816 = CARTESIAN_POINT ( 'NONE',  ( 101.7221769401408409, -2.897900707892763439, -3.993434276071010203 ) ) ;
#7817 = CARTESIAN_POINT ( 'NONE',  ( -8.000050800000012785, -0.1176501200716436601, 3.189834295598466873 ) ) ;
#7818 = CARTESIAN_POINT ( 'NONE',  ( 0.7212197595511942172, -0.5238431420100444491, 8.936767016217512349 ) ) ;
#7819 = CARTESIAN_POINT ( 'NONE',  ( -56.31355482043776561, 0.1467473176864696194, -1.355220493667176118 ) ) ;
#7820 = DIRECTION ( 'NONE',  ( 0.000000000000000000, -0.000000000000000000, -1.000000000000000000 ) ) ;
#7821 = EDGE_LOOP ( 'NONE', ( #12191, #5658, #19940, #31650 ) ) ;
#7822 = CARTESIAN_POINT ( 'NONE',  ( -5.112550801365594033, -3.675193018007246071, 1.088641768524163167 ) ) ;
#7823 = ORIENTED_EDGE ( 'NONE', *, *, #22872, .F. ) ;
#7824 = EDGE_CURVE ( 'NONE', #27107, #30379, #21415, .T. ) ;
#7825 = CARTESIAN_POINT ( 'NONE',  ( -4.704531657079158435, -2.975847129947406522, -0.3127741368606805072 ) ) ;
#7826 = ADVANCED_FACE ( 'NONE', ( #6350 ), #27080, .T. ) ;
#7827 = CARTESIAN_POINT ( 'NONE',  ( 108.0843398541090039, 18.64779751147721143, 4.615451654196422560 ) ) ;
#7828 = CARTESIAN_POINT ( 'NONE',  ( 48.08400536259535585, -8.675012021204926427, -2.713652344655543391 ) ) ;
#7829 = CARTESIAN_POINT ( 'NONE',  ( 7.193574579132851810, -9.614801642835368867, 1.500000000000000000 ) ) ;
#7830 = ORIENTED_EDGE ( 'NONE', *, *, #19980, .T. ) ;
#7831 = CARTESIAN_POINT ( 'NONE',  ( 21.48306690750116132, -21.75443153431600152, 1.466605545616818995 ) ) ;
#7832 = ORIENTED_EDGE ( 'NONE', *, *, #9153, .F. ) ;
#7833 = CARTESIAN_POINT ( 'NONE',  ( 0.7632845268458183785, 8.152713396062706508, 3.174628368984090176 ) ) ;
#7834 = CALENDAR_DATE ( 2026, 6, 10 ) ;
#7835 = CARTESIAN_POINT ( 'NONE',  ( 28.66649852640073348, -6.671163739231440459, 4.112224495658902690 ) ) ;
#7836 = B_SPLINE_CURVE_WITH_KNOTS ( 'NONE', 3,
 ( #12538, #32299, #16883, #27079, #20080, #7347, #27585, #7013 ),
 .UNSPECIFIED., .F., .F.,
 ( 4, 2, 2, 4 ),
 ( 2.197717257119807428E-07, 0.001262070444977244840, 0.001892995781603009492, 0.002523921118228774144 ),
 .UNSPECIFIED. ) ;
#7837 = LINE ( 'NONE', #30257, #4291 ) ;
#7839 = DIRECTION ( 'NONE',  ( -1.000000000000000000, 0.000000000000000000, 0.000000000000000000 ) ) ;
#7838 = CARTESIAN_POINT ( 'NONE',  ( 7.249760686538667009, -5.151476664237518044, 6.139290821770238438 ) ) ;
#7840 = ORIENTED_EDGE ( 'NONE', *, *, #18575, .T. ) ;
#7841 = CARTESIAN_POINT ( 'NONE',  ( -8.000050800000003903, -0.2821670390570966691, -3.000056433408583079 ) ) ;
#7842 = DIRECTION ( 'NONE',  ( 1.000000000000000000, -8.574039729943018344E-17, -0.000000000000000000 ) ) ;
#7843 = CARTESIAN_POINT ( 'NONE',  ( 21.11000000136559152, -2.892927487894331406, 1.570731468192932301 ) ) ;
#7844 = CARTESIAN_POINT ( 'NONE',  ( 0.000000000000000000, 0.000000000000000000, 0.000000000000000000 ) ) ;
#7846 = ORIENTED_EDGE ( 'NONE', *, *, #5872, .T. ) ;
#7845 = CARTESIAN_POINT ( 'NONE',  ( 108.2511990071235175, 19.57693511493973659, -2.786268106232082431 ) ) ;
#7847 = CARTESIAN_POINT ( 'NONE',  ( -5.812550801365592434, -3.368539882008727115, -1.828967928396028064 ) ) ;
#7848 = CARTESIAN_POINT ( 'NONE',  ( 0.000000000000000000, 0.000000000000000000, 0.000000000000000000 ) ) ;
#7849 = CARTESIAN_POINT ( 'NONE',  ( 5.377543748152547209, 1.391664247347333294, -7.892520144992419162 ) ) ;
#7850 = CYLINDRICAL_SURFACE ( 'NONE', #1124, 2.999999999999999112 ) ;
#7851 = ORIENTED_EDGE ( 'NONE', *, *, #16510, .F. ) ;
#7852 = ORIENTED_EDGE ( 'NONE', *, *, #32172, .F. ) ;
#7853 = CARTESIAN_POINT ( 'NONE',  ( 0.7632845268398871230, 4.729683950898978750, -7.360373001730866171 ) ) ;
#7854 = EDGE_CURVE ( 'NONE', #2520, #30204, #25731, .T. ) ;
#7855 = CARTESIAN_POINT ( 'NONE',  ( 22.42250000136559507, -0.3178988483021076838, -3.024605502323848949 ) ) ;
#7856 = ADVANCED_FACE ( 'NONE', ( #16386 ), #16046, .T. ) ;
#7857 = CARTESIAN_POINT ( 'NONE',  ( 40.87556030649425765, -5.373140178136390332, 3.390607986860986411 ) ) ;
#7858 = CARTESIAN_POINT ( 'NONE',  ( 10.00000000000000000, 4.681538312723516171, 0.8254815157535410064 ) ) ;
#7859 = CARTESIAN_POINT ( 'NONE',  ( 24.50111451137534146, -3.256483526998273983E-15, 2.499999999999998668 ) ) ;
#7860 =( BOUNDED_CURVE ( )  B_SPLINE_CURVE ( 2, ( #23986, #27012, #18653, #13949, #24476, #26667, #28854, #23841, #11472, #16151, #1594 ),
 .UNSPECIFIED., .F., .F. ) 
 B_SPLINE_CURVE_WITH_KNOTS ( ( 3, 2, 2, 2, 2, 3 ),
 ( 0.8966116191895003862, 0.9000000000000000222, 0.9250000000000000444, 0.9499999999999999556, 0.9749999999999999778, 0.9966116191895003640 ),
 .UNSPECIFIED. ) 
 CURVE ( )  GEOMETRIC_REPRESENTATION_ITEM ( )  RATIONAL_B_SPLINE_CURVE ( ( 0.9821626249036858880, 0.9896829947469992783, 1.000000000000000000, 0.9238795325112867385, 1.000000000000000000, 0.9238795325112867385, 1.000000000000000000, 0.9238795325112867385, 1.000000000000000000, 0.9341965377642874602, 0.9821626249036858880 ) ) 
 REPRESENTATION_ITEM ( '' )  );
#7861 = ADVANCED_FACE ( 'NONE', ( #5721 ), #531, .F. ) ;
#7862 = PLANE ( 'NONE',  #13469 ) ;
#7863 = CARTESIAN_POINT ( 'NONE',  ( 85.12704628545890273, -6.675959057343738401, 1.529339193916483097 ) ) ;
#7864 = EDGE_LOOP ( 'NONE', ( #16740, #18227, #26639, #30780, #17643, #11113, #27, #30840 ) ) ;
#7865 = CARTESIAN_POINT ( 'NONE',  ( 1.624999999999999778, 7.593217523260696211, -7.958834565716684573 ) ) ;
#7866 = CARTESIAN_POINT ( 'NONE',  ( 101.8016823592329274, -4.042758964359259188, -3.993434276136486716 ) ) ;
#7867 = ORIENTED_EDGE ( 'NONE', *, *, #826, .T. ) ;
#7868 = CARTESIAN_POINT ( 'NONE',  ( 108.0329590114848486, 18.36168870583371415, -4.580901328277968254 ) ) ;
#7869 = VERTEX_POINT ( 'NONE', #13375 ) ;
#7870 = DIRECTION ( 'NONE',  ( 8.574039729943018344E-17, 1.000000000000000000, 0.000000000000000000 ) ) ;
#7872 = ORIENTED_EDGE ( 'NONE', *, *, #26506, .T. ) ;
#7871 = CARTESIAN_POINT ( 'NONE',  ( 28.69209672924516852, -5.673860896767527251, -4.073741754953343452 ) ) ;
#7873 = ORIENTED_EDGE ( 'NONE', *, *, #28557, .F. ) ;
#7874 = CARTESIAN_POINT ( 'NONE',  ( 14.13431920379513862, -20.70626837987542856, 1.500000000000000000 ) ) ;
#7875 = CARTESIAN_POINT ( 'NONE',  ( -6.212550801365593678, 3.368539882008727115, 1.828967928396027176 ) ) ;
#7876 = CARTESIAN_POINT ( 'NONE',  ( 7.249760686538667009, 0.000000000000000000, 0.000000000000000000 ) ) ;
#7877 = DIRECTION ( 'NONE',  ( 0.000000000000000000, 0.000000000000000000, 1.000000000000000000 ) ) ;
#7879 = ORIENTED_EDGE ( 'NONE', *, *, #14733, .F. ) ;
#7878 = CARTESIAN_POINT ( 'NONE',  ( 22.11000000273118715, 1.573300977624590313, -1.942864903642426144 ) ) ;
#7880 = CARTESIAN_POINT ( 'NONE',  ( 107.6134620356101550, -19.72758389683053437, 2.997181592065166988 ) ) ;
#7881 = DIRECTION ( 'NONE',  ( -0.000000000000000000, -0.000000000000000000, 1.000000000000000000 ) ) ;
#7882 = CARTESIAN_POINT ( 'NONE',  ( 5.492556933410833508, -18.10995529321820641, 1.499999999999526157 ) ) ;
#7883 = CARTESIAN_POINT ( 'NONE',  ( 21.11000000136559152, -2.892927487894331406, 1.570731468192932301 ) ) ;
#7884 = FACE_OUTER_BOUND ( 'NONE', #20592, .T. ) ;
#7886 = EDGE_LOOP ( 'NONE', ( #10551, #8730, #22842, #19925 ) ) ;
#7885 = DIRECTION ( 'NONE',  ( -1.000000000000000000, -0.000000000000000000, -0.000000000000000000 ) ) ;
#7887 = CARTESIAN_POINT ( 'NONE',  ( 10.55147673363119232, 2.285372942704952504, 4.458382051008201508 ) ) ;
#7888 = EDGE_CURVE ( 'NONE', #14918, #1346, #25013, .T. ) ;
#7889 = FACE_OUTER_BOUND ( 'NONE', #2783, .T. ) ;
#7890 = CARTESIAN_POINT ( 'NONE',  ( 20.98500000136559862, -2.892927487894331406, 1.570731468192932301 ) ) ;
#7891 = CARTESIAN_POINT ( 'NONE',  ( 10.25005080000000035, 4.286263797015736102E-16, -3.499999999999999556 ) ) ;
#7892 = DIRECTION ( 'NONE',  ( -1.000000000000000000, 0.000000000000000000, 0.000000000000000000 ) ) ;
#7893 = FACE_OUTER_BOUND ( 'NONE', #32325, .T. ) ;
#7894 = ORIENTED_EDGE ( 'NONE', *, *, #27846, .T. ) ;
#7895 = DIRECTION ( 'NONE',  ( -0.000000000000000000, -1.000000000000000000, -0.000000000000000000 ) ) ;
#7896 = LINE ( 'NONE', #4897, #28978 ) ;
#7897 = CARTESIAN_POINT ( 'NONE',  ( -2.587550801365593678, 0.3701630799359330593, -3.521866450007987037 ) ) ;
#7898 = VERTEX_POINT ( 'NONE', #10718 ) ;
#7899 = B_SPLINE_CURVE_WITH_KNOTS ( 'NONE', 3,
 ( #31720, #2059, #12406, #11301, #19767, #22626, #20119, #22438, #27779, #12230 ),
 .UNSPECIFIED., .F., .F.,
 ( 4, 2, 2, 2, 4 ),
 ( -5.999999992670980713E-08, 0.0004826161079609663949, 0.0009652922159218595751, 0.001447968323882752647, 0.001930644431843645719 ),
 .UNSPECIFIED. ) ;
#7900 = B_SPLINE_CURVE_WITH_KNOTS ( 'NONE', 3,
 ( #16830, #27030, #4131, #14299, #10623, #15308 ),
 .UNSPECIFIED., .F., .F.,
 ( 4, 2, 4 ),
 ( -5.999999986713436683E-08, 0.0003820452512025651701, 0.0007641505024049974944 ),
 .UNSPECIFIED. ) ;
#7901 = CARTESIAN_POINT ( 'NONE',  ( 7.249760686538667009, 7.199384779417189684, -4.973063321323801134 ) ) ;
#7902 = CARTESIAN_POINT ( 'NONE',  ( 68.76824089134748874, -7.257250553475476984, -2.184958019050049050 ) ) ;
#7903 = CARTESIAN_POINT ( 'NONE',  ( -1.170068671574743036, -6.059534462705075342, -4.522129901861164925 ) ) ;
#7904 = CARTESIAN_POINT ( 'NONE',  ( 9.970488656677847672, -12.00323977417178867, 1.000000000000000000 ) ) ;
#7905 = ORIENTED_EDGE ( 'NONE', *, *, #28906, .T. ) ;
#7906 = CARTESIAN_POINT ( 'NONE',  ( -41.00655594638332246, -14.01733579338419311, 5.522895031406394040 ) ) ;
#7907 = ORIENTED_EDGE ( 'NONE', *, *, #28687, .T. ) ;
#7908 = CARTESIAN_POINT ( 'NONE',  ( 107.5617723795404999, -18.98359893170737323, 4.522129901861158707 ) ) ;
#7910 = ORIENTED_EDGE ( 'NONE', *, *, #22639, .F. ) ;
#7909 = CARTESIAN_POINT ( 'NONE',  ( 25.75999999999999801, -2.208672634433321348E-15, 0.000000000000000000 ) ) ;
#7911 = ADVANCED_FACE ( 'NONE', ( #13712 ), #8869, .T. ) ;
#7912 = ORIENTED_EDGE ( 'NONE', *, *, #3641, .F. ) ;
#7913 = LINE ( 'NONE', #22952, #25157 ) ;
#7914 = ORIENTED_EDGE ( 'NONE', *, *, #1345, .T. ) ;
#7915 = DIRECTION ( 'NONE',  ( 0.1437473352845045071, 0.000000000000000000, -0.9896144216807898353 ) ) ;
#7917 = ORIENTED_EDGE ( 'NONE', *, *, #31710, .F. ) ;
#7916 = CARTESIAN_POINT ( 'NONE',  ( 71.67787245194618606, -18.34520463695562498, 1.500000000000000000 ) ) ;
#7918 = VERTEX_POINT ( 'NONE', #24069 ) ;
#7919 = DIRECTION ( 'NONE',  ( 0.04852105321274706451, -0.4695180821586696363, 0.8815886103626625614 ) ) ;
#7920 = B_SPLINE_CURVE_WITH_KNOTS ( 'NONE', 3,
 ( #4787, #27182, #22695, #14963, #32397, #4288, #14464, #24679, #1805, #11990 ),
 .UNSPECIFIED., .F., .F.,
 ( 4, 2, 2, 2, 4 ),
 ( 1.968338519012299431E-07, 0.0005467928198071724975, 0.001093388805762443789, 0.001639984791717714972, 0.002186580777672986371 ),
 .UNSPECIFIED. ) ;
#7921 = EDGE_CURVE ( 'NONE', #5364, #10426, #15417, .T. ) ;
#7922 = DIRECTION ( 'NONE',  ( 0.000000000000000000, 0.000000000000000000, 1.000000000000000000 ) ) ;
#7923 = CARTESIAN_POINT ( 'NONE',  ( 7.577572045913244736, 15.00000000000000178, -4.612695725900422872 ) ) ;
#7924 = CARTESIAN_POINT ( 'NONE',  ( 10.00000000000000000, 4.116875700062115229, -2.376879293651021019 ) ) ;
#7925 = DIRECTION ( 'NONE',  ( 0.000000000000000000, 0.5877852522924689183, 0.8090169943749504489 ) ) ;
#7926 = FACE_OUTER_BOUND ( 'NONE', #7394, .T. ) ;
#7927 = CARTESIAN_POINT ( 'NONE',  ( 1.206523839548967247, -3.371562291789969468, 1.499999999999999556 ) ) ;
#7928 = CARTESIAN_POINT ( 'NONE',  ( 7.249760686538667009, -2.741043480754877582, -7.530955069117540646 ) ) ;
#7929 = ADVANCED_FACE ( 'NONE', ( #32455 ), #22396, .T. ) ;
#7930 = EDGE_CURVE ( 'NONE', #32468, #3987, #4038, .T. ) ;
#7931 = DIRECTION ( 'NONE',  ( -1.000000000000000000, 8.574039729943015878E-17, 1.232595164407830946E-32 ) ) ;
#7932 = CARTESIAN_POINT ( 'NONE',  ( 2.770684449829438734, 0.02953710645921867745, 1.228046178477532946 ) ) ;
#7933 = CARTESIAN_POINT ( 'NONE',  ( 7.249760686538667009, -6.147671362329260702, 6.226446564517894799 ) ) ;
#7934 = CARTESIAN_POINT ( 'NONE',  ( 6.356381935169121533, -8.556754636093200972, -0.9265622495396655944 ) ) ;
#7935 = EDGE_CURVE ( 'NONE', #23082, #3747, #3848, .T. ) ;
#7936 = EDGE_CURVE ( 'NONE', #32685, #10930, #32128, .T. ) ;
#7937 = CARTESIAN_POINT ( 'NONE',  ( 10.57125986779756843, -0.8254815157535575487, 4.681538312723514395 ) ) ;
#7938 = VERTEX_POINT ( 'NONE', #6699 ) ;
#7939 = CARTESIAN_POINT ( 'NONE',  ( -5.137550801365594388, -3.368539882008727115, -1.828967928396028064 ) ) ;
#7940 = CARTESIAN_POINT ( 'NONE',  ( 25.24521618911088794, -7.644457093038323125E-15, 2.510216189110891172 ) ) ;
#7941 = FACE_OUTER_BOUND ( 'NONE', #28836, .T. ) ;
#7942 = ORIENTED_EDGE ( 'NONE', *, *, #5491, .F. ) ;
#7943 = DIRECTION ( 'NONE',  ( -0.000000000000000000, -0.000000000000000000, -1.000000000000000000 ) ) ;
#7944 = EDGE_CURVE ( 'NONE', #11273, #27732, #4228, .T. ) ;
#7945 = ORIENTED_EDGE ( 'NONE', *, *, #14443, .T. ) ;
#7946 = CARTESIAN_POINT ( 'NONE',  ( 47.98568197278774505, -2.821418575600921130, -0.07017451552781585333 ) ) ;
#7947 = PERSON_AND_ORGANIZATION ( #15526, #26422 ) ;
#7949 = EDGE_LOOP ( 'NONE', ( #6973, #10784, #20905 ) ) ;
#7948 = CARTESIAN_POINT ( 'NONE',  ( -3.889464452585704723, -3.181828567483031112, -1.499999999999999556 ) ) ;
#7950 = ORIENTED_EDGE ( 'NONE', *, *, #3223, .F. ) ;
#7951 = CARTESIAN_POINT ( 'NONE',  ( -0.1874251621923629929, -14.67762397772687777, 1.745313648524859262 ) ) ;
#7952 = ORIENTED_EDGE ( 'NONE', *, *, #21181, .T. ) ;
#7953 = LINE ( 'NONE', #31034, #16037 ) ;
#7955 = VERTEX_POINT ( 'NONE', #32305 ) ;
#7954 = CARTESIAN_POINT ( 'NONE',  ( 10.56870887191539587, -4.467071865485484850, 1.625881193364682620 ) ) ;
#7956 = FACE_OUTER_BOUND ( 'NONE', #16613, .T. ) ;
#7957 = CARTESIAN_POINT ( 'NONE',  ( -23.54713438637982748, 8.275374457817619600, 8.600000000000003197 ) ) ;
#7958 = DIRECTION ( 'NONE',  ( 0.000000000000000000, 0.000000000000000000, 1.000000000000000000 ) ) ;
#7959 = CARTESIAN_POINT ( 'NONE',  ( 0.000000000000000000, 10.76487093102067583, -1.999317321091388377 ) ) ;
#7960 = EDGE_CURVE ( 'NONE', #3234, #12922, #21899, .T. ) ;
#7961 = ORIENTED_EDGE ( 'NONE', *, *, #21321, .T. ) ;
#7962 = CARTESIAN_POINT ( 'NONE',  ( 0.000000000000000000, 0.000000000000000000, -1.500000000000000000 ) ) ;
#7963 = LINE ( 'NONE', #18007, #12937 ) ;
#7964 = LINE ( 'NONE', #28360, #17123 ) ;
#7965 = DIRECTION ( 'NONE',  ( 1.000000000000000000, 0.000000000000000000, 0.000000000000000000 ) ) ;
#7966 = ADVANCED_FACE ( 'NONE', ( #24404 ), #30524, .F. ) ;
#7967 = EDGE_CURVE ( 'NONE', #23146, #20898, #3303, .T. ) ;
#7968 = CARTESIAN_POINT ( 'NONE',  ( 24.80306213860341558, -17.49230408913766865, 1.499999999999999778 ) ) ;
#7969 = CARTESIAN_POINT ( 'NONE',  ( 21.59559372540891786, -17.25941758357568645, -1.753144073646022649 ) ) ;
#7970 = CARTESIAN_POINT ( 'NONE',  ( 23.75111450864416440, -1.283275288181523244E-15, -2.499999999999998668 ) ) ;
#7971 = CARTESIAN_POINT ( 'NONE',  ( 5.377543748152548986, -6.139290821770219786, -5.151476664237539360 ) ) ;
#7972 = ORIENTED_EDGE ( 'NONE', *, *, #28359, .F. ) ;
#7973 = VERTEX_POINT ( 'NONE', #9871 ) ;
#7974 = CARTESIAN_POINT ( 'NONE',  ( -2.804531657079157636, 2.325406398514293205, -1.883076972206379374 ) ) ;
#7975 = DIRECTION ( 'NONE',  ( -0.1767573132311699990, -0.9842544651762054064, 0.000000000000000000 ) ) ;
#7976 = CARTESIAN_POINT ( 'NONE',  ( 2.948241552139481580, -0.000000000000000000, -1.325451157388740198 ) ) ;
#7977 = CARTESIAN_POINT ( 'NONE',  ( 15.65524065576216017, -15.16498509049018040, 1.500000000000000000 ) ) ;
#7978 = EDGE_LOOP ( 'NONE', ( #17666, #22365, #13289, #28205 ) ) ;
#7979 = DIRECTION ( 'NONE',  ( 0.000000000000000000, 0.000000000000000000, -1.000000000000000000 ) ) ;
#7980 = ADVANCED_FACE ( 'NONE', ( #10023 ), #29218, .F. ) ;
#7981 = VECTOR ( 'NONE', #18111, 1000.000000000000000 ) ;
#7982 = APPROVAL ( #819, 'UNSPECIFIED' ) ;
#7983 = ORIENTED_EDGE ( 'NONE', *, *, #25146, .T. ) ;
#7984 = CARTESIAN_POINT ( 'NONE',  ( 3.020080146456704195, -0.5244911560275570261, -8.942241244950251300 ) ) ;
#7985 = DATE_AND_TIME ( #12817, #24757 ) ;
#7986 = APPLICATION_CONTEXT ( 'configuration controlled 3d designs of mechanical parts and assemblies' ) ;
#7987 = CARTESIAN_POINT ( 'NONE',  ( 102.4111596038446947, -3.824652436571373659, 4.185347658344710453 ) ) ;
#7988 = CARTESIAN_POINT ( 'NONE',  ( 9.256550853498360709, 0.1793056638302361061, 1.452626841518512402 ) ) ;
#7990 = FACE_OUTER_BOUND ( 'NONE', #4168, .T. ) ;
#7989 = CARTESIAN_POINT ( 'NONE',  ( 44.05836296526000240, -19.40445080606629702, -1.500000000000000000 ) ) ;
#7991 = ORIENTED_EDGE ( 'NONE', *, *, #17433, .T. ) ;
#7992 = CARTESIAN_POINT ( 'NONE',  ( 0.7632845268398871230, 5.538577986808899567, 6.772677083992407532 ) ) ;
#7993 = LINE ( 'NONE', #27904, #29962 ) ;
#7994 = EDGE_CURVE ( 'NONE', #7241, #10104, #12693, .T. ) ;
#7995 = CARTESIAN_POINT ( 'NONE',  ( 109.2312629696830015, 19.37684342964560003, 4.110854402524375395 ) ) ;
#7996 = CARTESIAN_POINT ( 'NONE',  ( 19.80502601021794362, -16.61823365775807559, -1.499999999999999556 ) ) ;
#7997 = CIRCLE ( 'NONE', #22405, 0.5000000000000003331 ) ;
#7999 = EDGE_LOOP ( 'NONE', ( #15733, #14030, #16637, #2241, #23227 ) ) ;
#7998 = CARTESIAN_POINT ( 'NONE',  ( 108.1156589233279135, 18.82219444680288234, -4.397958565568440115 ) ) ;
#8000 = CARTESIAN_POINT ( 'NONE',  ( -7.212550801365592790, 1.828967928396027176, -3.368539882008727115 ) ) ;
#8001 = AXIS2_PLACEMENT_3D ( 'NONE', #21643, #29672, #12102 ) ;
#8002 = CARTESIAN_POINT ( 'NONE',  ( 10.00000000000000000, -2.285372942704986254, 4.458382051008184632 ) ) ;
#8003 = CARTESIAN_POINT ( 'NONE',  ( 0.5664946525207626982, 9.241976615239526183, 2.300561732649596181 ) ) ;
#8004 = ORIENTED_EDGE ( 'NONE', *, *, #7101, .T. ) ;
#8005 = ORIENTED_EDGE ( 'NONE', *, *, #17075, .T. ) ;
#8006 = AXIS2_PLACEMENT_3D ( 'NONE', #2950, #28796, #5894 ) ;
#8007 = DIRECTION ( 'NONE',  ( -1.000000000000000000, -0.000000000000000000, -0.000000000000000000 ) ) ;
#8008 = LINE ( 'NONE', #15362, #27195 ) ;
#8009 = CARTESIAN_POINT ( 'NONE',  ( 22.92250000136559862, 0.3178988483021036315, 3.024605502323848949 ) ) ;
#8010 = CARTESIAN_POINT ( 'NONE',  ( 110.2535626002996310, 19.41193660949216238, 0.4463807625373348298 ) ) ;
#8011 = CARTESIAN_POINT ( 'NONE',  ( 2.376492135548449625, -9.437149634395570530, 5.239665997527315433 ) ) ;
#8012 = CARTESIAN_POINT ( 'NONE',  ( 0.7632845268398871230, 0.000000000000000000, -8.749000000000000554 ) ) ;
#8013 = CARTESIAN_POINT ( 'NONE',  ( 69.15727116336861968, -7.845927800133500440, 0.4367667211769182267 ) ) ;
#8014 = ORIENTED_EDGE ( 'NONE', *, *, #23019, .T. ) ;
#8015 = SPHERICAL_SURFACE ( 'NONE', #1735, 0.5000000000000000000 ) ;
#8016 = VECTOR ( 'NONE', #15850, 1000.000000000000000 ) ;
#8017 = VECTOR ( 'NONE', #23971, 1000.000000000000000 ) ;
#8018 = PERSON_AND_ORGANIZATION ( #6766, #25292 ) ;
#8019 = CARTESIAN_POINT ( 'NONE',  ( 102.5829460782277351, -0.8583298743146006160, 2.713652344655542503 ) ) ;
#8020 = ORIENTED_EDGE ( 'NONE', *, *, #30787, .T. ) ;
#8021 = CIRCLE ( 'NONE', #1112, 0.4500000000000003442 ) ;
#8022 = DIRECTION ( 'NONE',  ( 0.9993908270190957621, 0.03489949670250105246, 3.467333458611667963E-15 ) ) ;
#8023 = ORIENTED_EDGE ( 'NONE', *, *, #13191, .T. ) ;
#8024 = CARTESIAN_POINT ( 'NONE',  ( -21.32474236360683406, 4.412344421670777450, 2.134689491126265271 ) ) ;
#8026 = VERTEX_POINT ( 'NONE', #10182 ) ;
#8025 = CARTESIAN_POINT ( 'NONE',  ( 85.00069437096559000, -4.631723123766721351, -4.312042181584450518 ) ) ;
#8027 = ORIENTED_EDGE ( 'NONE', *, *, #11934, .F. ) ;
#8028 = ADVANCED_FACE ( 'NONE', ( #31723 ), #6620, .T. ) ;
#8029 = FACE_OUTER_BOUND ( 'NONE', #32427, .T. ) ;
#8030 = CARTESIAN_POINT ( 'NONE',  ( 4.749760686538667009, 7.530955069117513112, 2.741043480754951744 ) ) ;
#8031 = EDGE_CURVE ( 'NONE', #4152, #10433, #4114, .T. ) ;
#8032 = LINE ( 'NONE', #26258, #21505 ) ;
#8033 = CARTESIAN_POINT ( 'NONE',  ( 69.42401195566041849, -8.835509274224047971, -1.010822989962099960 ) ) ;
#8035 = ORIENTED_EDGE ( 'NONE', *, *, #25516, .F. ) ;
#8034 = CARTESIAN_POINT ( 'NONE',  ( -10.00000000000000000, 0.000000000000000000, 0.000000000000000000 ) ) ;
#8036 = CARTESIAN_POINT ( 'NONE',  ( 18.60402535543785518, -7.603424548862136589, -0.07017451552783579571 ) ) ;
#8037 = CARTESIAN_POINT ( 'NONE',  ( 56.97280603064898941, -277.2763395528616002, 1.508259000770582059 ) ) ;
#8038 = ADVANCED_FACE ( 'NONE', ( #8797 ), #11303, .F. ) ;
#8039 = TOROIDAL_SURFACE ( 'NONE', #32075, 10.51999999999999957, 0.4500000000000000111 ) ;
#8040 = CARTESIAN_POINT ( 'NONE',  ( -2.559292292825085191, -12.25264313511502223, 1.500000000000079492 ) ) ;
#8041 = CARTESIAN_POINT ( 'NONE',  ( 21.29750000136559507, -0.3178988483021076838, -3.024605502323848949 ) ) ;
#8042 = AXIS2_PLACEMENT_3D ( 'NONE', #14298, #8956, #29359 ) ;
#8043 = CARTESIAN_POINT ( 'NONE',  ( -10.00000000000000000, 0.000000000000000000, 0.000000000000000000 ) ) ;
#8045 = ORIENTED_EDGE ( 'NONE', *, *, #11358, .F. ) ;
#8044 = CARTESIAN_POINT ( 'NONE',  ( 107.6641765185853501, -20.45809951660527659, -1.499999999999999556 ) ) ;
#8046 = DIRECTION ( 'NONE',  ( 0.000000000000000000, 0.08715574274765046370, 0.9961946980917462113 ) ) ;
#8047 = VECTOR ( 'NONE', #27770, 1000.000000000000000 ) ;
#8048 = DIRECTION ( 'NONE',  ( -8.541412920197223512E-17, -0.9961946980917464334, 0.08715574274764813223 ) ) ;
#8049 = CARTESIAN_POINT ( 'NONE',  ( 25.36000000273118715, 1.942864903642424146, 1.573300977624592534 ) ) ;
#8050 = CARTESIAN_POINT ( 'NONE',  ( -23.35000000000000142, -10.96966150227469505, 4.000000000000000000 ) ) ;
#8051 = CARTESIAN_POINT ( 'NONE',  ( 5.377543748152548986, 6.940565734314653845, -4.007137495034738706 ) ) ;
#8052 = FACE_OUTER_BOUND ( 'NONE', #13600, .T. ) ;
#8053 = ORIENTED_EDGE ( 'NONE', *, *, #3013, .F. ) ;
#8054 = CARTESIAN_POINT ( 'NONE',  ( 7.249760686538667009, -6.226446564517873483, -6.147671362329282019 ) ) ;
#8055 = DIRECTION ( 'NONE',  ( 0.000000000000000000, 0.8191520442889884679, 0.5735764363510509334 ) ) ;
#8056 = VERTEX_POINT ( 'NONE', #21511 ) ;
#8057 = DIRECTION ( 'NONE',  ( -1.000000000000000000, -0.000000000000000000, -0.000000000000000000 ) ) ;
#8058 = VECTOR ( 'NONE', #21602, 1000.000000000000000 ) ;
#8059 = LINE ( 'NONE', #5871, #2908 ) ;
#8060 = DIRECTION ( 'NONE',  ( -0.03662738895564519870, 0.5274252892134370096, 0.8488115212910427587 ) ) ;
#8062 = CARTESIAN_POINT ( 'NONE',  ( 108.0403038335384451, -18.64972729361248582, 4.956758977629584173 ) ) ;
#8061 = CARTESIAN_POINT ( 'NONE',  ( 7.378890305931267157, -8.603354364037917534, 1.000000000000000000 ) ) ;
#8063 = VERTEX_POINT ( 'NONE', #14281 ) ;
#8064 = AXIS2_PLACEMENT_3D ( 'NONE', #1097, #797, #6268 ) ;
#8065 = AXIS2_PLACEMENT_3D ( 'NONE', #31905, #1142, #19032 ) ;
#8066 = CARTESIAN_POINT ( 'NONE',  ( -41.25643961544781035, -14.95835580254835051, 5.310642798856784808 ) ) ;
#8067 = AXIS2_PLACEMENT_3D ( 'NONE', #2297, #25364, #24851 ) ;
#8068 = VERTEX_POINT ( 'NONE', #1294 ) ;
#8069 = CARTESIAN_POINT ( 'NONE',  ( 69.38611993481310947, -8.080330187051606217, 2.713652344655544724 ) ) ;
#8070 = ORIENTED_EDGE ( 'NONE', *, *, #20049, .F. ) ;
#8071 = ORIENTED_EDGE ( 'NONE', *, *, #30179, .F. ) ;
#8072 = LINE ( 'NONE', #15270, #28908 ) ;
#8073 = EDGE_CURVE ( 'NONE', #28455, #28296, #19866, .T. ) ;
#8074 = EDGE_CURVE ( 'NONE', #14366, #7526, #7860, .T. ) ;
#8076 = CIRCLE ( 'NONE', #4887, 4.000000000000000000 ) ;
#8075 = DIRECTION ( 'NONE',  ( -1.000000000000000000, -0.000000000000000000, -0.000000000000000000 ) ) ;
#8078 = ORIENTED_EDGE ( 'NONE', *, *, #31484, .F. ) ;
#8077 = CARTESIAN_POINT ( 'NONE',  ( 6.524595551582242692, -3.779376390944526598, 7.790581746767720084 ) ) ;
#8079 = ORIENTED_EDGE ( 'NONE', *, *, #14330, .T. ) ;
#8080 = CARTESIAN_POINT ( 'NONE',  ( 6.304370421170641947, -13.59668101824182429, -1.755882049235860221 ) ) ;
#8081 = CARTESIAN_POINT ( 'NONE',  ( 3.249999999999999556, 9.241976615262160522, 2.300561732649596625 ) ) ;
#8082 = CARTESIAN_POINT ( 'NONE',  ( -1.082681991931091714, 0.000000000000000000, -4.612695725900422872 ) ) ;
#8083 = CARTESIAN_POINT ( 'NONE',  ( 7.249760686538667009, -7.892520144992426268, -1.391664247347309535 ) ) ;
#8084 = CARTESIAN_POINT ( 'NONE',  ( -30.51827900900859802, 4.402097243136377180, 5.049999999999999822 ) ) ;
#8085 = AXIS2_PLACEMENT_3D ( 'NONE', #16901, #4197, #1533 ) ;
#8086 = CARTESIAN_POINT ( 'NONE',  ( -6.650050800000001594, 2.853674364686379583, 1.549418761218565921 ) ) ;
#8087 = CARTESIAN_POINT ( 'NONE',  ( 107.9618353151786181, 20.81780380167319677, 1.508259000770582059 ) ) ;
#8088 = CARTESIAN_POINT ( 'NONE',  ( 29.20398424897078726, -7.702373504165580975, 2.184956341284221004 ) ) ;
#8089 = AXIS2_PLACEMENT_3D ( 'NONE', #18689, #8488, #11504 ) ;
#8090 = CIRCLE ( 'NONE', #630, 10.87687437218811581 ) ;
#8091 = PLANE ( 'NONE',  #21422 ) ;
#8092 = DIRECTION ( 'NONE',  ( -1.000000000000000000, -0.000000000000000000, -0.000000000000000000 ) ) ;
#8093 = ORIENTED_EDGE ( 'NONE', *, *, #22719, .T. ) ;
#8094 = CARTESIAN_POINT ( 'NONE',  ( 6.530491751506347420, -6.030130624359216540, 6.216163082443046051 ) ) ;
#8095 = VECTOR ( 'NONE', #23863, 1000.000000000000000 ) ;
#8096 = AXIS2_PLACEMENT_3D ( 'NONE', #10656, #8167, #15844 ) ;
#8097 = LINE ( 'NONE', #20500, #25755 ) ;
#8098 = DIRECTION ( 'NONE',  ( -1.000000000000000000, 0.000000000000000000, -0.000000000000000000 ) ) ;
#8099 = ORIENTED_EDGE ( 'NONE', *, *, #19166, .F. ) ;
#8100 = AXIS2_PLACEMENT_3D ( 'NONE', #15839, #18026, #8160 ) ;
#8101 = AXIS2_PLACEMENT_3D ( 'NONE', #738, #26615, #3719 ) ;
#8102 = EDGE_CURVE ( 'NONE', #1079, #4970, #27404, .T. ) ;
#8103 = LINE ( 'NONE', #5621, #14072 ) ;
#8104 = CARTESIAN_POINT ( 'NONE',  ( 108.8978791464556508, 17.52043075494136204, 4.999054092451758358 ) ) ;
#8105 = ORIENTED_EDGE ( 'NONE', *, *, #28059, .F. ) ;
#8106 = CARTESIAN_POINT ( 'NONE',  ( 19.10390797508231131, -2.015740111943978619, -0.07017451552781628354 ) ) ;
#8107 = EDGE_CURVE ( 'NONE', #14569, #10511, #3481, .T. ) ;
#8108 = ORIENTED_EDGE ( 'NONE', *, *, #21355, .T. ) ;
#8109 = DIRECTION ( 'NONE',  ( -0.9975973382524639943, -0.06927878976713693071, 0.000000000000000000 ) ) ;
#8110 = CONTEXT_DEPENDENT_SHAPE_REPRESENTATION ( #7349, #9194 ) ;
#8111 = AXIS2_PLACEMENT_3D ( 'NONE', #16812, #16460, #24333 ) ;
#8113 = ORIENTED_EDGE ( 'NONE', *, *, #4293, .F. ) ;
#8112 = CARTESIAN_POINT ( 'NONE',  ( 24.75111450864415730, -6.623356326098185375E-16, -2.499999999999998224 ) ) ;
#8114 = VERTEX_POINT ( 'NONE', #13638 ) ;
#8115 = CARTESIAN_POINT ( 'NONE',  ( -4.148661379613653111, -6.185305878765366749, 1.745226859798899577 ) ) ;
#8116 = CIRCLE ( 'NONE', #22536, 11.00000000000000000 ) ;
#8117 = AXIS2_PLACEMENT_3D ( 'NONE', #22530, #33058, #2637 ) ;
#8118 = EDGE_LOOP ( 'NONE', ( #4128, #26930 ) ) ;
#8119 =( BOUNDED_SURFACE ( )  B_SPLINE_SURFACE ( 3, 2, ( 
 ( #5443, #18312, #28521 ),
 ( #5622, #25498, #15799 ),
 ( #2780, #26008, #26159 ),
 ( #10775, #3114, #20322 ),
 ( #31206, #3266, #2605 ),
 ( #30531, #12770, #22979 ),
 ( #21297, #21154, #28818 ),
 ( #24129, #6101, #18624 ),
 ( #6398, #1415, #5916 ),
 ( #19117, #14101, #13754 ) ),
 .UNSPECIFIED., .F., .F., .F. ) 
 B_SPLINE_SURFACE_WITH_KNOTS ( ( 4, 2, 2, 2, 4 ),
 ( 3, 3 ),
 ( 0.01791456443259262232, 0.01997296323899121900, 0.02100216264219051734, 0.02151676234379016478, 0.02203136204538981568 ),
 ( 0.000000000000000000, 1.000000000000000000 ),
 .UNSPECIFIED. ) 
 GEOMETRIC_REPRESENTATION_ITEM ( )  RATIONAL_B_SPLINE_SURFACE ( (
 ( 1.000000000000000000, 0.8490876263418722925, 1.000000000000000000),
 ( 1.000000000000000000, 0.8789005871660122704, 1.000000000000000000),
 ( 1.000000000000000000, 0.9052476245291617429, 1.000000000000000000),
 ( 1.000000000000000000, 0.9409176603639005654, 1.000000000000000000),
 ( 1.000000000000000000, 0.9521522767063923531, 1.000000000000000000),
 ( 1.000000000000000000, 0.9681060328970257922, 1.000000000000000000),
 ( 1.000000000000000000, 0.9732806895433457894, 1.000000000000000000),
 ( 1.000000000000000000, 0.9832765258107477591, 1.000000000000000000),
 ( 1.000000000000000000, 0.9881226520952709480, 1.000000000000000000),
 ( 1.000000000000000000, 0.9925898118721191432, 1.000000000000000000) ) ) 
 REPRESENTATION_ITEM ( '' )  SURFACE ( )  );
#8120 = CARTESIAN_POINT ( 'NONE',  ( 25.75999999999999446, 1.024942698525265428, 2.863353032229740691 ) ) ;
#8122 = VERTEX_POINT ( 'NONE', #11131 ) ;
#8121 = CARTESIAN_POINT ( 'NONE',  ( -2.393873106538427553, 0.6788706457666772165, 3.182475034827832339 ) ) ;
#8123 = VECTOR ( 'NONE', #19408, 1000.000000000000000 ) ;
#8124 = CARTESIAN_POINT ( 'NONE',  ( 69.42401195566040428, -8.835509274224051524, 1.010822989962089746 ) ) ;
#8125 = FACE_OUTER_BOUND ( 'NONE', #27916, .T. ) ;
#8126 = EDGE_CURVE ( 'NONE', #16126, #17282, #1107, .T. ) ;
#8127 = CIRCLE ( 'NONE', #2266, 0.4500000000000008438 ) ;
#8128 = DIRECTION ( 'NONE',  ( -1.000000000000000000, -0.000000000000000000, 0.000000000000000000 ) ) ;
#8129 = DIRECTION ( 'NONE',  ( 0.000000000000000000, 0.8090169943749446757, 0.5877852522924770229 ) ) ;
#8130 = AXIS2_PLACEMENT_3D ( 'NONE', #18941, #28965, #5880 ) ;
#8131 = ORIENTED_EDGE ( 'NONE', *, *, #21321, .F. ) ;
#8132 = CYLINDRICAL_SURFACE ( 'NONE', #27782, 2.999999999999999112 ) ;
#8133 = CARTESIAN_POINT ( 'NONE',  ( -2.624406592062199728, -0.1993550914063198232, -1.626071056744967214 ) ) ;
#8134 = EDGE_CURVE ( 'NONE', #17346, #17030, #20416, .T. ) ;
#8135 = CARTESIAN_POINT ( 'NONE',  ( 29.20401286869407542, -7.702374816469336416, -2.184956341621953513 ) ) ;
#8136 = DIRECTION ( 'NONE',  ( 0.000000000000000000, 0.000000000000000000, -1.000000000000000000 ) ) ;
#8137 = FACE_OUTER_BOUND ( 'NONE', #4716, .T. ) ;
#8138 = AXIS2_PLACEMENT_3D ( 'NONE', #13993, #19370, #18877 ) ;
#8139 = CARTESIAN_POINT ( 'NONE',  ( 23.00820037127621731, -17.39482224626771156, -1.688990564600181488 ) ) ;
#8140 = CARTESIAN_POINT ( 'NONE',  ( 7.249760686538667009, 0.000000000000000000, 0.000000000000000000 ) ) ;
#8141 = CARTESIAN_POINT ( 'NONE',  ( 2.274274201625327230, 0.000000000000000000, 0.000000000000000000 ) ) ;
#8142 = CIRCLE ( 'NONE', #5482, 8.500000000000000000 ) ;
#8143 = CIRCLE ( 'NONE', #4405, 0.5000000000000004441 ) ;
#8144 = CARTESIAN_POINT ( 'NONE',  ( -4.062550801365593323, 0.3701630799359330593, -3.521866450007987037 ) ) ;
#8145 = EDGE_LOOP ( 'NONE', ( #25979, #30005, #2409 ) ) ;
#8146 = EDGE_CURVE ( 'NONE', #29452, #7632, #10262, .T. ) ;
#8147 = AXIS2_PLACEMENT_3D ( 'NONE', #16421, #4077, #17078 ) ;
#8148 = CIRCLE ( 'NONE', #26819, 8.750000000000000000 ) ;
#8149 = CARTESIAN_POINT ( 'NONE',  ( -8.100050800000001772, -0.3135853898029607456, 2.983565686104819648 ) ) ;
#8150 = ADVANCED_FACE ( 'NONE', ( #6132 ), #23595, .T. ) ;
#8151 = CIRCLE ( 'NONE', #26827, 0.5000000000000004441 ) ;
#8152 = CARTESIAN_POINT ( 'NONE',  ( 11.90652295052632503, 20.12228623747235901, -4.612695725900421984 ) ) ;
#8153 = CARTESIAN_POINT ( 'NONE',  ( 7.249760686538667009, 0.000000000000000000, 0.000000000000000000 ) ) ;
#8154 = CARTESIAN_POINT ( 'NONE',  ( 20.55552624091973968, -16.63177717300951741, 1.500000000000000000 ) ) ;
#8155 = AXIS2_PLACEMENT_3D ( 'NONE', #15723, #29089, #23393 ) ;
#8156 = ORIENTED_EDGE ( 'NONE', *, *, #18352, .T. ) ;
#8157 = CARTESIAN_POINT ( 'NONE',  ( -12.44989959798873791, 0.5000000000000000000, -12.99999999999999645 ) ) ;
#8158 = AXIS2_PLACEMENT_3D ( 'NONE', #24725, #12175, #22375 ) ;
#8159 = VERTEX_POINT ( 'NONE', #16316 ) ;
#8160 = DIRECTION ( 'NONE',  ( 0.000000000000000000, 0.000000000000000000, -1.000000000000000000 ) ) ;
#8161 = PERSON_AND_ORGANIZATION ( #6766, #25292 ) ;
#8162 = EDGE_CURVE ( 'NONE', #10245, #4314, #26845, .T. ) ;
#8163 = CARTESIAN_POINT ( 'NONE',  ( 85.02201553617686614, -4.979580722693575545, 4.215289907551350801 ) ) ;
#8164 = EDGE_CURVE ( 'NONE', #27019, #8068, #19657, .T. ) ;
#8165 = CARTESIAN_POINT ( 'NONE',  ( -4.716257286563782181, 19.50000000000000000, -4.924645716438866394 ) ) ;
#8166 = VECTOR ( 'NONE', #2987, 1000.000000000000114 ) ;
#8168 = DIRECTION ( 'NONE',  ( 1.000000000000000000, -0.000000000000000000, -0.000000000000000000 ) ) ;
#8167 = DIRECTION ( 'NONE',  ( 1.000000000000000000, -0.000000000000000000, -0.000000000000000000 ) ) ;
#8169 = AXIS2_PLACEMENT_3D ( 'NONE', #21418, #26285, #13561 ) ;
#8170 = ORIENTED_EDGE ( 'NONE', *, *, #23425, .F. ) ;
#8171 = CIRCLE ( 'NONE', #8684, 0.4499999999999999001 ) ;
#8172 = ADVANCED_FACE ( 'NONE', ( #14440 ), #4457, .F. ) ;
#8173 = CARTESIAN_POINT ( 'NONE',  ( 18.79914435243739135, -5.422385761091336853, 4.312047644171948413 ) ) ;
#8174 = DIRECTION ( 'NONE',  ( -0.1436597682917712671, 0.03489949670250103858, 0.9890115753135888532 ) ) ;
#8175 = CIRCLE ( 'NONE', #31152, 0.4499999999999997891 ) ;
#8176 = CARTESIAN_POINT ( 'NONE',  ( 21.17250000136559507, -3.024605502323851169, 0.3178988483021052969 ) ) ;
#8177 = VECTOR ( 'NONE', #11057, 1000.000000000000114 ) ;
#8179 = ORIENTED_EDGE ( 'NONE', *, *, #7010, .F. ) ;
#8178 = CARTESIAN_POINT ( 'NONE',  ( 0.000000000000000000, 0.000000000000000000, 0.000000000000000000 ) ) ;
#8180 = CARTESIAN_POINT ( 'NONE',  ( -6.112550801365593145, 1.088641768524161613, 3.675193018007247403 ) ) ;
#8181 = CARTESIAN_POINT ( 'NONE',  ( 18.65791233782715963, -7.001076235476726417, 2.184956778830005497 ) ) ;
#8182 = CARTESIAN_POINT ( 'NONE',  ( 47.93698235206657188, -7.077015994068657889, -3.390608234577424884 ) ) ;
#8183 = CIRCLE ( 'NONE', #23123, 2.999999999999999556 ) ;
#8184 = VERTEX_POINT ( 'NONE', #9596 ) ;
#8185 = VERTEX_POINT ( 'NONE', #9784 ) ;
#8186 = EDGE_CURVE ( 'NONE', #15425, #24311, #29849, .T. ) ;
#8187 = CC_DESIGN_DATE_AND_TIME_ASSIGNMENT ( #12965, #5280, ( #16786 ) ) ;
#8188 = CARTESIAN_POINT ( 'NONE',  ( 12.44989959798868817, 19.51744974835125035, 13.00000000000004441 ) ) ;
#8189 = DIRECTION ( 'NONE',  ( 7.472768010110560055E-18, 0.08715574274765119922, 0.9961946980917462113 ) ) ;
#8190 = VERTEX_POINT ( 'NONE', #21987 ) ;
#8191 = CARTESIAN_POINT ( 'NONE',  ( 4.592425496802574958E-16, 18.00000000000000355, 3.750000000000000444 ) ) ;
#8192 = DIRECTION ( 'NONE',  ( -0.4922101374339078461, -0.7179542890850304504, -0.4922101374328877177 ) ) ;
#8193 = VECTOR ( 'NONE', #753, 1000.000000000000114 ) ;
#8194 = DIRECTION ( 'NONE',  ( -0.000000000000000000, 0.8191520442889912434, -0.5735764363510468256 ) ) ;
#8195 = AXIS2_PLACEMENT_3D ( 'NONE', #25111, #8947, #9914 ) ;
#8196 = AXIS2_PLACEMENT_3D ( 'NONE', #2642, #32919, #30579 ) ;
#8197 = DIRECTION ( 'NONE',  ( -0.1413077769430314268, 0.9899657126261587337, 0.000000000000000000 ) ) ;
#8198 = CARTESIAN_POINT ( 'NONE',  ( 41.35669399754907261, -8.343390166155122856, 1.169951067571303849 ) ) ;
#8199 = ORIENTED_EDGE ( 'NONE', *, *, #28741, .F. ) ;
#8200 = DIRECTION ( 'NONE',  ( -8.326672684688674053E-17, -0.3746065934159164001, 0.9271838545667857590 ) ) ;
#8201 = EDGE_CURVE ( 'NONE', #9973, #3483, #17202, .T. ) ;
#8202 = AXIS2_PLACEMENT_3D ( 'NONE', #7172, #17365, #6980 ) ;
#8203 = AXIS2_PLACEMENT_3D ( 'NONE', #23725, #3171, #28730 ) ;
#8204 = ORIENTED_EDGE ( 'NONE', *, *, #12741, .F. ) ;
#8205 = AXIS2_PLACEMENT_3D ( 'NONE', #26083, #26575, #10533 ) ;
#8206 = PERSON_AND_ORGANIZATION_ROLE ( 'design_supplier' ) ;
#8207 = EDGE_CURVE ( 'NONE', #28814, #17955, #22557, .T. ) ;
#8209 = FACE_OUTER_BOUND ( 'NONE', #18531, .T. ) ;
#8208 = LOCAL_TIME ( 16, 7, 10.00000000000000000, #28745 ) ;
#8210 = ORIENTED_EDGE ( 'NONE', *, *, #5832, .T. ) ;
#8211 = CARTESIAN_POINT ( 'NONE',  ( 20.72684859436193250, -16.16085785620104076, -1.000000000000000222 ) ) ;
#8212 = ORIENTED_EDGE ( 'NONE', *, *, #30913, .F. ) ;
#8213 = CARTESIAN_POINT ( 'NONE',  ( 5.390905497009046421, 2.994789822248789868, 3.164707540391793028 ) ) ;
#8215 = EDGE_LOOP ( 'NONE', ( #29318, #1455, #1676, #2419 ) ) ;
#8214 = CARTESIAN_POINT ( 'NONE',  ( 69.02196556234740399, -5.145383722448461761, -4.185348026738465954 ) ) ;
#8216 = ORIENTED_EDGE ( 'NONE', *, *, #17739, .T. ) ;
#8217 = CARTESIAN_POINT ( 'NONE',  ( 7.249760686538667009, -5.151476664237435443, -6.139290821770307716 ) ) ;
#8218 = CARTESIAN_POINT ( 'NONE',  ( -5.362550801365593145, 2.228590825266444142, 2.752080473201636845 ) ) ;
#8219 = CARTESIAN_POINT ( 'NONE',  ( -2.619932554246580731E-16, -3.055657119358825557, 3.641590349731918863 ) ) ;
#8220 = CARTESIAN_POINT ( 'NONE',  ( 107.5922305810999688, -19.42186344497500983, -3.623800042533074972 ) ) ;
#8222 = ORIENTED_EDGE ( 'NONE', *, *, #26956, .F. ) ;
#8221 = DIRECTION ( 'NONE',  ( 0.4999999999999978351, 0.8660254037844398178, 0.000000000000000000 ) ) ;
#8223 = LINE ( 'NONE', #5707, #6541 ) ;
#8224 = DIRECTION ( 'NONE',  ( -1.000000000000000000, 0.000000000000000000, 0.000000000000000000 ) ) ;
#8225 = CARTESIAN_POINT ( 'NONE',  ( -2.829357234188641712, -11.58112209631934419, 1.743702880379067066 ) ) ;
#8226 = CARTESIAN_POINT ( 'NONE',  ( 0.08034255810714041601, -7.899847910285846098, 7.347818361009607280 ) ) ;
#8227 = AXIS2_PLACEMENT_3D ( 'NONE', #15257, #25306, #22790 ) ;
#8228 = CARTESIAN_POINT ( 'NONE',  ( 10.00000000000000000, 4.458382051008192626, 2.285372942704970267 ) ) ;
#8230 = EDGE_LOOP ( 'NONE', ( #369, #20549, #13640, #931 ) ) ;
#8229 = DIRECTION ( 'NONE',  ( -2.219124775574845909E-17, -0.2588190451025115246, -0.9659258262890707547 ) ) ;
#8231 = CARTESIAN_POINT ( 'NONE',  ( 3.249999999999999556, -9.314797388894900720, 1.239665997526854468 ) ) ;
#8232 = CIRCLE ( 'NONE', #26373, 0.5000000000000004441 ) ;
#8233 = EDGE_CURVE ( 'NONE', #22601, #681, #24954, .T. ) ;
#8234 = CC_DESIGN_PERSON_AND_ORGANIZATION_ASSIGNMENT ( #21229, #31427, ( #5017 ) ) ;
#8235 = CARTESIAN_POINT ( 'NONE',  ( -31.12328840805762553, -25.43932300454937945, 1.499999999999999778 ) ) ;
#8236 = CARTESIAN_POINT ( 'NONE',  ( 24.48500000273118715, 0.2613211581691317065, 2.486304738420681559 ) ) ;
#8237 = LOCAL_TIME ( 16, 7, 10.00000000000000000, #4126 ) ;
#8238 = CARTESIAN_POINT ( 'NONE',  ( 34.30158461016502258, 20.00000000000000000, 1.818740222761740633 ) ) ;
#8239 = CARTESIAN_POINT ( 'NONE',  ( 2.795120570943890215, -3.714272345030796174, -9.022485053477831585 ) ) ;
#8240 = CARTESIAN_POINT ( 'NONE',  ( -2.609487367014430070, -0.08210191867354442452, -1.553472644056464569 ) ) ;
#8241 = CARTESIAN_POINT ( 'NONE',  ( 108.0270956946189926, -18.45953337857165266, 4.403826084184283118 ) ) ;
#8242 = DIRECTION ( 'NONE',  ( -1.000000000000000000, 0.000000000000000000, 0.000000000000000000 ) ) ;
#8243 = ORIENTED_EDGE ( 'NONE', *, *, #27688, .F. ) ;
#8244 = ADVANCED_FACE ( 'NONE', ( #29693 ), #30353, .T. ) ;
#8245 = CIRCLE ( 'NONE', #19464, 3.000000000000000000 ) ;
#8246 = PLANE ( 'NONE',  #7060 ) ;
#8247 = ADVANCED_FACE ( 'NONE', ( #32876 ), #4610, .T. ) ;
#8248 = CARTESIAN_POINT ( 'NONE',  ( -3.135269660805078740, -0.5000000000000000000, -1.500000000000000000 ) ) ;
#8249 = CARTESIAN_POINT ( 'NONE',  ( 1.278428506419904798, -2.392608122357158251, -1.500000000000000444 ) ) ;
#8251 = CARTESIAN_POINT ( 'NONE',  ( 107.9807428589029286, -17.79206407539387769, 4.344990111930268739 ) ) ;
#8250 = CARTESIAN_POINT ( 'NONE',  ( 10.00000000000000000, -5.003758587302151284, 0.2499999999999993061 ) ) ;
#8252 = VERTEX_POINT ( 'NONE', #27827 ) ;
#8253 = CARTESIAN_POINT ( 'NONE',  ( 15.05218482013242820, 8.633077639384330482, -1.050000000000000044 ) ) ;
#8254 = ORIENTED_EDGE ( 'NONE', *, *, #4870, .T. ) ;
#8255 = CARTESIAN_POINT ( 'NONE',  ( 2.661997753583466242, 0.9074203448823292550, -10.09011512947408562 ) ) ;
#8257 = ORIENTED_EDGE ( 'NONE', *, *, #23198, .F. ) ;
#8256 = LINE ( 'NONE', #13573, #28306 ) ;
#8258 = ORIENTED_EDGE ( 'NONE', *, *, #28059, .T. ) ;
#8259 = CARTESIAN_POINT ( 'NONE',  ( 4.013969549054193054E-16, 4.681538312723529494, -0.8254815157534771686 ) ) ;
#8260 = APPROVAL_PERSON_ORGANIZATION ( #4623, #17997, #20169 ) ;
#8261 = CARTESIAN_POINT ( 'NONE',  ( 2.636537196392334970, 0.4393720697977969714, -1.497239384009418917 ) ) ;
#8263 = VERTEX_POINT ( 'NONE', #25153 ) ;
#8262 = DIRECTION ( 'NONE',  ( 0.000000000000000000, 0.000000000000000000, -1.000000000000000000 ) ) ;
#8264 = EDGE_LOOP ( 'NONE', ( #20214, #3360, #31210, #19907, #17443 ) ) ;
#8265 = CARTESIAN_POINT ( 'NONE',  ( -3.405997759315474660, -10.41452980168814868, -1.743528089750926657 ) ) ;
#8266 = CARTESIAN_POINT ( 'NONE',  ( 21.36776303755842932, -21.72386242187981864, -1.606475753954833108 ) ) ;
#8267 = FACE_OUTER_BOUND ( 'NONE', #18574, .T. ) ;
#8268 = CARTESIAN_POINT ( 'NONE',  ( 107.9478736030354327, -17.31875496774473078, -4.501973445319090494 ) ) ;
#8269 = CARTESIAN_POINT ( 'NONE',  ( 107.9266616237874246, -17.01330774345008123, 2.743473114337553920 ) ) ;
#8270 = VECTOR ( 'NONE', #31672, 1000.000000000000000 ) ;
#8271 = CARTESIAN_POINT ( 'NONE',  ( -6.750050800000001239, 3.113457007523260156, -0.9222479816126439855 ) ) ;
#8272 = CARTESIAN_POINT ( 'NONE',  ( 5.532104225389706365, -12.77500742877625939, 1.499999999999998668 ) ) ;
#8273 = CARTESIAN_POINT ( 'NONE',  ( 47.93698235206608160, -7.077015994075030569, 3.390608234564004508 ) ) ;
#8274 = DIRECTION ( 'NONE',  ( 1.000000000000000000, 0.000000000000000000, 0.000000000000000000 ) ) ;
#8275 = CARTESIAN_POINT ( 'NONE',  ( 5.885541838704151374, 5.105720535585501096, -6.662285765435168372 ) ) ;
#8276 = VERTEX_POINT ( 'NONE', #27161 ) ;
#8277 = CARTESIAN_POINT ( 'NONE',  ( 10.00000000000000000, 4.116875700062115229, -2.376879293651021019 ) ) ;
#8278 = CYLINDRICAL_SURFACE ( 'NONE', #5986, 2.999999999999999112 ) ;
#8279 = EDGE_CURVE ( 'NONE', #13240, #15674, #15040, .T. ) ;
#8280 = CARTESIAN_POINT ( 'NONE',  ( 18.51491971917342028, -8.599446730134173933, -0.07017451552783579571 ) ) ;
#8281 = VERTEX_POINT ( 'NONE', #9942 ) ;
#8282 = CARTESIAN_POINT ( 'NONE',  ( 23.42250000136559862, -0.3178988483021076838, -3.024605502323848949 ) ) ;
#8283 = EDGE_CURVE ( 'NONE', #10426, #30241, #15128, .T. ) ;
#8284 = DIRECTION ( 'NONE',  ( 0.000000000000000000, 1.000000000000000000, 0.000000000000000000 ) ) ;
#8285 = CARTESIAN_POINT ( 'NONE',  ( 6.749760686538667009, 0.000000000000000000, 0.000000000000000000 ) ) ;
#8286 = EDGE_LOOP ( 'NONE', ( #402, #14170, #11483, #13552 ) ) ;
#8287 = CARTESIAN_POINT ( 'NONE',  ( 18.82979855633279698, -5.079733283857774673, -4.282233996325130576 ) ) ;
#8288 = ORIENTED_EDGE ( 'NONE', *, *, #9523, .F. ) ;
#8289 = DIRECTION ( 'NONE',  ( 0.000000000000000000, 0.000000000000000000, 1.000000000000000000 ) ) ;
#8291 = ORIENTED_EDGE ( 'NONE', *, *, #8828, .T. ) ;
#8290 = CARTESIAN_POINT ( 'NONE',  ( 40.72654494865584240, -4.620392906576441305, -2.184955499788741928 ) ) ;
#8292 = ORIENTED_EDGE ( 'NONE', *, *, #25745, .F. ) ;
#8293 = CARTESIAN_POINT ( 'NONE',  ( 24.67250000136559507, 2.363507492473148286, 1.913930629741525058 ) ) ;
#8294 = B_SPLINE_CURVE_WITH_KNOTS ( 'NONE', 3,
 ( #15649, #2789, #30370, #12970, #5284, #8115, #23185, #17831, #15148, #294, #25509, #20678, #9960, #30880, #28032, #28532, #20517, #25357, #27845, #7951, #15305, #7440, #28182, #12633, #5454, #12780, #30730, #22991, #17639, #2617, #438, #28341 ),
 .UNSPECIFIED., .F., .F.,
 ( 4, 2, 2, 2, 2, 2, 2, 2, 2, 2, 2, 2, 2, 2, 2, 4 ),
 ( 0.000000000000000000, 0.004269922980577924194, 0.005337403725722405026, 0.006404884470866884991, 0.008539845961155846654, 0.009607326706300330088, 0.01067480745144481179, 0.01174228819658929696, 0.01280976894173377865, 0.01494473043202274032, 0.01601221117716722375, 0.01707969192231171066, 0.02134961490288964092, 0.02561953788346757466, 0.02988946086404550492, 0.03415938384462344213 ),
 .UNSPECIFIED. ) ;
#8295 = ORIENTED_EDGE ( 'NONE', *, *, #23425, .T. ) ;
#8296 = CARTESIAN_POINT ( 'NONE',  ( 6.883866357751288412, 0.6899766464188887838, -8.704251636488454125 ) ) ;
#8298 = VERTEX_POINT ( 'NONE', #11973 ) ;
#8297 = CARTESIAN_POINT ( 'NONE',  ( 68.93397511287616908, -3.394585223421259457, -1.169951107274167512 ) ) ;
#8299 = CARTESIAN_POINT ( 'NONE',  ( 19.70572127725480982, 15.17811413760662198, 1.050000000000000044 ) ) ;
#8300 = CARTESIAN_POINT ( 'NONE',  ( 3.499999999999999556, -1.471047635026914380, 6.892461014225956362 ) ) ;
#8301 = FACE_OUTER_BOUND ( 'NONE', #17440, .T. ) ;
#8302 = DIRECTION ( 'NONE',  ( 0.000000000000000000, 0.000000000000000000, 1.000000000000000000 ) ) ;
#8303 = ORIENTED_EDGE ( 'NONE', *, *, #17613, .F. ) ;
#8304 = CARTESIAN_POINT ( 'NONE',  ( 4.749760686538667009, -7.892520144992426268, -1.391664247347309535 ) ) ;
#8305 = CARTESIAN_POINT ( 'NONE',  ( 109.7220438555052056, -17.55815402607574782, -5.485967528433937979 ) ) ;
#8306 = CARTESIAN_POINT ( 'NONE',  ( 55.01832146648879274, -7.980226898947390346, -1.529339875107651237 ) ) ;
#8307 = CARTESIAN_POINT ( 'NONE',  ( -6.850050802731187716, 2.331437884370912705, -1.887961173149511618 ) ) ;
#8308 = EDGE_CURVE ( 'NONE', #24602, #14512, #28946, .T. ) ;
#8309 = CARTESIAN_POINT ( 'NONE',  ( 24.40680557455002386, -17.41959047392573012, 1.432979604635828075 ) ) ;
#8310 = CARTESIAN_POINT ( 'NONE',  ( 3.249999999999999556, 0.000000000000000000, 0.000000000000000000 ) ) ;
#8311 = CARTESIAN_POINT ( 'NONE',  ( 7.249760686538667009, -6.139290821770289064, 5.151476664237455871 ) ) ;
#8312 = CARTESIAN_POINT ( 'NONE',  ( 102.5305753040692736, -0.1042037546421159255, 0.07017451552782062729 ) ) ;
#8313 = CARTESIAN_POINT ( 'NONE',  ( -3.912550801365593856, 3.675193018007247403, -1.088641768524161391 ) ) ;
#8314 = ORIENTED_EDGE ( 'NONE', *, *, #27856, .T. ) ;
#8315 = CARTESIAN_POINT ( 'NONE',  ( -3.804531657079157636, -1.883076972206379818, -2.325406398514292761 ) ) ;
#8316 = DIRECTION ( 'NONE',  ( 0.000000000000000000, 0.000000000000000000, -1.000000000000000000 ) ) ;
#8317 = FACE_OUTER_BOUND ( 'NONE', #28674, .T. ) ;
#8318 = CARTESIAN_POINT ( 'NONE',  ( 11.72844750001789649, -13.05523934058538238, 1.000000000000000000 ) ) ;
#8319 = EDGE_LOOP ( 'NONE', ( #9803, #19476, #25380, #14970 ) ) ;
#8320 = CARTESIAN_POINT ( 'NONE',  ( 84.89587746248641054, -2.934653466125641152, -2.184955971586068468 ) ) ;
#8321 =( BOUNDED_CURVE ( )  B_SPLINE_CURVE ( 3, ( #181, #2169, #12354, #6444 ),
 .UNSPECIFIED., .F., .F. ) 
 B_SPLINE_CURVE_WITH_KNOTS ( ( 4, 4 ),
 ( 0.2844899013887129402, 0.5370275574894024517 ),
 .UNSPECIFIED. ) 
 CURVE ( )  GEOMETRIC_REPRESENTATION_ITEM ( )  RATIONAL_B_SPLINE_CURVE ( ( 1.000000000000000000, 0.9946924518608444288, 0.9946924518608444288, 1.000000000000000000 ) ) 
 REPRESENTATION_ITEM ( '' )  );
#8322 = ORIENTED_EDGE ( 'NONE', *, *, #21053, .F. ) ;
#8323 = CARTESIAN_POINT ( 'NONE',  ( 0.9068484513889774057, -4.286977062749324219, 1.499999999999999334 ) ) ;
#8324 = APPLICATION_PROTOCOL_DEFINITION ( 'international standard', 'config_control_design', 1994, #17589 ) ;
#8325 = ADVANCED_FACE ( 'NONE', ( #32532 ), #14686, .T. ) ;
#8326 = CARTESIAN_POINT ( 'NONE',  ( 40.88327824823386436, -6.765025065066961218, 4.150065482898403602 ) ) ;
#8327 = CARTESIAN_POINT ( 'NONE',  ( 9.192617927958238511, 0.08611596088385638226, 1.322472180770136729 ) ) ;
#8328 = FACE_OUTER_BOUND ( 'NONE', #12968, .T. ) ;
#8329 = ORIENTED_EDGE ( 'NONE', *, *, #2436, .T. ) ;
#8330 = ADVANCED_FACE ( 'NONE', ( #12618 ), #5268, .T. ) ;
#8331 = CARTESIAN_POINT ( 'NONE',  ( 18.81968905113669166, -5.192737262265858078, 4.312036717478699543 ) ) ;
#8332 = CARTESIAN_POINT ( 'NONE',  ( 0.3749743548324790399, 10.05686762493600028, -0.8908839545097162471 ) ) ;
#8333 = DIRECTION ( 'NONE',  ( 0.000000000000000000, 0.000000000000000000, 1.000000000000000000 ) ) ;
#8335 = EDGE_LOOP ( 'NONE', ( #5558, #15328, #5016, #17366 ) ) ;
#8334 = CARTESIAN_POINT ( 'NONE',  ( 0.4082220075202627196, -6.684754012654100741, 0.9788672205888330202 ) ) ;
#8336 = CARTESIAN_POINT ( 'NONE',  ( -2.612550801365594477, -3.368539882008727115, -1.828967928396028064 ) ) ;
#8337 = ADVANCED_FACE ( 'NONE', ( #2599 ), #15938, .F. ) ;
#8338 = CARTESIAN_POINT ( 'NONE',  ( 18.60402535544292846, -7.603424548862589560, 0.4426577274541249607 ) ) ;
#8339 = CARTESIAN_POINT ( 'NONE',  ( 35.28555349212372505, -7.422113525891726127, -2.787782628876159574 ) ) ;
#8340 = ORIENTED_EDGE ( 'NONE', *, *, #10429, .T. ) ;
#8341 = EDGE_LOOP ( 'NONE', ( #24396, #31158, #25510, #3677 ) ) ;
#8342 = FACE_OUTER_BOUND ( 'NONE', #10420, .T. ) ;
#8343 = CARTESIAN_POINT ( 'NONE',  ( 107.6300027435836313, -19.96576125925905032, -2.508990583258498663 ) ) ;
#8344 = ORIENTED_EDGE ( 'NONE', *, *, #13399, .F. ) ;
#8345 = EDGE_CURVE ( 'NONE', #16032, #25766, #8097, .T. ) ;
#8346 = EDGE_CURVE ( 'NONE', #10694, #26222, #7784, .T. ) ;
#8347 = DIRECTION ( 'NONE',  ( 0.000000000000000000, -0.5735764363510537089, 0.8191520442889864695 ) ) ;
#8348 = CARTESIAN_POINT ( 'NONE',  ( 0.7632845268449801601, 2.223716399040764014, 8.461683424485153537 ) ) ;
#8349 = DIRECTION ( 'NONE',  ( -0.4999999999999977796, -0.8660254037844398178, 0.000000000000000000 ) ) ;
#8350 = CARTESIAN_POINT ( 'NONE',  ( 0.5032039692105039208, -9.704418393844072455, -0.7352278974791732757 ) ) ;
#8351 = CARTESIAN_POINT ( 'NONE',  ( 23.61515526891508188, -8.000136145883233851, 0.8105616806102798888 ) ) ;
#8352 = EDGE_LOOP ( 'NONE', ( #14794, #30637, #28128, #18619 ) ) ;
#8353 = CARTESIAN_POINT ( 'NONE',  ( 6.037141848526922594, -2.473100090966218190, 8.105561522824304532 ) ) ;
#8354 = ORIENTED_EDGE ( 'NONE', *, *, #12424, .F. ) ;
#8355 = DATE_TIME_ROLE ( 'creation_date' ) ;
#8356 = CARTESIAN_POINT ( 'NONE',  ( 29.35001421184127324, -4.582605737176272953, 4.522129901861162260 ) ) ;
#8357 = ORIENTED_EDGE ( 'NONE', *, *, #19047, .F. ) ;
#8358 = EDGE_CURVE ( 'NONE', #4598, #1159, #13396, .T. ) ;
#8359 = PLANE ( 'NONE',  #18374 ) ;
#8360 = EDGE_LOOP ( 'NONE', ( #2077, #21605, #17278, #20810 ) ) ;
#8361 = LINE ( 'NONE', #3369, #29517 ) ;
#8362 = ORIENTED_EDGE ( 'NONE', *, *, #23951, .F. ) ;
#8363 = ORIENTED_EDGE ( 'NONE', *, *, #24697, .F. ) ;
#8364 = DIRECTION ( 'NONE',  ( 8.574039729943018344E-17, 1.000000000000000000, 0.000000000000000000 ) ) ;
#8365 = CARTESIAN_POINT ( 'NONE',  ( -5.762550801365593500, -2.228590825266444586, -2.752080473201636401 ) ) ;
#8366 = CARTESIAN_POINT ( 'NONE',  ( 21.08401840680159367, -16.78474387324287775, 1.500000000000000000 ) ) ;
#8367 = CARTESIAN_POINT ( 'NONE',  ( 0.9354051327728147847, -3.271575928939224553, -1.500000000000276890 ) ) ;
#8369 = ORIENTED_EDGE ( 'NONE', *, *, #25298, .F. ) ;
#8368 = CARTESIAN_POINT ( 'NONE',  ( 6.037141848526922594, 7.798898458906324827, -3.315649934461640136 ) ) ;
#8370 = CARTESIAN_POINT ( 'NONE',  ( -6.037550801365592967, -3.675193018007246071, 1.088641768524163167 ) ) ;
#8371 = CARTESIAN_POINT ( 'NONE',  ( 16.52153293541288548, 12.50053646836298427, 1.500000000000000000 ) ) ;
#8372 = PERSON ( 'NAUO-PER8', 'UNSPECIFIED', 'UNSPECIFIED', ('UNSPECIFIED'), ('UNSPECIFIED'), ('UNSPECIFIED') ) ;
#8373 = CARTESIAN_POINT ( 'NONE',  ( 14.56323991668084794, -20.55228079977623068, 1.750894133678834841 ) ) ;
#8374 = FACE_BOUND ( 'NONE', #15543, .T. ) ;
#8375 = CARTESIAN_POINT ( 'NONE',  ( 2.998015176062106324, -0.2419477797672030250, 1.432989973798650452 ) ) ;
#8376 = ADVANCED_FACE ( 'NONE', ( #25492 ), #8278, .T. ) ;
#8378 = ORIENTED_EDGE ( 'NONE', *, *, #5183, .T. ) ;
#8377 = DIRECTION ( 'NONE',  ( 8.574039729943018344E-17, 1.000000000000000000, 0.000000000000000000 ) ) ;
#8379 = FACE_OUTER_BOUND ( 'NONE', #21535, .T. ) ;
#8380 = CARTESIAN_POINT ( 'NONE',  ( 41.20585001718147566, -8.497180311781161066, 0.07017451552781736601 ) ) ;
#8381 = CARTESIAN_POINT ( 'NONE',  ( 24.29750000273118715, 2.594547506269380133, 0.7685399846772031918 ) ) ;
#8382 = EDGE_CURVE ( 'NONE', #6843, #32892, #30525, .T. ) ;
#8383 = EDGE_CURVE ( 'NONE', #12214, #19072, #22190, .T. ) ;
#8384 = CARTESIAN_POINT ( 'NONE',  ( -19.58167718253661604, 5.525525355233698477, 1.499999999999569011 ) ) ;
#8385 = CARTESIAN_POINT ( 'NONE',  ( 1.624999999999999778, 5.222868219166995729, -9.680994141368717720 ) ) ;
#8386 = CARTESIAN_POINT ( 'NONE',  ( -3.162653373153519798, 0.0004983460144661164444, -1.055926639513774745 ) ) ;
#8387 = CARTESIAN_POINT ( 'NONE',  ( 24.39659513448239991, -17.41072360183627055, 1.416990234759656575 ) ) ;
#8388 = B_SPLINE_SURFACE_WITH_KNOTS ( 'NONE', 1, 3, ( 
 ( #20237, #4543, #7708, #15034, #17903, #14717, #22751, #4853 ),
 ( #20091, #7517, #2375, #25421, #12548, #7208, #22901, #27931 ) ),
 .UNSPECIFIED., .F., .F., .F.,
 ( 2, 2 ),
 ( 4, 2, 2, 4 ),
 ( 0.000000000000000000, 1.000000000000000000 ),
 ( 0.000000000000000000, 0.5000000000000000000, 0.7500000000000000000, 1.000000000000000000 ),
 .UNSPECIFIED. ) ;
#8389 = CARTESIAN_POINT ( 'NONE',  ( 5.865515302491369098, 15.00000000000000000, -1.491740999229417941 ) ) ;
#8390 = ORIENTED_EDGE ( 'NONE', *, *, #10708, .T. ) ;
#8391 = CARTESIAN_POINT ( 'NONE',  ( -56.71071518287084245, 0.7496615022747066259, 1.500000000000000000 ) ) ;
#8392 = CARTESIAN_POINT ( 'NONE',  ( -3.222375984151267581, 0.000000000000000000, -1.000000000000000000 ) ) ;
#8393 = CARTESIAN_POINT ( 'NONE',  ( 29.11693253001929449, -8.303828435806623887, -0.07017451552783451896 ) ) ;
#8395 = CARTESIAN_POINT ( 'NONE',  ( 108.0493838057754914, -18.78047663426704617, 4.827283856852130128 ) ) ;
#8394 = DIRECTION ( 'NONE',  ( 1.000000000000000000, -8.574039729943018344E-17, -0.000000000000000000 ) ) ;
#8396 = VERTEX_POINT ( 'NONE', #24297 ) ;
#8397 = ADVANCED_FACE ( 'NONE', ( #29303 ), #11586, .F. ) ;
#8398 = APPROVAL ( #17195, 'UNSPECIFIED' ) ;
#8399 = DIRECTION ( 'NONE',  ( 0.000000000000000000, 0.9659258262890668689, 0.2588190451025257910 ) ) ;
#8400 = ORIENTED_EDGE ( 'NONE', *, *, #25584, .F. ) ;
#8401 = LINE ( 'NONE', #26301, #24124 ) ;
#8403 = VERTEX_POINT ( 'NONE', #26489 ) ;
#8402 = LINE ( 'NONE', #23929, #23506 ) ;
#8404 = ORIENTED_EDGE ( 'NONE', *, *, #22244, .F. ) ;
#8405 = CARTESIAN_POINT ( 'NONE',  ( 23.61632761762281163, -8.296864917633445913, -2.713652344655543391 ) ) ;
#8406 = CARTESIAN_POINT ( 'NONE',  ( -5.850050802731187716, 1.887961173149511618, 2.331437884370912705 ) ) ;
#8408 = ORIENTED_EDGE ( 'NONE', *, *, #1396, .F. ) ;
#8407 = CARTESIAN_POINT ( 'NONE',  ( 7.249760686538667009, -3.748318449932352081, 7.906491560603652324 ) ) ;
#8409 = ORIENTED_EDGE ( 'NONE', *, *, #1022, .T. ) ;
#8410 = CARTESIAN_POINT ( 'NONE',  ( 14.60944221173904722, -20.56080756410654331, -1.750898334667394973 ) ) ;
#8411 = CARTESIAN_POINT ( 'NONE',  ( 108.0291781248180598, -18.48951985539477505, -4.325670280508457921 ) ) ;
#8412 = DIRECTION ( 'NONE',  ( 0.4999999999999978906, 0.8660254037844399289, -0.000000000000000000 ) ) ;
#8413 = CARTESIAN_POINT ( 'NONE',  ( -2.500050800000000351, -0.3135853898029607456, 2.983565686104819648 ) ) ;
#8414 = FACE_OUTER_BOUND ( 'NONE', #20122, .T. ) ;
#8415 = EDGE_CURVE ( 'NONE', #8879, #29777, #12401, .T. ) ;
#8416 = B_SPLINE_CURVE_WITH_KNOTS ( 'NONE', 3,
 ( #22920, #12880, #20756, #10212, #18423, #7880, #15887, #23574, #30653, #220 ),
 .UNSPECIFIED., .F., .F.,
 ( 4, 3, 3, 4 ),
 ( 2.385244779468109755E-18, 0.001000000000068484085, 0.002000000000134635400, 0.003364209820971502535 ),
 .UNSPECIFIED. ) ;
#8417 = FACE_OUTER_BOUND ( 'NONE', #7949, .T. ) ;
#8418 = CARTESIAN_POINT ( 'NONE',  ( 0.6070402175060268801, -7.493581194466792716, 1.500000000000000444 ) ) ;
#8419 = CARTESIAN_POINT ( 'NONE',  ( 7.249760686538667009, -6.940565734314625423, 4.007137495034787555 ) ) ;
#8420 = CARTESIAN_POINT ( 'NONE',  ( 42.88108885380913193, -22.62752020922543750, 4.522129901861158707 ) ) ;
#8421 = CARTESIAN_POINT ( 'NONE',  ( 2.458207506242486851, -0.2539630985812899033, 1.478790212540433746 ) ) ;
#8422 = VERTEX_POINT ( 'NONE', #31679 ) ;
#8423 = CARTESIAN_POINT ( 'NONE',  ( 109.3993806922052698, 20.31298924473501444, 2.334455007174201402 ) ) ;
#8424 = FACE_OUTER_BOUND ( 'NONE', #24589, .T. ) ;
#8425 = CARTESIAN_POINT ( 'NONE',  ( 4.749760686538667009, -6.940565734314570356, -4.007137495034885255 ) ) ;
#8426 = ORIENTED_EDGE ( 'NONE', *, *, #27178, .T. ) ;
#8427 = CARTESIAN_POINT ( 'NONE',  ( 24.79750000136559507, 2.363507492473148286, 1.913930629741525058 ) ) ;
#8428 = CARTESIAN_POINT ( 'NONE',  ( 25.41500598742548434, -2.668779812802359430, -0.3011795608359353338 ) ) ;
#8429 = CARTESIAN_POINT ( 'NONE',  ( 2.357329973329945982, 9.815384016743308848, 4.593471141847078165 ) ) ;
#8430 = EDGE_LOOP ( 'NONE', ( #16683, #21150, #29510, #21298 ) ) ;
#8431 = CARTESIAN_POINT ( 'NONE',  ( 6.883866621640342132, 7.111352071735089098, -5.066432324612653915 ) ) ;
#8432 = EDGE_CURVE ( 'NONE', #8281, #635, #8142, .T. ) ;
#8433 = ORIENTED_EDGE ( 'NONE', *, *, #13414, .F. ) ;
#8434 = ORIENTED_EDGE ( 'NONE', *, *, #22489, .T. ) ;
#8435 = FACE_OUTER_BOUND ( 'NONE', #28885, .T. ) ;
#8437 = EDGE_LOOP ( 'NONE', ( #31344, #6953, #13771 ) ) ;
#8436 = CARTESIAN_POINT ( 'NONE',  ( 22.75111450864416085, -1.241879311143409511E-16, -2.499999999999998668 ) ) ;
#8438 = ORIENTED_EDGE ( 'NONE', *, *, #16302, .F. ) ;
#8439 = CARTESIAN_POINT ( 'NONE',  ( -15.12340757463330654, -27.93932300454937590, -1.000000000000000000 ) ) ;
#8440 = EDGE_LOOP ( 'NONE', ( #30495, #32182, #7228, #24539, #7952, #23709, #16862, #15094 ) ) ;
#8441 = CARTESIAN_POINT ( 'NONE',  ( -7.400050800000000706, 1.887961173149511618, 2.331437884370912705 ) ) ;
#8443 = ORIENTED_EDGE ( 'NONE', *, *, #26832, .F. ) ;
#8442 = DIRECTION ( 'NONE',  ( 2.219124775574847758E-17, 0.2588190451025115246, 0.9659258262890707547 ) ) ;
#8444 = FACE_OUTER_BOUND ( 'NONE', #30651, .T. ) ;
#8445 = CARTESIAN_POINT ( 'NONE',  ( 0.7080126359153782190, 8.723904125990792124, 2.275870607900281950 ) ) ;
#8446 = ADVANCED_FACE ( 'NONE', ( #21293 ), #21781, .T. ) ;
#8447 = DIRECTION ( 'NONE',  ( 0.000000000000000000, 0.000000000000000000, -1.000000000000000000 ) ) ;
#8448 = LINE ( 'NONE', #12790, #22055 ) ;
#8449 = EDGE_CURVE ( 'NONE', #30480, #13484, #16424, .T. ) ;
#8450 = CARTESIAN_POINT ( 'NONE',  ( 108.0279038916327323, -18.47117121451548272, 4.374159544809090860 ) ) ;
#8451 = ADVANCED_FACE ( 'NONE', ( #8424 ), #6097, .T. ) ;
#8452 = CARTESIAN_POINT ( 'NONE',  ( 3.499999999999999556, 6.704570150426983233, 2.172265885002680808 ) ) ;
#8453 = FACE_OUTER_BOUND ( 'NONE', #30731, .T. ) ;
#8454 = CARTESIAN_POINT ( 'NONE',  ( 41.35640441665029954, -8.240600375904646668, -1.529340244838580887 ) ) ;
#8455 = CARTESIAN_POINT ( 'NONE',  ( -6.962942409646511344, 7.727249047114547632E-16, -2.999999999999999556 ) ) ;
#8456 = DIRECTION ( 'NONE',  ( 1.000000000000000000, -0.000000000000000000, -0.000000000000000000 ) ) ;
#8457 = CARTESIAN_POINT ( 'NONE',  ( 22.80257594975842395, -21.89069150541910957, 1.310091732169401668 ) ) ;
#8458 = DIRECTION ( 'NONE',  ( -0.000000000000000000, -0.000000000000000000, -1.000000000000000000 ) ) ;
#8459 = CARTESIAN_POINT ( 'NONE',  ( 107.6641398346956890, -20.45810202417174750, -1.499999999999999556 ) ) ;
#8460 = CARTESIAN_POINT ( 'NONE',  ( -4.112550801365593145, -1.088641768524163389, -3.675193018007246071 ) ) ;
#8461 = ORIENTED_EDGE ( 'NONE', *, *, #587, .T. ) ;
#8462 = CARTESIAN_POINT ( 'NONE',  ( -5.300050800000001061, 0.3135853898029611342, -2.983565686104819648 ) ) ;
#8463 = CARTESIAN_POINT ( 'NONE',  ( 8.901201215455847304, 15.00000000000002132, -5.396302277755718357 ) ) ;
#8464 = CARTESIAN_POINT ( 'NONE',  ( -4.957304906975410042, 1.062355717592091686, 3.000000000000001332 ) ) ;
#8465 = CARTESIAN_POINT ( 'NONE',  ( 7.931701156347861215, -9.929036423920559074, 1.500000000000000000 ) ) ;
#8466 = VERTEX_POINT ( 'NONE', #21464 ) ;
#8467 = CARTESIAN_POINT ( 'NONE',  ( 102.3434546416267352, -2.854938759700329953, -3.993434327340286583 ) ) ;
#8468 = B_SPLINE_CURVE_WITH_KNOTS ( 'NONE', 3,
 ( #12027, #12520, #12338, #10154 ),
 .UNSPECIFIED., .F., .F.,
 ( 4, 4 ),
 ( 0.000000000000000000, 2.202192133514975633E-08 ),
 .UNSPECIFIED. ) ;
#8469 = ORIENTED_EDGE ( 'NONE', *, *, #17788, .T. ) ;
#8470 = CARTESIAN_POINT ( 'NONE',  ( 2.053765210313523770, -0.9196025812828518831, 1.500000000001123768 ) ) ;
#8471 = APPROVAL_DATE_TIME ( #11143, #7982 ) ;
#8472 = CARTESIAN_POINT ( 'NONE',  ( 69.02940965802889650, -5.294544073377518423, 4.275175994965093373 ) ) ;
#8473 = EDGE_CURVE ( 'NONE', #12070, #18469, #20261, .T. ) ;
#8474 = LINE ( 'NONE', #329, #27793 ) ;
#8475 = CARTESIAN_POINT ( 'NONE',  ( 12.27700767694853390, 19.86581740147262209, 5.412820279296879811 ) ) ;
#8476 = ORIENTED_EDGE ( 'NONE', *, *, #32671, .F. ) ;
#8477 = CARTESIAN_POINT ( 'NONE',  ( 18.82980128142734344, -5.079702822763886516, 4.282223223018092995 ) ) ;
#8478 = FACE_OUTER_BOUND ( 'NONE', #26912, .T. ) ;
#8479 = CYLINDRICAL_SURFACE ( 'NONE', #19945, 303.6457063863960002 ) ;
#8481 = ORIENTED_EDGE ( 'NONE', *, *, #10579, .F. ) ;
#8480 = CARTESIAN_POINT ( 'NONE',  ( 2.889143798718252221, 0.000000000000000000, 0.9788672205888330202 ) ) ;
#8482 = CARTESIAN_POINT ( 'NONE',  ( -2.762550801365593500, -2.752080473201636845, 2.228590825266444586 ) ) ;
#8483 = DIRECTION ( 'NONE',  ( 6.938893903907228378E-15, 0.000000000000000000, -1.000000000000000000 ) ) ;
#8484 = CARTESIAN_POINT ( 'NONE',  ( 13.62547635268498070, 21.94000000000005102, -1.491740999229417941 ) ) ;
#8485 = ORIENTED_EDGE ( 'NONE', *, *, #10856, .F. ) ;
#8486 = ORIENTED_EDGE ( 'NONE', *, *, #7854, .F. ) ;
#8487 = DIRECTION ( 'NONE',  ( 0.000000000000000000, 0.000000000000000000, 1.000000000000000000 ) ) ;
#8488 = DIRECTION ( 'NONE',  ( 1.000000000000000000, 0.000000000000000000, 0.000000000000000000 ) ) ;
#8489 = CARTESIAN_POINT ( 'NONE',  ( 10.57125986779756843, 0.6226916219172030642, 4.971152295393303611 ) ) ;
#8490 = CARTESIAN_POINT ( 'NONE',  ( 109.5084093630373872, -17.21855534384547326, 4.522129901861156931 ) ) ;
#8491 = B_SPLINE_CURVE_WITH_KNOTS ( 'NONE', 3,
 ( #2864, #21697, #8827, #32410, #1327, #8971 ),
 .UNSPECIFIED., .F., .F.,
 ( 4, 2, 4 ),
 ( 0.000000000000000000, 0.0009761896101137411321, 0.001952379220227482264 ),
 .UNSPECIFIED. ) ;
#8492 = EDGE_LOOP ( 'NONE', ( #21193, #12523, #5550, #21603, #1427, #16188 ) ) ;
#8493 = CARTESIAN_POINT ( 'NONE',  ( -8.000050800000000351, 0.000000000000000000, 0.000000000000000000 ) ) ;
#8494 = CARTESIAN_POINT ( 'NONE',  ( 10.55147673363118876, 2.376879293651121383, -4.116875700062057497 ) ) ;
#8495 =( BOUNDED_SURFACE ( )  B_SPLINE_SURFACE ( 3, 2, ( 
 ( #29618, #26937, #26598 ),
 ( #31952, #19077, #13713 ),
 ( #11393, #8870, #22092 ),
 ( #24405, #1523, #6528 ),
 ( #24070, #11699, #16734 ),
 ( #24563, #3699, #1195 ),
 ( #26754, #32306, #19575 ),
 ( #31624, #3870, #6351 ),
 ( #14048, #21591, #18928 ),
 ( #31799, #29265, #29771 ),
 ( #6850, #8714, #29118 ),
 ( #6203, #16387, #20087 ),
 ( #7353, #27741, #14862 ),
 ( #27591, #30280, #2179 ),
 ( #27246, #30433, #24912 ),
 ( #32800, #7513, #4363 ),
 ( #24755, #22585, #25418 ),
 ( #4540, #25062, #4848 ),
 ( #2526, #9872, #12694 ),
 ( #17544, #15030, #9693 ),
 ( #25249, #2371, #10024 ),
 ( #12544, #22748, #22898 ),
 ( #7703, #14541, #14713 ),
 ( #7204, #1875, #10183 ),
 ( #2025, #12051, #5596 ),
 ( #32954, #27924, #12197 ),
 ( #22247, #20234, #12366 ),
 ( #20406, #30620, #22397 ),
 ( #32456, #17715, #27436 ),
 ( #5037, #9515, #4692 ),
 ( #15216, #19731, #29933 ),
 ( #32614, #7020, #17230 ),
 ( #19918, #30129, #17397 ),
 ( #11020, #20887, #2874 ) ),
 .UNSPECIFIED., .F., .F., .F. ) 
 B_SPLINE_SURFACE_WITH_KNOTS ( ( 4, 2, 2, 2, 2, 2, 2, 2, 2, 2, 2, 2, 2, 2, 2, 2, 4 ),
 ( 3, 3 ),
 ( 0.000000000000000000, 0.004360795930118540123, 0.005450994912648174720, 0.006541193895177810184, 0.008721591860237080246, 0.009811790842766714843, 0.01090198982529634944, 0.01199218880782598404, 0.01308238779035562037, 0.01526278575541489130, 0.01635298473794452589, 0.01744318372047416049, 0.02180397965059269888, 0.02398437761565196807, 0.02616477558071124074, 0.03052557151082978260, 0.03488636744094832098 ),
 ( 0.000000000000000000, 1.000000000000000000 ),
 .UNSPECIFIED. ) 
 GEOMETRIC_REPRESENTATION_ITEM ( )  RATIONAL_B_SPLINE_SURFACE ( (
 ( 1.000000000000000000, 0.8508761217583473702, 1.000000000000000000),
 ( 1.000000000000000000, 0.8513495135180835227, 1.000000000000000000),
 ( 1.000000000000000000, 0.8517270363692717172, 1.000000000000000000),
 ( 1.000000000000000000, 0.8525422031685686575, 1.000000000000000000),
 ( 1.000000000000000000, 0.8526809929701213431, 1.000000000000000000),
 ( 1.000000000000000000, 0.8529405693517642106, 1.000000000000000000),
 ( 1.000000000000000000, 0.8530607691951643812, 1.000000000000000000),
 ( 1.000000000000000000, 0.8534148638638719975, 1.000000000000000000),
 ( 1.000000000000000000, 0.8536546893696659311, 1.000000000000000000),
 ( 1.000000000000000000, 0.8539620067557214256, 1.000000000000000000),
 ( 1.000000000000000000, 0.8540316192635319936, 1.000000000000000000),
 ( 1.000000000000000000, 0.8540602109241151041, 1.000000000000000000),
 ( 1.000000000000000000, 0.8540396564185858130, 1.000000000000000000),
 ( 1.000000000000000000, 0.8539811336537593833, 1.000000000000000000),
 ( 1.000000000000000000, 0.8539432050989358425, 1.000000000000000000),
 ( 1.000000000000000000, 0.8538670370114783692, 1.000000000000000000),
 ( 1.000000000000000000, 0.8538286120051845618, 1.000000000000000000),
 ( 1.000000000000000000, 0.8536849753243391792, 1.000000000000000000),
 ( 1.000000000000000000, 0.8533602685196585158, 1.000000000000000000),
 ( 1.000000000000000000, 0.8529654596012481438, 1.000000000000000000),
 ( 1.000000000000000000, 0.8528244218823842759, 1.000000000000000000),
 ( 1.000000000000000000, 0.8525299725566436448, 1.000000000000000000),
 ( 1.000000000000000000, 0.8523761395252034134, 1.000000000000000000),
 ( 1.000000000000000000, 0.8516129481394613121, 1.000000000000000000),
 ( 1.000000000000000000, 0.8513036087791725492, 1.000000000000000000),
 ( 1.000000000000000000, 0.8508287454031215891, 1.000000000000000000),
 ( 1.000000000000000000, 0.8506601076795354821, 1.000000000000000000),
 ( 1.000000000000000000, 0.8503078255506797412, 1.000000000000000000),
 ( 1.000000000000000000, 0.8501262613430246029, 1.000000000000000000),
 ( 1.000000000000000000, 0.8496349353270501448, 1.000000000000000000),
 ( 1.000000000000000000, 0.8494863696526087082, 1.000000000000000000),
 ( 1.000000000000000000, 0.8492518783361784340, 1.000000000000000000),
 ( 1.000000000000000000, 0.8491664931671285554, 1.000000000000000000),
 ( 1.000000000000000000, 0.8490876263417841407, 1.000000000000000000) ) ) 
 REPRESENTATION_ITEM ( '' )  SURFACE ( )  );
#8496 = CARTESIAN_POINT ( 'NONE',  ( -30.49402871571406948, -10.96966150227469505, -11.00000000000000000 ) ) ;
#8497 = CARTESIAN_POINT ( 'NONE',  ( -2.249956573341760357, 1.323625320507108460, 3.284597389080124774 ) ) ;
#8498 = CARTESIAN_POINT ( 'NONE',  ( 107.9802527803231129, -17.78500706576168611, -4.325704939595124365 ) ) ;
#8499 = CARTESIAN_POINT ( 'NONE',  ( 85.14283307489679942, -6.932413485865819069, 0.07017451552782748292 ) ) ;
#8500 = ORIENTED_EDGE ( 'NONE', *, *, #7101, .F. ) ;
#8501 = CARTESIAN_POINT ( 'NONE',  ( 6.880159540721328959, -2.328896285337246130, 8.414807581959454552 ) ) ;
#8503 = ADVANCED_FACE ( 'NONE', ( #31495 ), #8578, .T. ) ;
#8502 = VERTEX_POINT ( 'NONE', #26631 ) ;
#8504 = PERSON_AND_ORGANIZATION ( #6766, #25292 ) ;
#8505 = CARTESIAN_POINT ( 'NONE',  ( 28.66412654021265283, -6.764326628257229856, 3.995006647739479888 ) ) ;
#8506 = AXIS2_PLACEMENT_3D ( 'NONE', #14949, #22681, #16972 ) ;
#8507 = EDGE_CURVE ( 'NONE', #20422, #10078, #1467, .T. ) ;
#8508 = DIRECTION ( 'NONE',  ( -0.03489949670250104552, 0.9993908270190956511, 0.000000000000000000 ) ) ;
#8509 = ORIENTED_EDGE ( 'NONE', *, *, #25687, .T. ) ;
#8510 = DIRECTION ( 'NONE',  ( -1.000000000000000000, 0.000000000000000000, 0.000000000000000000 ) ) ;
#8511 = ORIENTED_EDGE ( 'NONE', *, *, #17976, .F. ) ;
#8512 = ORIENTED_EDGE ( 'NONE', *, *, #31237, .T. ) ;
#8513 = ADVANCED_FACE ( 'NONE', ( #14097 ), #4055, .T. ) ;
#8514 = EDGE_CURVE ( 'NONE', #32756, #14180, #26332, .T. ) ;
#8515 = CARTESIAN_POINT ( 'NONE',  ( 4.749760686538667009, 6.940565734314653845, -4.007137495034738706 ) ) ;
#8516 = CARTESIAN_POINT ( 'NONE',  ( -3.612550801365593589, -1.828967928396026732, 3.368539882008728004 ) ) ;
#8517 = VECTOR ( 'NONE', #16615, 1000.000000000000000 ) ;
#8519 = ORIENTED_EDGE ( 'NONE', *, *, #28359, .T. ) ;
#8518 = CARTESIAN_POINT ( 'NONE',  ( 0.5704037183048226156, -5.066169706250006399, 8.085411865508406848 ) ) ;
#8520 = CARTESIAN_POINT ( 'NONE',  ( -8.187550801365594211, 0.3701630799359330593, -3.521866450007987037 ) ) ;
#8521 = CARTESIAN_POINT ( 'NONE',  ( 16.18510121775752353, 12.06909784052177237, 1.500000000000000000 ) ) ;
#8522 = CYLINDRICAL_SURFACE ( 'NONE', #30015, 0.5000000000000004441 ) ;
#8523 = CARTESIAN_POINT ( 'NONE',  ( 22.29750000136559507, -0.3178988483021076838, -3.024605502323848949 ) ) ;
#8526 = EDGE_CURVE ( 'NONE', #16840, #30035, #5433, .T. ) ;
#8525 = ORIENTED_EDGE ( 'NONE', *, *, #24787, .F. ) ;
#8524 = CARTESIAN_POINT ( 'NONE',  ( 2.864531019710234272, -3.575186956654052395, 8.868883597856999756 ) ) ;
#8527 = CARTESIAN_POINT ( 'NONE',  ( -24.45088912031106076, 4.048764718688453002, 2.144778699193373939 ) ) ;
#8528 = CARTESIAN_POINT ( 'NONE',  ( 21.92250000273118715, -1.291182301015472378, -2.378061970571982098 ) ) ;
#8529 = DIRECTION ( 'NONE',  ( 0.000000000000000000, 0.000000000000000000, 1.000000000000000000 ) ) ;
#8530 = ADVANCED_FACE ( 'NONE', ( #32171 ), #7075, .F. ) ;
#8531 = VECTOR ( 'NONE', #25641, 1000.000000000000000 ) ;
#8532 = CARTESIAN_POINT ( 'NONE',  ( 79.17573959169237696, 22.98125563777605151, 4.629213727441585213 ) ) ;
#8533 = DIRECTION ( 'NONE',  ( 0.02413862388702639472, -0.9993908270190956511, 0.02520519206291751621 ) ) ;
#8534 = DIRECTION ( 'NONE',  ( 1.000000000000000000, 0.000000000000000000, 0.000000000000000000 ) ) ;
#8535 = VECTOR ( 'NONE', #20475, 1000.000000000000000 ) ;
#8536 = DIRECTION ( 'NONE',  ( 0.000000000000000000, 0.7071067811865495711, -0.7071067811865454633 ) ) ;
#8537 = CARTESIAN_POINT ( 'NONE',  ( -5.437550801365592434, 1.088641768524161613, 3.675193018007247403 ) ) ;
#8538 = ORIENTED_EDGE ( 'NONE', *, *, #10765, .T. ) ;
#8539 = VECTOR ( 'NONE', #12570, 1000.000000000000000 ) ;
#8540 = CARTESIAN_POINT ( 'NONE',  ( 20.03174988220922614, -21.67712946496415682, 1.441661034764442073 ) ) ;
#8541 = CARTESIAN_POINT ( 'NONE',  ( -3.029003146408718372, -0.04861012228918290545, -1.223725428626261991 ) ) ;
#8542 = DIRECTION ( 'NONE',  ( 0.4999999999999982236, 0.8660254037844398178, 0.000000000000000000 ) ) ;
#8544 = CARTESIAN_POINT ( 'NONE',  ( 35.00000000000000000, 18.00000000000000355, 0.3702070605511352808 ) ) ;
#8543 = DIRECTION ( 'NONE',  ( 1.000000000000000000, -8.574039729943018344E-17, -0.000000000000000000 ) ) ;
#8545 = ORIENTED_EDGE ( 'NONE', *, *, #28340, .F. ) ;
#8546 = FACE_OUTER_BOUND ( 'NONE', #26869, .T. ) ;
#8547 = EDGE_LOOP ( 'NONE', ( #31215, #8896, #6706, #32559, #25499, #4967, #1072 ) ) ;
#8548 = CARTESIAN_POINT ( 'NONE',  ( -7.800050800000000173, -1.887961173149512062, -2.331437884370912261 ) ) ;
#8550 = EDGE_LOOP ( 'NONE', ( #29636, #16787, #27787, #15146 ) ) ;
#8549 = DIRECTION ( 'NONE',  ( -1.000000000000000000, 0.000000000000000000, 0.000000000000000000 ) ) ;
#8551 = ORIENTED_EDGE ( 'NONE', *, *, #7509, .F. ) ;
#8552 = CARTESIAN_POINT ( 'NONE',  ( 41.44907012423725234, -8.741883605788331124, -2.713652344655543391 ) ) ;
#8553 = ADVANCED_FACE ( 'NONE', ( #19468 ), #29659, .T. ) ;
#8554 = ADVANCED_FACE ( 'NONE', ( #17084, #4080 ), #4225, .T. ) ;
#8555 = AXIS2_PLACEMENT_3D ( 'NONE', #27960, #7885, #5378 ) ;
#8556 = CARTESIAN_POINT ( 'NONE',  ( -5.950050802731187360, 2.983565686104819648, 0.3135853898029609677 ) ) ;
#8558 = VERTEX_POINT ( 'NONE', #9742 ) ;
#8557 = CARTESIAN_POINT ( 'NONE',  ( 3.499999999999999556, -2.652816298622462376, 5.657964889053574531 ) ) ;
#8559 = CARTESIAN_POINT ( 'NONE',  ( 4.749760686538667009, 6.940565734314653845, -4.007137495034738706 ) ) ;
#8560 = CIRCLE ( 'NONE', #4850, 8.749000000000002331 ) ;
#8561 = CARTESIAN_POINT ( 'NONE',  ( -4.102049215352101541, -5.462733247114307744, -1.745628864018728743 ) ) ;
#8562 = DIRECTION ( 'NONE',  ( 1.000000000000000000, -8.574039729943018344E-17, -0.000000000000000000 ) ) ;
#8564 = CARTESIAN_POINT ( 'NONE',  ( 10.37705096095362123, -12.86926679082229263, -1.500000000000000000 ) ) ;
#8563 = VECTOR ( 'NONE', #17486, 1000.000000000000114 ) ;
#8565 = EDGE_CURVE ( 'NONE', #11659, #10748, #9013, .T. ) ;
#8566 = CARTESIAN_POINT ( 'NONE',  ( -3.050050802731187449, -1.887961173149512062, -2.331437884370912261 ) ) ;
#8567 = LINE ( 'NONE', #18776, #30652 ) ;
#8568 = CIRCLE ( 'NONE', #27255, 4.000000000000000888 ) ;
#8569 = CARTESIAN_POINT ( 'NONE',  ( 24.73500000273118715, -2.486304738420683780, 0.2613211581691335383 ) ) ;
#8570 = CARTESIAN_POINT ( 'NONE',  ( 0.000000000000000000, 0.5000000000000000000, 0.000000000000000000 ) ) ;
#8571 = ADVANCED_FACE ( 'NONE', ( #7392 ), #4578, .F. ) ;
#8572 = CARTESIAN_POINT ( 'NONE',  ( 73.45519860863089434, -21.36028973287599086, 4.522129901861158707 ) ) ;
#8573 = CYLINDRICAL_SURFACE ( 'NONE', #22002, 6.248999999999999666 ) ;
#8574 = ORIENTED_EDGE ( 'NONE', *, *, #13233, .F. ) ;
#8575 = CARTESIAN_POINT ( 'NONE',  ( 7.249760686538667009, 3.647351267791679508, -7.953573330858177748 ) ) ;
#8576 = CIRCLE ( 'NONE', #23521, 0.5000000000000004441 ) ;
#8577 = AXIS2_PLACEMENT_3D ( 'NONE', #19842, #14961, #17833 ) ;
#8578 = CYLINDRICAL_SURFACE ( 'NONE', #15610, 8.749000000000002331 ) ;
#8579 = FACE_OUTER_BOUND ( 'NONE', #15091, .T. ) ;
#8580 = ORIENTED_EDGE ( 'NONE', *, *, #23315, .F. ) ;
#8581 = VECTOR ( 'NONE', #28695, 1000.000000000000114 ) ;
#8582 = B_SPLINE_CURVE_WITH_KNOTS ( 'NONE', 3,
 ( #5822, #23724, #663, #6163, #11162, #31573, #16348, #8830 ),
 .UNSPECIFIED., .F., .F.,
 ( 4, 2, 2, 4 ),
 ( 5.099451029780061619E-07, 0.001229189756360173818, 0.001843529661988771310, 0.002457869567617369452 ),
 .UNSPECIFIED. ) ;
#8583 = CONICAL_SURFACE ( 'NONE', #31557, 11.99878165403819352, 0.03490658503988666728 ) ;
#8584 = CARTESIAN_POINT ( 'NONE',  ( 25.45498872556016678, -2.391612775111189748, -1.307231450088218949 ) ) ;
#8585 = CARTESIAN_POINT ( 'NONE',  ( 21.36097421961354925, -21.76718868951427055, 1.410897148389129052 ) ) ;
#8586 = ORIENTED_EDGE ( 'NONE', *, *, #2080, .T. ) ;
#8587 = CARTESIAN_POINT ( 'NONE',  ( 0.9077343987014625526, -4.284037799451631656, -1.499999999999999334 ) ) ;
#8588 = ORIENTED_EDGE ( 'NONE', *, *, #21699, .F. ) ;
#8589 = AXIS2_PLACEMENT_3D ( 'NONE', #24767, #2035, #22411 ) ;
#8590 = VERTEX_POINT ( 'NONE', #14595 ) ;
#8591 = CARTESIAN_POINT ( 'NONE',  ( 24.79284380060802206, -17.49144841392629246, -1.371632250993898294 ) ) ;
#8593 = ORIENTED_EDGE ( 'NONE', *, *, #7417, .F. ) ;
#8592 = CARTESIAN_POINT ( 'NONE',  ( 35.00045521830035966, -0.01303574654798581554, -2.568038078148735526 ) ) ;
#8594 = ORIENTED_EDGE ( 'NONE', *, *, #20802, .F. ) ;
#8595 = CARTESIAN_POINT ( 'NONE',  ( 10.52034268205830614, 3.641590349731970822, -3.055657119358763829 ) ) ;
#8596 = EDGE_CURVE ( 'NONE', #780, #28781, #32709, .T. ) ;
#8597 = ORIENTED_EDGE ( 'NONE', *, *, #387, .T. ) ;
#8598 = CARTESIAN_POINT ( 'NONE',  ( 0.3749743454409040222, 2.260462012960326117, -9.839947797887550252 ) ) ;
#8600 = ORIENTED_EDGE ( 'NONE', *, *, #11511, .T. ) ;
#8599 = CARTESIAN_POINT ( 'NONE',  ( 19.00106589343955577, -3.165308183742087778, -1.169950778988538831 ) ) ;
#8601 = CARTESIAN_POINT ( 'NONE',  ( 21.73500000273118715, -2.486304738420683780, 0.2613211581691335383 ) ) ;
#8602 = DIRECTION ( 'NONE',  ( 0.000000000000000000, 1.000000000000000000, 0.000000000000000000 ) ) ;
#8603 = CIRCLE ( 'NONE', #7530, 0.4499999999999999001 ) ;
#8604 = CARTESIAN_POINT ( 'NONE',  ( 1.075551320669168476, 0.5000000000000000000, -7.404527507138929820 ) ) ;
#8605 = CARTESIAN_POINT ( 'NONE',  ( -9.560873106162357428E-17, -1.115095498423342990, 4.884328206559833241 ) ) ;
#8606 = AXIS2_PLACEMENT_3D ( 'NONE', #10594, #20798, #31004 ) ;
#8607 = CARTESIAN_POINT ( 'NONE',  ( 108.0280430118043142, -18.47317451037714164, 4.369308448245075915 ) ) ;
#8608 = VECTOR ( 'NONE', #25913, 999.9999999999998863 ) ;
#8609 = AXIS2_PLACEMENT_3D ( 'NONE', #16763, #29291, #6377 ) ;
#8610 = PLANE ( 'NONE',  #7493 ) ;
#8611 = CARTESIAN_POINT ( 'NONE',  ( -2.614103913510795962, -0.09422588260484983380, -1.555412231120104849 ) ) ;
#8612 = DIRECTION ( 'NONE',  ( -1.000000000000000000, 0.000000000000000000, 0.000000000000000000 ) ) ;
#8613 = DIRECTION ( 'NONE',  ( 0.000000000000000000, 0.000000000000000000, -1.000000000000000000 ) ) ;
#8614 = VECTOR ( 'NONE', #16075, 1000.000000000000000 ) ;
#8615 = AXIS2_PLACEMENT_3D ( 'NONE', #470, #10651, #28564 ) ;
#8616 = EDGE_CURVE ( 'NONE', #1245, #28881, #26814, .T. ) ;
#8617 = CARTESIAN_POINT ( 'NONE',  ( 7.249760686538667009, 7.953573330858214163, 3.647351267791597795 ) ) ;
#8618 = FACE_OUTER_BOUND ( 'NONE', #3722, .T. ) ;
#8619 = CARTESIAN_POINT ( 'NONE',  ( 24.23499999999999943, 0.2613211581691317065, 2.486304738420681559 ) ) ;
#8620 = CYLINDRICAL_SURFACE ( 'NONE', #14521, 0.4499999999999990119 ) ;
#8621 = DIRECTION ( 'NONE',  ( 0.000000000000000000, 0.000000000000000000, 1.000000000000000000 ) ) ;
#8622 = CARTESIAN_POINT ( 'NONE',  ( -4.962550801365593678, -2.228590825266444586, -2.752080473201636401 ) ) ;
#8623 = EDGE_LOOP ( 'NONE', ( #22761, #32188, #32094, #31803 ) ) ;
#8624 = CARTESIAN_POINT ( 'NONE',  ( -6.450050800000000528, -1.549418761218565477, 2.853674364686380471 ) ) ;
#8625 = VECTOR ( 'NONE', #5795, 1000.000000000000000 ) ;
#8626 = LINE ( 'NONE', #26673, #19418 ) ;
#8627 = CARTESIAN_POINT ( 'NONE',  ( 23.22564588060096469, -22.38932300456763969, 1.000000000000000000 ) ) ;
#8628 = CARTESIAN_POINT ( 'NONE',  ( 9.134478070117602044, -0.4075412269879192806, 1.500000000000000000 ) ) ;
#8629 = VERTEX_POINT ( 'NONE', #2226 ) ;
#8630 = CARTESIAN_POINT ( 'NONE',  ( 54.91409664899088483, -4.233361888145720009, -2.184956776138697876 ) ) ;
#8631 = EDGE_CURVE ( 'NONE', #2628, #28480, #31115, .T. ) ;
#8632 = VECTOR ( 'NONE', #16145, 1000.000000000000000 ) ;
#8633 = VECTOR ( 'NONE', #24598, 1000.000000000000000 ) ;
#8634 = CONICAL_SURFACE ( 'NONE', #1181, 10.97000000000001485, 0.1745329251994333364 ) ;
#8635 = VERTEX_POINT ( 'NONE', #1918 ) ;
#8636 = CARTESIAN_POINT ( 'NONE',  ( 0.2669397441535706350, -7.206081505926538178, 1.499999999999929390 ) ) ;
#8637 = ADVANCED_FACE ( 'NONE', ( #20124 ), #2064, .T. ) ;
#8638 = APPROVAL_STATUS ( 'not_yet_approved' ) ;
#8639 = CARTESIAN_POINT ( 'NONE',  ( 54.95788720335500699, -5.807879973348830660, 4.312042181588143563 ) ) ;
#8640 = AXIS2_PLACEMENT_3D ( 'NONE', #10163, #29440, #6705 ) ;
#8641 = CIRCLE ( 'NONE', #31618, 6.000000000000000888 ) ;
#8642 = DIRECTION ( 'NONE',  ( 3.623545766764168400E-17, 0.4226182617406938902, 0.9063077870366526012 ) ) ;
#8643 = DIRECTION ( 'NONE',  ( 1.000000000000000000, -8.574039729943018344E-17, -0.000000000000000000 ) ) ;
#8644 = CARTESIAN_POINT ( 'NONE',  ( 8.007433738499960540, 15.00000000000002132, 5.412820279296878923 ) ) ;
#8645 = EDGE_LOOP ( 'NONE', ( #4140, #11588, #30294, #28596 ) ) ;
#8646 = CARTESIAN_POINT ( 'NONE',  ( 18.60402535544292490, -7.603424548862588672, 0.07017451552782096036 ) ) ;
#8647 = CARTESIAN_POINT ( 'NONE',  ( 25.98173092684325880, 19.04622029248877269, -1.226162093883974125 ) ) ;
#8648 = CARTESIAN_POINT ( 'NONE',  ( -8.000050800000000351, 0.000000000000000000, -3.000000000000000444 ) ) ;
#8650 = EDGE_LOOP ( 'NONE', ( #5394, #16760, #31690, #28180 ) ) ;
#8649 = CARTESIAN_POINT ( 'NONE',  ( 0.000000000000000000, 37.67766952966368876, 0.000000000000000000 ) ) ;
#8651 = AXIS2_PLACEMENT_3D ( 'NONE', #31412, #26556, #8487 ) ;
#8652 = CARTESIAN_POINT ( 'NONE',  ( -3.862550801365593145, 3.521866450007987037, 0.3701630799359328372 ) ) ;
#8653 = AXIS2_PLACEMENT_3D ( 'NONE', #7424, #4265, #4944 ) ;
#8654 = DIRECTION ( 'NONE',  ( 0.000000000000000000, -1.000000000000000000, 0.000000000000000000 ) ) ;
#8655 = CARTESIAN_POINT ( 'NONE',  ( 2.598264985223430301, 0.000000000000000000, -5.684322216989628807 ) ) ;
#8656 = VECTOR ( 'NONE', #8458, 1000.000000000000000 ) ;
#8657 = EDGE_LOOP ( 'NONE', ( #23439, #15006, #891, #28063 ) ) ;
#8658 = AXIS2_PLACEMENT_3D ( 'NONE', #20497, #2447, #25335 ) ;
#8659 = VECTOR ( 'NONE', #18013, 1000.000000000000227 ) ;
#8660 = DIRECTION ( 'NONE',  ( 0.000000000000000000, 0.5877852522924689183, 0.8090169943749503378 ) ) ;
#8662 = AXIS2_PLACEMENT_3D ( 'NONE', #17846, #28046, #28358 ) ;
#8661 = CARTESIAN_POINT ( 'NONE',  ( 10.52034268205830259, 3.407865132560229604, -3.672404558090004212 ) ) ;
#8663 = CARTESIAN_POINT ( 'NONE',  ( -32.06740601709051930, 0.000000000000000000, -0.9045955023117262517 ) ) ;
#8664 = DIRECTION ( 'NONE',  ( 0.000000000000000000, 1.000000000000000000, 0.000000000000000000 ) ) ;
#8665 = CLOSED_SHELL ( 'NONE', ( #27434, #2624, #2261, #1945, #24011, #6892, #14143, #24472, #9747, #8038, #24909, #16781, #5086, #4727, #25621, #15928, #27626, #20218, #10308, #31341, #16582, #25484, #31403, #10915, #15420, #1163, #2542, #29694, #23982, #17333, #1136, #26943, #21217, #28797, #3250, #19395, #4922, #12368, #17404, #2715, #13817, #20814, #15953, #2003, #32585, #12173, #31013, #8553, #5617, #6989, #30865, #17191, #21203, #12084, #27558, #22941, #2112, #13802, #10459, #18795, #25877, #11028, #13630, #22879, #999, #31312, #14090, #798, #13875, #19775, #17724, #17774, #3624, #4672, #21599, #23855, #8530, #17207, #18396, #15283, #22938, #9959, #20808, #29384, #11720, #22342, #14471, #22668, #26312, #5612, #6770, #18997, #23658, #26181, #25445, #9528, #28967, #1071, #2369, #30256, #30445, #6675, #16910, #14965, #5644, #29006, #20657, #21080, #32583, #25006, #1193, #29312, #26370, #11922, #13167, #15842, #9218, #3216, #27487, #19605, #31446, #6322, #13026, #6463, #24142, #17150, #8397, #22631, #11319, #20240, #5763, #5315, #1974, #13658, #23476 ) ) ;
#8666 = CIRCLE ( 'NONE', #19906, 8.749000000000002331 ) ;
#8667 = DIRECTION ( 'NONE',  ( 0.000000000000000000, 0.000000000000000000, -1.000000000000000000 ) ) ;
#8668 = ORIENTED_EDGE ( 'NONE', *, *, #29780, .T. ) ;
#8669 = AXIS2_PLACEMENT_3D ( 'NONE', #29790, #27452, #17055 ) ;
#8670 = CARTESIAN_POINT ( 'NONE',  ( 6.356382228872878848, 2.398350474622056083, -8.265862592379898288 ) ) ;
#8671 = DIRECTION ( 'NONE',  ( 0.000000000000000000, 0.000000000000000000, 1.000000000000000000 ) ) ;
#8672 = CARTESIAN_POINT ( 'NONE',  ( -4.837550801365592790, 3.675193018007246959, -1.088641768524161391 ) ) ;
#8673 = CARTESIAN_POINT ( 'NONE',  ( 2.998015176062106768, -0.2419477797672031638, -1.432989973798650229 ) ) ;
#8674 = LINE ( 'NONE', #6173, #12462 ) ;
#8675 = ORIENTED_EDGE ( 'NONE', *, *, #15869, .T. ) ;
#8676 = ADVANCED_FACE ( 'NONE', ( #7243 ), #12090, .T. ) ;
#8677 = CARTESIAN_POINT ( 'NONE',  ( 3.063284526843530919, -7.360373001715506014, -4.729683950890343880 ) ) ;
#8678 = ADVANCED_FACE ( 'NONE', ( #14902 ), #32497, .T. ) ;
#8679 = AXIS2_PLACEMENT_3D ( 'NONE', #16029, #31132, #10541 ) ;
#8680 = ORIENTED_EDGE ( 'NONE', *, *, #20205, .F. ) ;
#8682 = AXIS2_PLACEMENT_3D ( 'NONE', #24073, #5867, #8872 ) ;
#8681 = DATE_AND_TIME ( #16363, #17275 ) ;
#8683 = CARTESIAN_POINT ( 'NONE',  ( 85.03574907444304642, -5.203687580104308985, 3.994701829074096544 ) ) ;
#8684 = AXIS2_PLACEMENT_3D ( 'NONE', #13515, #987, #490 ) ;
#8685 = CARTESIAN_POINT ( 'NONE',  ( 7.642108059735714498, -9.326698953827136762, -1.000000000000000000 ) ) ;
#8686 = VERTEX_POINT ( 'NONE', #4733 ) ;
#8687 = CARTESIAN_POINT ( 'NONE',  ( 0.1574692247322750649, -10.55579611470083279, 1.187839595764553335 ) ) ;
#8688 = ORIENTED_EDGE ( 'NONE', *, *, #26636, .F. ) ;
#8689 = ORIENTED_EDGE ( 'NONE', *, *, #3090, .T. ) ;
#8690 =( GEOMETRIC_REPRESENTATION_CONTEXT ( 3 ) GLOBAL_UNCERTAINTY_ASSIGNED_CONTEXT ( ( #2816 ) ) GLOBAL_UNIT_ASSIGNED_CONTEXT ( ( #25162, #5769, #10955 ) ) REPRESENTATION_CONTEXT ( 'NONE', 'WORKASPACE' ) );
#8691 = DIRECTION ( 'NONE',  ( 1.000000000000000000, -0.000000000000000000, 0.000000000000000000 ) ) ;
#8692 = CARTESIAN_POINT ( 'NONE',  ( -4.812550801365593323, 1.828967928396027398, -3.368539882008727115 ) ) ;
#8693 = CARTESIAN_POINT ( 'NONE',  ( 6.840024017557634117, -8.509480309817995192, 1.499999999999999778 ) ) ;
#8694 = AXIS2_PLACEMENT_3D ( 'NONE', #14264, #24459, #6757 ) ;
#8695 = CARTESIAN_POINT ( 'NONE',  ( 0.5438053540825241727, -6.200476582808712500, -1.499999999999999556 ) ) ;
#8697 = EDGE_LOOP ( 'NONE', ( #11474, #19122, #17865, #24315 ) ) ;
#8696 = CYLINDRICAL_SURFACE ( 'NONE', #3242, 11.00000000000000000 ) ;
#8698 = CARTESIAN_POINT ( 'NONE',  ( -5.587550801365593678, 3.521866450007987037, 0.3701630799359328372 ) ) ;
#8699 = CARTESIAN_POINT ( 'NONE',  ( 9.923352537987668143, 1.153138503447697749, 1.050000000000000044 ) ) ;
#8700 = CARTESIAN_POINT ( 'NONE',  ( 3.249999999999999556, 9.314797388894909602, -1.239665997526784746 ) ) ;
#8701 = CARTESIAN_POINT ( 'NONE',  ( -50.81000000000000227, -10.96999999999998643, 9.000000000000000000 ) ) ;
#8704 = EDGE_CURVE ( 'NONE', #22357, #8954, #12414, .T. ) ;
#8703 = VERTEX_POINT ( 'NONE', #25108 ) ;
#8702 = CARTESIAN_POINT ( 'NONE',  ( -56.77537022611499395, 0.4514244267945254907, 2.028141679927229379 ) ) ;
#8705 = B_SPLINE_CURVE_WITH_KNOTS ( 'NONE', 3,
 ( #10675, #15860, #21069, #13818, #23727, #1149, #26709, #16196 ),
 .UNSPECIFIED., .F., .F.,
 ( 4, 2, 2, 4 ),
 ( 0.000000000000000000, 0.5000000000000000000, 0.7500000000000000000, 1.000000000000000000 ),
 .UNSPECIFIED. ) ;
#8706 = AXIS2_PLACEMENT_3D ( 'NONE', #27687, #20034, #2300 ) ;
#8707 = VECTOR ( 'NONE', #21073, 1000.000000000000000 ) ;
#8708 = CARTESIAN_POINT ( 'NONE',  ( -28.62968855526470691, 6.563152521750583723, 2.075789994699551499 ) ) ;
#8709 = CARTESIAN_POINT ( 'NONE',  ( 20.61000000273118715, -1.573300977624594976, 1.942864903642425700 ) ) ;
#8710 = CIRCLE ( 'NONE', #6045, 301.6269746700523910 ) ;
#8711 = CARTESIAN_POINT ( 'NONE',  ( -21.88206647074803968, 4.362210445734582720, 1.500000000000000000 ) ) ;
#8712 = CIRCLE ( 'NONE', #9762, 8.750000000000000000 ) ;
#8713 = DIRECTION ( 'NONE',  ( 0.000000000000000000, -0.4226182617407076014, 0.9063077870366462729 ) ) ;
#8714 = CARTESIAN_POINT ( 'NONE',  ( -3.806083282599349804, -9.689094992912284710, -1.500000000000080158 ) ) ;
#8715 = EDGE_CURVE ( 'NONE', #29681, #32685, #26283, .T. ) ;
#8716 = DIRECTION ( 'NONE',  ( -1.000000000000000000, 0.000000000000000000, 1.388624693425302853E-14 ) ) ;
#8717 = APPROVAL_PERSON_ORGANIZATION ( #22596, #3324, #28246 ) ;
#8718 = CARTESIAN_POINT ( 'NONE',  ( -50.60000000000000142, -10.96966150227468972, 1.000000000000000000 ) ) ;
#8719 = CARTESIAN_POINT ( 'NONE',  ( -4.487550801365593145, -2.752080473201636845, 2.228590825266444586 ) ) ;
#8720 = ORIENTED_EDGE ( 'NONE', *, *, #25914, .T. ) ;
#8721 = ADVANCED_FACE ( 'NONE', ( #5229 ), #30674, .F. ) ;
#8722 = CARTESIAN_POINT ( 'NONE',  ( 20.74999999999999645, -1.779113243963175696E-15, 0.000000000000000000 ) ) ;
#8723 = EDGE_CURVE ( 'NONE', #15410, #11567, #6531, .T. ) ;
#8724 = CARTESIAN_POINT ( 'NONE',  ( 3.063284526839887167, 8.152713396088806519, -3.174628368995990879 ) ) ;
#8726 = CARTESIAN_POINT ( 'NONE',  ( 23.26681913458019224, -17.19558280316135779, 1.454198315410549336 ) ) ;
#8725 = DIRECTION ( 'NONE',  ( -1.000000000000000000, -0.000000000000000000, 0.000000000000000000 ) ) ;
#8727 = EDGE_LOOP ( 'NONE', ( #15346, #2549, #2911, #30119, #25131 ) ) ;
#8728 = AXIS2_PLACEMENT_3D ( 'NONE', #12756, #10266, #17967 ) ;
#8729 = CARTESIAN_POINT ( 'NONE',  ( 3.499999999999999556, 7.008469740302810891, -0.7425307242147067832 ) ) ;
#8730 = ORIENTED_EDGE ( 'NONE', *, *, #2801, .T. ) ;
#8731 =( BOUNDED_CURVE ( )  B_SPLINE_CURVE ( 2, ( #10391, #15054, #17917, #20599, #2544, #25272, #28443, #13204, #28257, #28108, #5206, #23406, #511, #10041, #20252, #15382, #7371, #20429, #25589, #12561, #22765, #5367, #32973, #12871, #23094, #7533, #17741, #15552, #22915, #10540, #27948, #365, #5055, #15232, #2700, #25435, #30807, #7875, #18067, #13062, #23263, #20751, #16372, #26581, #5843, #20908, #8365, #23567, #21239, #16028, #26256, #8852, #31437, #14026, #8218, #18417, #26734, #21575, #3851, #3682, #24050, #23897, #29250, #13842, #3373, #8692, #6334, #13538, #23749, #16523, #1355, #28608, #16220, #31781, #862, #18716, #6025, #24237, #5702, #21396, #1174, #31131, #11039, #28754, #3195, #31603, #10883, #18561, #15882, #8516, #19059, #3538, #26091, #13357, #28919, #26438, #691, #13695, #1006, #21091, #31292, #11189, #18907, #29100, #6187, #11374, #11529, #9499, #19556, #7186, #19714, #4339, #16710, #24731, #12033, #32286, #17019, #11859, #14518, #29754, #9000 ),
 .UNSPECIFIED., .F., .F. ) 
 B_SPLINE_CURVE_WITH_KNOTS ( ( 3, 2, 2, 2, 2, 2, 2, 2, 2, 2, 2, 2, 2, 2, 2, 2, 2, 2, 2, 2, 2, 2, 2, 2, 2, 2, 2, 2, 2, 2, 2, 2, 2, 2, 2, 2, 2, 2, 2, 2, 2, 2, 2, 2, 2, 2, 2, 2, 2, 2, 2, 2, 2, 2, 2, 2, 2, 2, 2, 2, 3 ),
 ( 0.009695607697749946546, 0.01562500000000000000, 0.03125000000000000000, 0.04687500000000000000, 0.06250000000000000000, 0.07812500000000001388, 0.09375000000000000000, 0.1093750000000000000, 0.1250000000000000000, 0.1406250000000000000, 0.1562500000000000000, 0.1718750000000000000, 0.1875000000000000000, 0.2031250000000000000, 0.2187500000000000000, 0.2343749999999999722, 0.2500000000000000000, 0.2656250000000000000, 0.2812500000000000000, 0.2968750000000000000, 0.3125000000000000000, 0.3281250000000000000, 0.3437500000000000000, 0.3593750000000000000, 0.3750000000000000000, 0.3906250000000000000, 0.4062500000000000000, 0.4218750000000000555, 0.4375000000000000000, 0.4531250000000000000, 0.4687500000000000000, 0.4843750000000000000, 0.4999999999999999445, 0.5156250000000000000, 0.5312500000000000000, 0.5468750000000000000, 0.5625000000000000000, 0.5781250000000000000, 0.5937500000000000000, 0.6093750000000000000, 0.6250000000000000000, 0.6406250000000000000, 0.6562500000000000000, 0.6718750000000000000, 0.6875000000000000000, 0.7031250000000000000, 0.7187500000000000000, 0.7343750000000000000, 0.7500000000000000000, 0.7656250000000000000, 0.7812500000000000000, 0.7968750000000000000, 0.8125000000000000000, 0.8281250000000000000, 0.8437500000000000000, 0.8593750000000000000, 0.8750000000000000000, 0.8906250000000001110, 0.9062500000000000000, 0.9218750000000000000, 0.9278186525000968743 ),
 .UNSPECIFIED. ) 
 CURVE ( )  GEOMETRIC_REPRESENTATION_ITEM ( )  RATIONAL_B_SPLINE_CURVE ( ( 0.9641510359188718571, 0.9711137207058399001, 1.000000000000000000, 0.9238795325112867385, 1.000000000000000000, 0.9238795325112867385, 1.000000000000000000, 0.9238795325112867385, 1.000000000000000000, 0.9238795325112867385, 1.000000000000000000, 0.9238795325112867385, 1.000000000000000000, 0.9238795325112867385, 1.000000000000000000, 0.9238795325112867385, 1.000000000000000000, 0.9238795325112867385, 1.000000000000000000, 0.9238795325112867385, 1.000000000000000000, 0.9238795325112867385, 1.000000000000000000, 0.9238795325112867385, 1.000000000000000000, 0.9238795325112867385, 1.000000000000000000, 0.9238795325112867385, 1.000000000000000000, 0.9238795325112867385, 1.000000000000000000, 0.9238795325112867385, 1.000000000000000000, 0.9238795325112867385, 1.000000000000000000, 0.9238795325112867385, 1.000000000000000000, 0.9238795325112867385, 1.000000000000000000, 0.9238795325112867385, 1.000000000000000000, 0.9238795325112867385, 1.000000000000000000, 0.9238795325112867385, 1.000000000000000000, 0.9238795325112867385, 1.000000000000000000, 0.9238795325112867385, 1.000000000000000000, 0.9238795325112867385, 1.000000000000000000, 0.9238795325112867385, 1.000000000000000000, 0.9238795325112867385, 1.000000000000000000, 0.9238795325112867385, 1.000000000000000000, 0.9238795325112867385, 1.000000000000000000, 0.9238795325112867385, 1.000000000000000000, 0.9238795325112867385, 1.000000000000000000, 0.9238795325112867385, 1.000000000000000000, 0.9238795325112867385, 1.000000000000000000, 0.9238795325112867385, 1.000000000000000000, 0.9238795325112867385, 1.000000000000000000, 0.9238795325112867385, 1.000000000000000000, 0.9238795325112867385, 1.000000000000000000, 0.9238795325112867385, 1.000000000000000000, 0.9238795325112867385, 1.000000000000000000, 0.9238795325112867385, 1.000000000000000000, 0.9238795325112867385, 1.000000000000000000, 0.9238795325112867385, 1.000000000000000000, 0.9238795325112867385, 1.000000000000000000, 0.9238795325112867385, 1.000000000000000000, 0.9238795325112867385, 1.000000000000000000, 0.9238795325112867385, 1.000000000000000000, 0.9238795325112867385, 1.000000000000000000, 0.9238795325112867385, 1.000000000000000000, 0.9238795325112867385, 1.000000000000000000, 0.9238795325112867385, 1.000000000000000000, 0.9238795325112867385, 1.000000000000000000, 0.9238795325112867385, 1.000000000000000000, 0.9238795325112867385, 1.000000000000000000, 0.9238795325112867385, 1.000000000000000000, 0.9238795325112867385, 1.000000000000000000, 0.9238795325112867385, 1.000000000000000000, 0.9238795325112867385, 1.000000000000000000, 0.9238795325112867385, 1.000000000000000000, 0.9238795325112867385, 1.000000000000000000, 0.9710442491585387081, 0.9641176721898496726 ) ) 
 REPRESENTATION_ITEM ( '' )  );
#8732 = DIRECTION ( 'NONE',  ( -1.000000000000000000, -0.000000000000000000, -0.000000000000000000 ) ) ;
#8734 = ORIENTED_EDGE ( 'NONE', *, *, #19166, .T. ) ;
#8733 = CARTESIAN_POINT ( 'NONE',  ( 17.75999999999999801, -2.208672634433321348E-15, 0.000000000000000000 ) ) ;
#8735 = ADVANCED_FACE ( 'NONE', ( #30975 ), #25224, .T. ) ;
#8736 = VERTEX_POINT ( 'NONE', #28130 ) ;
#8737 = CARTESIAN_POINT ( 'NONE',  ( -8.000050800000000351, 2.857870525728205990, -2.169999637890065003 ) ) ;
#8738 = CIRCLE ( 'NONE', #5034, 10.94895958125474245 ) ;
#8739 = AXIS2_PLACEMENT_3D ( 'NONE', #8285, #10286, #31022 ) ;
#8740 = CARTESIAN_POINT ( 'NONE',  ( -5.762942409646513831, 3.284080845023683730E-15, 3.000000000000000000 ) ) ;
#8742 = EDGE_LOOP ( 'NONE', ( #12504, #5922, #18481, #343 ) ) ;
#8741 = CARTESIAN_POINT ( 'NONE',  ( 18.96091535642496240, -3.614110606601101949, 2.184956778829998836 ) ) ;
#8743 = DIRECTION ( 'NONE',  ( 0.000000000000000000, -0.2588190451025286221, 0.9659258262890662028 ) ) ;
#8744 = CARTESIAN_POINT ( 'NONE',  ( 10.00000000000000178, -8.574039729943018837E-16, 0.000000000000000000 ) ) ;
#8745 = EDGE_CURVE ( 'NONE', #17772, #26254, #10283, .T. ) ;
#8746 = CARTESIAN_POINT ( 'NONE',  ( 108.0371116761128576, -18.60376102042065938, -4.091500227421209779 ) ) ;
#8747 = SECURITY_CLASSIFICATION ( '', '', #7135 ) ;
#8748 = CARTESIAN_POINT ( 'NONE',  ( 7.362531900907011817, -8.542914936921272684, -1.000000000000000000 ) ) ;
#8749 = DIRECTION ( 'NONE',  ( -1.000000000000000000, 0.000000000000000000, 0.000000000000000000 ) ) ;
#8750 = DIRECTION ( 'NONE',  ( -1.000000000000000000, 0.000000000000000000, 0.000000000000000000 ) ) ;
#8751 = EDGE_CURVE ( 'NONE', #22534, #21729, #10234, .T. ) ;
#8752 = CARTESIAN_POINT ( 'NONE',  ( -2.037945749704337831E-16, -2.376879293651093406, 4.116875700062075261 ) ) ;
#8753 = CARTESIAN_POINT ( 'NONE',  ( 29.22961111230291209, -6.951722887056884126, 3.390608046102742801 ) ) ;
#8754 = CARTESIAN_POINT ( 'NONE',  ( -2.786590204610738475, -5.640011313470055576, 4.522129901861158707 ) ) ;
#8755 = DIRECTION ( 'NONE',  ( -3.623545766764323707E-17, -0.4226182617407121533, 0.9063077870366440525 ) ) ;
#8756 = VECTOR ( 'NONE', #14164, 1000.000000000000000 ) ;
#8757 = VERTEX_POINT ( 'NONE', #2726 ) ;
#8758 = DIRECTION ( 'NONE',  ( 1.000000000000000000, 0.000000000000000000, 0.000000000000000000 ) ) ;
#8759 = EDGE_CURVE ( 'NONE', #8809, #10694, #20623, .T. ) ;
#8760 = EDGE_CURVE ( 'NONE', #866, #3400, #13229, .T. ) ;
#8761 = DIRECTION ( 'NONE',  ( -1.000000000000000000, 0.000000000000000000, 0.000000000000000000 ) ) ;
#8762 = ORIENTED_EDGE ( 'NONE', *, *, #23507, .T. ) ;
#8763 = CARTESIAN_POINT ( 'NONE',  ( 25.35555344407661593, -2.327875542983621315, 1.215979502681800328 ) ) ;
#8764 = CARTESIAN_POINT ( 'NONE',  ( 16.36487458112949511, 19.37645981759117575, -4.612695725900422872 ) ) ;
#8765 = SECURITY_CLASSIFICATION ( '', '', #23481 ) ;
#8766 = ORIENTED_EDGE ( 'NONE', *, *, #10067, .F. ) ;
#8767 = CARTESIAN_POINT ( 'NONE',  ( 17.32050807568873552, 10.00000000000002309, -1.491740999229417941 ) ) ;
#8768 = CARTESIAN_POINT ( 'NONE',  ( 0.2099999999999983824, 0.0003384977253079179960, -2.168404344971008868E-16 ) ) ;
#8769 = ORIENTED_EDGE ( 'NONE', *, *, #20666, .F. ) ;
#8770 = ORIENTED_EDGE ( 'NONE', *, *, #2240, .F. ) ;
#8771 = LINE ( 'NONE', #29163, #3866 ) ;
#8772 = DATE_AND_TIME ( #11271, #13044 ) ;
#8774 = ORIENTED_EDGE ( 'NONE', *, *, #3502, .T. ) ;
#8773 = CARTESIAN_POINT ( 'NONE',  ( -0.2168228499960635214, -15.24168959957554215, -0.9788672205760856615 ) ) ;
#8775 = ORIENTED_EDGE ( 'NONE', *, *, #25981, .T. ) ;
#8776 = CARTESIAN_POINT ( 'NONE',  ( 25.54750000136559507, 3.024605502323846729, -0.3178988483021056854 ) ) ;
#8777 = EDGE_CURVE ( 'NONE', #12277, #19429, #48, .T. ) ;
#8778 = VERTEX_POINT ( 'NONE', #20458 ) ;
#8779 = CARTESIAN_POINT ( 'NONE',  ( -2.819379691724115400, -6.927609664242504017, 4.522129901861158707 ) ) ;
#8780 = LINE ( 'NONE', #29171, #3795 ) ;
#8781 = VECTOR ( 'NONE', #33054, 1000.000000000000000 ) ;
#8783 = ORIENTED_EDGE ( 'NONE', *, *, #16072, .T. ) ;
#8782 = CARTESIAN_POINT ( 'NONE',  ( 4.749760686538667009, -5.151476664237518044, 6.139290821770238438 ) ) ;
#8784 = CYLINDRICAL_SURFACE ( 'NONE', #17231, 0.5000000000000004441 ) ;
#8785 = CARTESIAN_POINT ( 'NONE',  ( 7.249760686538667009, -0.7071067811865734409, 8.721381771256202953 ) ) ;
#8786 = CARTESIAN_POINT ( 'NONE',  ( -56.77633738153843979, 0.4614026863384942390, 1.995096760105839362 ) ) ;
#8787 = CARTESIAN_POINT ( 'NONE',  ( 0.7632845268398872340, -2.223716399045631231, 8.461683424509299556 ) ) ;
#8788 = CARTESIAN_POINT ( 'NONE',  ( 107.5619444582182354, -18.98608621969496113, 4.515334266560267373 ) ) ;
#8789 = CARTESIAN_POINT ( 'NONE',  ( 10.00000000000000178, -2.285372942704923638, -4.458382051008218383 ) ) ;
#8790 = CARTESIAN_POINT ( 'NONE',  ( 18.60860417056578342, -7.552242585353035054, -0.8105616806102179384 ) ) ;
#8791 = DIRECTION ( 'NONE',  ( 1.000000000000000000, 0.000000000000000000, 0.000000000000000000 ) ) ;
#8792 = LINE ( 'NONE', #3620, #12350 ) ;
#8793 = CARTESIAN_POINT ( 'NONE',  ( 3.249999999999999556, 6.807171995660584507, 6.478011392632914145 ) ) ;
#8794 = CARTESIAN_POINT ( 'NONE',  ( 108.3721138249345728, 20.25023653045810690, -2.520993486554220286 ) ) ;
#8795 = CARTESIAN_POINT ( 'NONE',  ( 25.75999999999999801, -2.208672634433321348E-15, 0.000000000000000000 ) ) ;
#8796 = EDGE_CURVE ( 'NONE', #16327, #22347, #7750, .T. ) ;
#8797 = FACE_OUTER_BOUND ( 'NONE', #30289, .T. ) ;
#8798 = EDGE_CURVE ( 'NONE', #15271, #14502, #23428, .T. ) ;
#8799 = CARTESIAN_POINT ( 'NONE',  ( -3.262550801365593056, 0.3701630799359330593, -3.521866450007987037 ) ) ;
#8800 = ORIENTED_EDGE ( 'NONE', *, *, #21033, .F. ) ;
#8801 = CARTESIAN_POINT ( 'NONE',  ( -5.350050800000001772, -0.9222479816126459840, -3.113457007523259268 ) ) ;
#8802 =( BOUNDED_CURVE ( )  B_SPLINE_CURVE ( 2, ( #21762, #31971, #21440, #21612, #3419, #6073, #8556, #19257, #8406, #5887, #8740 ),
 .UNSPECIFIED., .F., .F. ) 
 B_SPLINE_CURVE_WITH_KNOTS ( ( 3, 2, 2, 2, 2, 3 ),
 ( 0.2478822619934377414, 0.2500000000000000000, 0.2656250000000000000, 0.2812500000000000000, 0.2968750000000000000, 0.3103822619934377136 ),
 .UNSPECIFIED. ) 
 CURVE ( )  GEOMETRIC_REPRESENTATION_ITEM ( )  RATIONAL_B_SPLINE_CURVE ( ( 0.9821626249036861100, 0.9896829947469993893, 1.000000000000000000, 0.9238795325112867385, 1.000000000000000000, 0.9238795325112867385, 1.000000000000000000, 0.9238795325112867385, 1.000000000000000000, 0.9341965377642874602, 0.9821626249036857770 ) ) 
 REPRESENTATION_ITEM ( '' )  );
#8803 = VECTOR ( 'NONE', #6200, 1000.000000000000000 ) ;
#8804 = CARTESIAN_POINT ( 'NONE',  ( 7.577572045913208321, 15.00000000000002132, -4.612695725900422872 ) ) ;
#8805 = DIRECTION ( 'NONE',  ( 0.000000000000000000, 0.000000000000000000, -1.000000000000000000 ) ) ;
#8806 = CARTESIAN_POINT ( 'NONE',  ( 8.305304940806680136, -2.146676032412352164, 1.000000000000000000 ) ) ;
#8807 = ORIENTED_EDGE ( 'NONE', *, *, #2022, .T. ) ;
#8808 = CARTESIAN_POINT ( 'NONE',  ( 3.499999999999999556, 0.000000000000000000, 0.000000000000000000 ) ) ;
#8809 = VERTEX_POINT ( 'NONE', #10413 ) ;
#8810 = CARTESIAN_POINT ( 'NONE',  ( 0.8635714481620181404, -8.446712017869664635, 1.500000000000000000 ) ) ;
#8811 = APPROVAL_ROLE ( '' ) ;
#8812 = CARTESIAN_POINT ( 'NONE',  ( 40.88222826846868685, -6.571667082204984744, 4.275175681024973251 ) ) ;
#8813 = EDGE_CURVE ( 'NONE', #29082, #23972, #7896, .T. ) ;
#8814 = CC_DESIGN_PERSON_AND_ORGANIZATION_ASSIGNMENT ( #1120, #16165, ( #1293 ) ) ;
#8815 = CARTESIAN_POINT ( 'NONE',  ( 22.75143042797981252, 17.32866418988431079, -1.049999999999999822 ) ) ;
#8816 = CARTESIAN_POINT ( 'NONE',  ( 102.3595522875182837, -3.079674301831176741, -4.215290384261815682 ) ) ;
#8817 = CARTESIAN_POINT ( 'NONE',  ( 23.30536738591935730, -17.34558290870676700, -1.520589546895734001 ) ) ;
#8818 = CARTESIAN_POINT ( 'NONE',  ( 107.8806307222008627, -16.35047421165092985, 3.636029349014985090 ) ) ;
#8819 = VERTEX_POINT ( 'NONE', #28281 ) ;
#8820 = CARTESIAN_POINT ( 'NONE',  ( -2.986084103915760846, 1.331507122045496354E-29, 1.110774563390631409 ) ) ;
#8821 = DIRECTION ( 'NONE',  ( 1.000000000000000000, -0.000000000000000000, -0.000000000000000000 ) ) ;
#8822 = CARTESIAN_POINT ( 'NONE',  ( 2.274274201625327230, 0.000000000000000000, 0.000000000000000000 ) ) ;
#8824 = ORIENTED_EDGE ( 'NONE', *, *, #7059, .T. ) ;
#8823 = DIRECTION ( 'NONE',  ( 0.000000000000000000, 0.5735764363510378328, 0.8191520442889975717 ) ) ;
#8825 = CARTESIAN_POINT ( 'NONE',  ( -23.54713438637982748, 12.65740340961132304, 3.359978791489319772 ) ) ;
#8826 = DIRECTION ( 'NONE',  ( -0.000000000000000000, -0.000000000000000000, -1.000000000000000000 ) ) ;
#8827 = CARTESIAN_POINT ( 'NONE',  ( 108.5974656045667075, 15.84760961618085062, 1.739510335802044727 ) ) ;
#8828 = EDGE_CURVE ( 'NONE', #12125, #9954, #17234, .T. ) ;
#8829 = LINE ( 'NONE', #16347, #28943 ) ;
#8830 = CARTESIAN_POINT ( 'NONE',  ( 0.7632845268398871230, -3.174628368996133876, 8.152713396088751452 ) ) ;
#8831 = DIRECTION ( 'NONE',  ( 0.000000000000000000, 0.9961946980917454342, 0.08715574274765873486 ) ) ;
#8832 = CARTESIAN_POINT ( 'NONE',  ( -0.5220033361344453837, 0.000000000000000000, 5.485967528433935314 ) ) ;
#8833 = EDGE_CURVE ( 'NONE', #3232, #9843, #13086, .T. ) ;
#8834 = CARTESIAN_POINT ( 'NONE',  ( 25.29725835852283922, -17.51800646107394854, 1.124426024579843642 ) ) ;
#8835 = ORIENTED_EDGE ( 'NONE', *, *, #12000, .T. ) ;
#8836 = CARTESIAN_POINT ( 'NONE',  ( 25.52557118915447631, -17.56218954043520597, -1.078818547980193943 ) ) ;
#8837 = CARTESIAN_POINT ( 'NONE',  ( -2.069657272239051160, 1.153746456547815269, 3.257691561679774139 ) ) ;
#8838 = CARTESIAN_POINT ( 'NONE',  ( -2.737550801365594033, -3.368539882008727115, -1.828967928396027842 ) ) ;
#8839 = CARTESIAN_POINT ( 'NONE',  ( 107.5817932186935622, -17.35116855567646965, -4.522076874643048860 ) ) ;
#8840 = DIRECTION ( 'NONE',  ( 0.04852105321274754329, -0.4695180821586618092, 0.8815886103626667802 ) ) ;
#8841 = ORIENTED_EDGE ( 'NONE', *, *, #21254, .T. ) ;
#8842 = PLANE ( 'NONE',  #22012 ) ;
#8843 = ORIENTED_EDGE ( 'NONE', *, *, #8186, .T. ) ;
#8844 = COORDINATED_UNIVERSAL_TIME_OFFSET ( 0, 0, .AHEAD. ) ;
#8845 = CARTESIAN_POINT ( 'NONE',  ( 7.249760686538667009, 0.000000000000000000, 5.500000000000000000 ) ) ;
#8846 = CARTESIAN_POINT ( 'NONE',  ( -3.500050802731187627, 2.853674364686379583, 1.549418761218565921 ) ) ;
#8847 = ORIENTED_EDGE ( 'NONE', *, *, #10830, .F. ) ;
#8848 = CARTESIAN_POINT ( 'NONE',  ( -50.81000000000000227, -10.96999999999998643, 5.700000000000000178 ) ) ;
#8849 = ORIENTED_EDGE ( 'NONE', *, *, #7544, .T. ) ;
#8850 = ORIENTED_EDGE ( 'NONE', *, *, #5258, .F. ) ;
#8851 = DIRECTION ( 'NONE',  ( 1.000000000000000000, 0.000000000000000000, 0.000000000000000000 ) ) ;
#8852 = CARTESIAN_POINT ( 'NONE',  ( -5.512550801365594388, 3.675193018007246959, -1.088641768524161391 ) ) ;
#8853 = CARTESIAN_POINT ( 'NONE',  ( 22.17249999999999943, 1.291182301015469047, 2.378061970571981654 ) ) ;
#8854 = CARTESIAN_POINT ( 'NONE',  ( 0.5134311721232786008, -4.169659756541258311, -1.765416748134584157 ) ) ;
#8856 = EDGE_LOOP ( 'NONE', ( #32668, #30291, #28183, #20874, #10876 ) ) ;
#8855 = CARTESIAN_POINT ( 'NONE',  ( 0.000000000000000000, 7.008469740302810891, -0.7425307242147067832 ) ) ;
#8857 = CARTESIAN_POINT ( 'NONE',  ( -7.537550801365592967, -3.368539882008727115, -1.828967928396028064 ) ) ;
#8858 = CARTESIAN_POINT ( 'NONE',  ( 101.8797206818347973, -5.166491396334524033, 2.184956718991889257 ) ) ;
#8859 = CARTESIAN_POINT ( 'NONE',  ( 10.35374396645284989, -19.59145211855898339, 1.750308502512231579 ) ) ;
#8860 = CARTESIAN_POINT ( 'NONE',  ( 3.250000000000001332, 1.102182119233145856E-15, 7.000000000000000888 ) ) ;
#8861 = ORIENTED_EDGE ( 'NONE', *, *, #1519, .F. ) ;
#8862 = ADVANCED_FACE ( 'NONE', ( #12583 ), #14546, .F. ) ;
#8864 = VERTEX_POINT ( 'NONE', #27974 ) ;
#8863 = DIRECTION ( 'NONE',  ( 0.000000000000000000, 0.9961946980917448791, 0.08715574274766618723 ) ) ;
#8865 = ADVANCED_FACE ( 'NONE', ( #15581 ), #22029, .T. ) ;
#8866 = EDGE_CURVE ( 'NONE', #25021, #21409, #2924, .T. ) ;
#8867 = CARTESIAN_POINT ( 'NONE',  ( 23.29750000273119070, 2.594547506269380133, 0.7685399846772031918 ) ) ;
#8868 = CARTESIAN_POINT ( 'NONE',  ( 6.883866482134012976, -0.8319830743950079599, -8.691827696555167293 ) ) ;
#8869 = CYLINDRICAL_SURFACE ( 'NONE', #15015, 6.248999999999999666 ) ;
#8870 = CARTESIAN_POINT ( 'NONE',  ( -3.910130424047638442, -3.305169137730107121, -1.500000000000157652 ) ) ;
#8871 = DIRECTION ( 'NONE',  ( 0.000000000000000000, 0.000000000000000000, 1.000000000000000000 ) ) ;
#8872 = DIRECTION ( 'NONE',  ( 0.000000000000000000, 0.000000000000000000, -1.000000000000000000 ) ) ;
#8873 = CARTESIAN_POINT ( 'NONE',  ( 7.249760686538667009, 8.466096581343512284, -2.210816291636124475 ) ) ;
#8874 = ORIENTED_EDGE ( 'NONE', *, *, #18015, .F. ) ;
#8875 = DIRECTION ( 'NONE',  ( -1.000000000000000000, 8.574039729943017111E-17, -0.000000000000000000 ) ) ;
#8876 = CARTESIAN_POINT ( 'NONE',  ( 5.377543748152548986, 7.892520144992453801, -1.391664247347147443 ) ) ;
#8878 = CARTESIAN_POINT ( 'NONE',  ( 107.4492989043458664, -17.34924253231580593, 4.492206751594263636 ) ) ;
#8877 = PLANE ( 'NONE',  #2777 ) ;
#8879 = VERTEX_POINT ( 'NONE', #26757 ) ;
#8880 = CARTESIAN_POINT ( 'NONE',  ( -4.800050800000000173, -2.331437884370912705, 1.887961173149512062 ) ) ;
#8881 = VERTEX_POINT ( 'NONE', #8389 ) ;
#8882 = DIRECTION ( 'NONE',  ( 0.000000000000000000, 0.9945218953682729568, 0.1045284632676571068 ) ) ;
#8884 = EDGE_LOOP ( 'NONE', ( #9832, #10329, #7139, #11497 ) ) ;
#8883 = CARTESIAN_POINT ( 'NONE',  ( 102.3443137184323177, -2.859699058333353694, -4.001040673967360739 ) ) ;
#8885 = VERTEX_POINT ( 'NONE', #21259 ) ;
#8886 = CARTESIAN_POINT ( 'NONE',  ( 29.25343337322282622, -7.426690278353109242, -4.522129901861164036 ) ) ;
#8887 = DIRECTION ( 'NONE',  ( -0.000000000000000000, -0.3746065934159164001, 0.9271838545667856479 ) ) ;
#8888 = EDGE_CURVE ( 'NONE', #6067, #18014, #11585, .T. ) ;
#8890 = ORIENTED_EDGE ( 'NONE', *, *, #21763, .T. ) ;
#8889 = CARTESIAN_POINT ( 'NONE',  ( 11.59716086141860458, -20.31972538710700960, -1.499999999999999334 ) ) ;
#8891 = CARTESIAN_POINT ( 'NONE',  ( 17.20462742525712585, 13.34747051462077927, -1.500000000000000000 ) ) ;
#8892 = CARTESIAN_POINT ( 'NONE',  ( 3.063284526839887167, 2.223716399045691183, -8.461683424509292450 ) ) ;
#8893 = CARTESIAN_POINT ( 'NONE',  ( 108.1227634682907848, -19.83712552029795617, -1.563595750885480085 ) ) ;
#8894 = CARTESIAN_POINT ( 'NONE',  ( 10.11068946041623740, -12.10067465432455869, -1.499999999999573896 ) ) ;
#8896 = ORIENTED_EDGE ( 'NONE', *, *, #23066, .T. ) ;
#8895 = CARTESIAN_POINT ( 'NONE',  ( 107.8874544901744912, -16.44873477293144859, -1.585822557233536934 ) ) ;
#8897 = CARTESIAN_POINT ( 'NONE',  ( 10.57125986779756843, -4.884328206559830576, -1.115095498423360310 ) ) ;
#8898 = DIRECTION ( 'NONE',  ( -0.000000000000000000, -0.000000000000000000, -1.000000000000000000 ) ) ;
#8899 = DIRECTION ( 'NONE',  ( 0.000000000000000000, 0.000000000000000000, -1.000000000000000000 ) ) ;
#8900 = UNCERTAINTY_MEASURE_WITH_UNIT (LENGTH_MEASURE( 1.000000000000000082E-05 ), #18799, 'distance_accuracy_value', 'NONE');
#8901 = CARTESIAN_POINT ( 'NONE',  ( -2.600000000000000089, 0.000000000000000000, 1.500000000000000000 ) ) ;
#8902 = DIRECTION ( 'NONE',  ( 0.000000000000000000, -0.5877852522924797984, 0.8090169943749425663 ) ) ;
#8903 = ORIENTED_EDGE ( 'NONE', *, *, #11976, .F. ) ;
#8904 = DIRECTION ( 'NONE',  ( 3.623545766764192436E-17, 0.4226182617406968878, 0.9063077870366511579 ) ) ;
#8905 = CARTESIAN_POINT ( 'NONE',  ( 107.4085326904115334, -16.76255377593236418, -3.296787005979242124 ) ) ;
#8906 = CARTESIAN_POINT ( 'NONE',  ( -12.44989959798873791, 18.00000000000000355, -0.3702070605508915868 ) ) ;
#8907 = EDGE_LOOP ( 'NONE', ( #22458, #7027, #17259, #1267 ) ) ;
#8908 =( BOUNDED_SURFACE ( )  B_SPLINE_SURFACE ( 3, 2, ( 
 ( #21499, #31524, #11462 ),
 ( #31709, #3470, #21809 ),
 ( #21319, #13627, #16451 ),
 ( #13936, #18992, #6122 ),
 ( #24158, #1281, #8788 ),
 ( #29180, #21657, #31864 ),
 ( #11613, #23977, #23830 ),
 ( #8933, #3616, #19139 ),
 ( #6421, #29329, #31372 ),
 ( #8607, #1095, #942 ),
 ( #8450, #16619, #26834 ),
 ( #16137, #11120, #18644 ),
 ( #28841, #5938, #26362 ),
 ( #12472, #15910, #395 ),
 ( #17631, #8395, #10731 ),
 ( #5587, #8062, #14950 ),
 ( #18591, #13386, #23436 ),
 ( #31465, #25164, #20166 ),
 ( #26121, #13093, #5732 ),
 ( #3226, #23606, #890 ),
 ( #17474, #23292, #5875 ),
 ( #18266, #15767, #27673 ),
 ( #21266, #28288, #28479 ),
 ( #10572, #2285, #726 ),
 ( #10914, #25972, #28780 ),
 ( #22683, #4775, #30364 ),
 ( #26295, #3080, #3405 ),
 ( #21121, #31319, #32886 ),
 ( #7433, #30982, #20945 ),
 ( #13236, #16062, #20779 ),
 ( #9953, #542, #13568 ),
 ( #15593, #25807, #31163 ),
 ( #8251, #18444, #23775 ),
 ( #11066, #5400, #2931 ),
 ( #28636, #14061, #19436 ),
 ( #32132, #13724, #18750 ),
 ( #9208, #18937, #28960 ),
 ( #3710, #26608, #8878 ) ),
 .UNSPECIFIED., .F., .F., .F. ) 
 B_SPLINE_SURFACE_WITH_KNOTS ( ( 4, 2, 2, 2, 2, 2, 2, 2, 2, 2, 2, 2, 2, 2, 2, 2, 2, 2, 4 ),
 ( 3, 3 ),
 ( 0.007231348716683458529, 0.007247137925435321107, 0.007262927134187182818, 0.007270821738563113673, 0.007278716342939045396, 0.007294505551690907974, 0.007357662386698358287, 0.007483976056713257177, 0.007610289726728156068, 0.007736603396743054958, 0.007862917066757953849, 0.007989230736772852740, 0.008115544406787751630, 0.008178701241795201943, 0.008194490450547063654, 0.008210279659298925364, 0.008218174263674856220, 0.008226068868050787075, 0.008241858076802650521 ),
 ( 0.000000000000000000, 1.000000000000000000 ),
 .UNSPECIFIED. ) 
 GEOMETRIC_REPRESENTATION_ITEM ( )  RATIONAL_B_SPLINE_SURFACE ( (
 ( 1.000000000000000000, 0.7067447072241932471, 1.000000000000000000),
 ( 1.000000000000000000, 0.7067447061585132584, 1.000000000000000000),
 ( 1.000000000000000000, 0.7067447050979218659, 1.000000000000000000),
 ( 1.000000000000000000, 0.7067447029864426522, 1.000000000000000000),
 ( 1.000000000000000000, 0.7067442384298668889, 1.000000000000000000),
 ( 1.000000000000000000, 0.7067449321202956547, 1.000000000000000000),
 ( 1.000000000000000000, 0.7067458649492553979, 1.000000000000000000),
 ( 1.000000000000000000, 0.7067471220154400990, 1.000000000000000000),
 ( 1.000000000000000000, 0.7067477637805932300, 1.000000000000000000),
 ( 1.000000000000000000, 0.7067497297540578094, 1.000000000000000000),
 ( 1.000000000000000000, 0.7067510945828608948, 1.000000000000000000),
 ( 1.000000000000000000, 0.7067582039293559548, 1.000000000000000000),
 ( 1.000000000000000000, 0.7067647927017992604, 1.000000000000000000),
 ( 1.000000000000000000, 0.7067880497366301196, 1.000000000000000000),
 ( 1.000000000000000000, 0.7068082938633269974, 1.000000000000000000),
 ( 1.000000000000000000, 0.7068628506264388323, 1.000000000000000000),
 ( 1.000000000000000000, 0.7068980583899157066, 1.000000000000000000),
 ( 1.000000000000000000, 0.7069883395600154996, 1.000000000000000000),
 ( 1.000000000000000000, 0.7070467650740049903, 1.000000000000000000),
 ( 1.000000000000000000, 0.7071655611593249402, 1.000000000000000000),
 ( 1.000000000000000000, 0.7072232875170134658, 1.000000000000000000),
 ( 1.000000000000000000, 0.7073145313144446611, 1.000000000000000000),
 ( 1.000000000000000000, 0.7073497553658054660, 1.000000000000000000),
 ( 1.000000000000000000, 0.7074042560665476653, 1.000000000000000000),
 ( 1.000000000000000000, 0.7074245345453707978, 1.000000000000000000),
 ( 1.000000000000000000, 0.7074478136499360303, 1.000000000000000000),
 ( 1.000000000000000000, 0.7074544300748824011, 1.000000000000000000),
 ( 1.000000000000000000, 0.7074615795605810886, 1.000000000000000000),
 ( 1.000000000000000000, 0.7074629527376177229, 1.000000000000000000),
 ( 1.000000000000000000, 0.7074655910163150097, 1.000000000000000000),
 ( 1.000000000000000000, 0.7074674355297142503, 1.000000000000000000),
 ( 1.000000000000000000, 0.7074683863501984860, 1.000000000000000000),
 ( 1.000000000000000000, 0.7074680773870454242, 1.000000000000000000),
 ( 1.000000000000000000, 0.7074680753537760936, 1.000000000000000000),
 ( 1.000000000000000000, 0.7074680743359408330, 1.000000000000000000),
 ( 1.000000000000000000, 0.7074680712787539960, 1.000000000000000000),
 ( 1.000000000000000000, 0.7074680692358628065, 1.000000000000000000),
 ( 1.000000000000000000, 0.7074680671880581029, 1.000000000000000000) ) ) 
 REPRESENTATION_ITEM ( '' )  SURFACE ( )  );
#8909 = CARTESIAN_POINT ( 'NONE',  ( 0.000000000000000000, -10.85582367538895276, 1.425064293572299023 ) ) ;
#8910 = DIRECTION ( 'NONE',  ( 0.000000000000000000, 0.000000000000000000, 1.000000000000000000 ) ) ;
#8911 = ORIENTED_EDGE ( 'NONE', *, *, #30617, .T. ) ;
#8912 = CARTESIAN_POINT ( 'NONE',  ( -3.135269660805079628, -0.5000000000000024425, -1.949999999999999956 ) ) ;
#8913 = ORIENTED_EDGE ( 'NONE', *, *, #20438, .F. ) ;
#8914 = EDGE_LOOP ( 'NONE', ( #3152, #5243, #25005 ) ) ;
#8915 = CARTESIAN_POINT ( 'NONE',  ( 6.357667873252800028, 3.476490553296956332, -7.873899671211455953 ) ) ;
#8916 = EDGE_CURVE ( 'NONE', #28886, #9323, #2848, .T. ) ;
#8917 = B_SPLINE_SURFACE_WITH_KNOTS ( 'NONE', 3, 3, ( 
 ( #27581, #12533, #10014, #20225, #15206, #30118, #17387, #22889, #14850, #11157 ),
 ( #13179, #15708, #5819, #21062, #8182, #3167, #28581, #20726, #31408, #484 ),
 ( #20878, #23538, #978, #28884, #13507, #10849, #8339, #656, #18197, #30926 ),
 ( #10668, #26225, #31093, #21362, #16186, #23720, #3024, #28405, #5988, #13666 ) ),
 .UNSPECIFIED., .F., .F., .F.,
 ( 4, 4 ),
 ( 4, 3, 3, 4 ),
 ( -2.395551311511394542E-13, 1.000000000000001776 ),
 ( 0.003584360682139460345, 0.5017921803410697601, 0.7508960901705348245, 1.000000000000000000 ),
 .UNSPECIFIED. ) ;
#8919 = VERTEX_POINT ( 'NONE', #28948 ) ;
#8918 = CARTESIAN_POINT ( 'NONE',  ( 3.020080204145388691, -4.831795131253269204, 7.542713057966124346 ) ) ;
#8920 = ORIENTED_EDGE ( 'NONE', *, *, #873, .F. ) ;
#8921 = CARTESIAN_POINT ( 'NONE',  ( -46.10000000000000142, -10.96966150227468972, 6.999999999999999112 ) ) ;
#8922 = EDGE_LOOP ( 'NONE', ( #31980, #5927, #4998 ) ) ;
#8923 = FACE_OUTER_BOUND ( 'NONE', #31110, .T. ) ;
#8924 = DIRECTION ( 'NONE',  ( -1.000000000000000000, -0.000000000000000000, -0.000000000000000000 ) ) ;
#8926 = ORIENTED_EDGE ( 'NONE', *, *, #10150, .F. ) ;
#8925 = CARTESIAN_POINT ( 'NONE',  ( 23.87614828266676170, -3.446665583135163580, -0.4367666033346507271 ) ) ;
#8927 = LINE ( 'NONE', #24320, #19919 ) ;
#8928 = CARTESIAN_POINT ( 'NONE',  ( 5.612973690782940395, -0.1996300861631509771, 8.213905076232780544 ) ) ;
#8929 = EDGE_CURVE ( 'NONE', #6855, #14402, #23917, .T. ) ;
#8930 = DIRECTION ( 'NONE',  ( 0.000000000000000000, 1.000000000000000000, 0.000000000000000000 ) ) ;
#8931 = EDGE_CURVE ( 'NONE', #4375, #6812, #23109, .T. ) ;
#8932 = CARTESIAN_POINT ( 'NONE',  ( 3.499999999999999556, 0.000000000000000000, 0.000000000000000000 ) ) ;
#8933 = CARTESIAN_POINT ( 'NONE',  ( 108.0283109730694520, -18.47703308593441562, 4.359537947287052795 ) ) ;
#8934 = CARTESIAN_POINT ( 'NONE',  ( -0.2493515011840002071, -1.403010508276435031, -5.485967528433937979 ) ) ;
#8935 = FACE_OUTER_BOUND ( 'NONE', #27678, .T. ) ;
#8936 = CARTESIAN_POINT ( 'NONE',  ( 9.999999999999998224, -4.753758587302148619, 3.462581523170091167E-33 ) ) ;
#8937 = EDGE_CURVE ( 'NONE', #18451, #30629, #27375, .T. ) ;
#8938 = DIRECTION ( 'NONE',  ( 0.000000000000000000, 0.000000000000000000, 1.000000000000000000 ) ) ;
#8939 = DIRECTION ( 'NONE',  ( -8.281886410780533213E-17, -0.9659258262890709767, 0.2588190451025108030 ) ) ;
#8940 = PLANE ( 'NONE',  #15043 ) ;
#8941 = DIRECTION ( 'NONE',  ( -7.770718973608944144E-17, -0.9063077870366468280, -0.4226182617407062136 ) ) ;
#8942 = CARTESIAN_POINT ( 'NONE',  ( -4.600050802731187716, -0.9222479816126459840, -3.113457007523259268 ) ) ;
#8943 = ORIENTED_EDGE ( 'NONE', *, *, #9566, .F. ) ;
#8944 = ADVANCED_FACE ( 'NONE', ( #13378 ), #11886, .T. ) ;
#8945 = CARTESIAN_POINT ( 'NONE',  ( -7.200050800000000528, -2.331437884370912705, 1.887961173149512062 ) ) ;
#8946 = CARTESIAN_POINT ( 'NONE',  ( 22.85793694858476144, -21.91835806764118999, -1.144022321087336813 ) ) ;
#8947 = DIRECTION ( 'NONE',  ( -0.000000000000000000, -0.000000000000000000, -1.000000000000000000 ) ) ;
#8948 = CARTESIAN_POINT ( 'NONE',  ( -41.34821589589207491, -14.97033716811276527, 5.482725084223756262 ) ) ;
#8949 = ORIENTED_EDGE ( 'NONE', *, *, #328, .F. ) ;
#8950 = FACE_OUTER_BOUND ( 'NONE', #21078, .T. ) ;
#8951 = ORIENTED_EDGE ( 'NONE', *, *, #28942, .T. ) ;
#8952 = CARTESIAN_POINT ( 'NONE',  ( 2.123522008129191008, -10.79631020383399864, 1.499999999999645173 ) ) ;
#8953 = SECURITY_CLASSIFICATION_LEVEL ( 'unclassified' ) ;
#8954 = VERTEX_POINT ( 'NONE', #31457 ) ;
#8955 = CARTESIAN_POINT ( 'NONE',  ( 54.95170718583340630, -5.584587902149642069, 4.215290387855766596 ) ) ;
#8956 = DIRECTION ( 'NONE',  ( 1.000000000000000000, -8.574039729943018344E-17, -0.000000000000000000 ) ) ;
#8957 = CARTESIAN_POINT ( 'NONE',  ( 69.03558484036936704, -5.418257723488958177, -4.312042181581901445 ) ) ;
#8958 = CARTESIAN_POINT ( 'NONE',  ( 23.72064572292702778, -17.26593119145025668, -1.418862781619861346 ) ) ;
#8959 = CARTESIAN_POINT ( 'NONE',  ( 4.187842409712549624E-16, 4.884328206559851893, -1.115095498423258391 ) ) ;
#8960 = ORIENTED_EDGE ( 'NONE', *, *, #5122, .T. ) ;
#8961 = EDGE_CURVE ( 'NONE', #15643, #136, #3362, .T. ) ;
#8962 = CARTESIAN_POINT ( 'NONE',  ( 9.282537329960032224, 0.2172754300400924765, 1.041239158277174504 ) ) ;
#8963 = ADVANCED_FACE ( 'NONE', ( #18742, #13866 ), #11213, .T. ) ;
#8964 = CARTESIAN_POINT ( 'NONE',  ( 22.70718278262463841, -21.88016059487463849, -1.342589741762356237 ) ) ;
#8965 = CARTESIAN_POINT ( 'NONE',  ( 18.87719011064256236, -4.549990820396901725, -3.693496858444236697 ) ) ;
#8967 = EDGE_LOOP ( 'NONE', ( #3083, #18302, #659, #16895 ) ) ;
#8966 = CARTESIAN_POINT ( 'NONE',  ( 25.57055368252914462, 0.2377959888981342196, -2.835553682530281172 ) ) ;
#8968 = CARTESIAN_POINT ( 'NONE',  ( -2.362550801365593589, 2.752080473201636845, -2.228590825266444142 ) ) ;
#8969 = DIRECTION ( 'NONE',  ( -0.000000000000000000, -1.000000000000000000, -0.000000000000000000 ) ) ;
#8970 = DIRECTION ( 'NONE',  ( -1.000000000000000000, 0.000000000000000000, 0.000000000000000000 ) ) ;
#8971 = CARTESIAN_POINT ( 'NONE',  ( 108.5619817448483531, 15.65002148400673754, 0.4463807625373211185 ) ) ;
#8972 = DIRECTION ( 'NONE',  ( 0.000000000000000000, 0.9659258262890693114, -0.2588190451025167427 ) ) ;
#8973 = DIRECTION ( 'NONE',  ( 0.2880220749472531261, 0.1662896225033515807, -0.9430753128943476504 ) ) ;
#8974 = SHAPE_REPRESENTATION ( 'Part3_SlicingGear', ( #2865 ), #7630 ) ;
#8975 = CARTESIAN_POINT ( 'NONE',  ( 7.249760686538667009, 8.437262856154164936, 2.318425219014256911 ) ) ;
#8976 = CARTESIAN_POINT ( 'NONE',  ( 10.00000000000000178, 1.476463073999634723, 4.787500056513374069 ) ) ;
#8977 = CARTESIAN_POINT ( 'NONE',  ( -1.528445841742499756, -6.248157669862440144, 5.485967528433933538 ) ) ;
#8978 = VERTEX_POINT ( 'NONE', #23768 ) ;
#8979 = CARTESIAN_POINT ( 'NONE',  ( 20.79750000273118715, -2.594547506269383685, -0.7685399846772043020 ) ) ;
#8980 = ORIENTED_EDGE ( 'NONE', *, *, #26233, .F. ) ;
#8981 = EDGE_CURVE ( 'NONE', #18491, #15207, #14052, .T. ) ;
#8982 = DIRECTION ( 'NONE',  ( 1.000000000000000000, -0.000000000000000000, -0.000000000000000000 ) ) ;
#8983 = APPROVAL ( #7437, 'UNKNOWN' ) ;
#8984 = CARTESIAN_POINT ( 'NONE',  ( 107.4500593345376558, -17.36019228850485163, -4.522129901861164925 ) ) ;
#8985 = CARTESIAN_POINT ( 'NONE',  ( 10.55147673363118876, -4.116875700062067267, -2.376879293651108060 ) ) ;
#8986 = CARTESIAN_POINT ( 'NONE',  ( 69.12709522372956883, -7.241778149835164768, 2.184957268579549083 ) ) ;
#8987 = ORIENTED_EDGE ( 'NONE', *, *, #23011, .F. ) ;
#8988 = DIRECTION ( 'NONE',  ( 0.000000000000000000, 0.000000000000000000, 1.000000000000000000 ) ) ;
#8989 = B_SPLINE_CURVE_WITH_KNOTS ( 'NONE', 3,
 ( #16996, #12312, #22038, #12156, #4497, #17172, #22354, #32259, #24868, #27384 ),
 .UNSPECIFIED., .F., .F.,
 ( 4, 2, 2, 2, 4 ),
 ( 1.968338519012285667E-07, 0.0005467926089500455998, 0.001093388384048189993, 0.001639984159146334278, 0.002186579934244478780 ),
 .UNSPECIFIED. ) ;
#8990 = EDGE_LOOP ( 'NONE', ( #31214, #11045, #808, #18335, #5312, #163, #30458, #19822, #16947, #31364 ) ) ;
#8991 = DATE_AND_TIME ( #31927, #3398 ) ;
#8992 = CARTESIAN_POINT ( 'NONE',  ( 85.03573724897340469, -5.203500048815656420, 3.995005841633558319 ) ) ;
#8993 = EDGE_CURVE ( 'NONE', #19834, #21274, #16697, .T. ) ;
#8994 = CARTESIAN_POINT ( 'NONE',  ( 0.000000000000000000, 0.000000000000000000, 0.000000000000000000 ) ) ;
#8995 = ORIENTED_EDGE ( 'NONE', *, *, #21617, .F. ) ;
#8996 = CARTESIAN_POINT ( 'NONE',  ( 6.357667975083865386, 3.797112024432019339, 7.724391461487803312 ) ) ;
#8997 = ORIENTED_EDGE ( 'NONE', *, *, #27733, .F. ) ;
#8998 = EDGE_LOOP ( 'NONE', ( #21471, #28554, #26732 ) ) ;
#8999 = CARTESIAN_POINT ( 'NONE',  ( 24.75111450864415730, -6.623356326098185375E-16, -2.499999999999998224 ) ) ;
#9000 = CARTESIAN_POINT ( 'NONE',  ( -2.124956573341760357, 1.323625320507108460, 3.284597389080124774 ) ) ;
#9001 = CARTESIAN_POINT ( 'NONE',  ( 22.10999999999999943, 1.942864903642424146, 1.573300977624592534 ) ) ;
#9002 = FACE_OUTER_BOUND ( 'NONE', #15306, .T. ) ;
#9004 = VERTEX_POINT ( 'NONE', #28630 ) ;
#9003 = CARTESIAN_POINT ( 'NONE',  ( 3.830085165118329002E-16, 4.467071865485494619, -1.625881193364653088 ) ) ;
#9005 = CARTESIAN_POINT ( 'NONE',  ( -5.187550801365593323, -3.521866450007987037, -0.3701630799359323931 ) ) ;
#9006 = CARTESIAN_POINT ( 'NONE',  ( 0.000000000000000000, -6.807171995660629804, 6.478011392632865295 ) ) ;
#9007 = CARTESIAN_POINT ( 'NONE',  ( 7.541562596972942956, -18.86384717194523475, 1.499999999999760192 ) ) ;
#9008 = DIRECTION ( 'NONE',  ( 0.000000000000000000, 0.000000000000000000, 1.000000000000000000 ) ) ;
#9009 = ORIENTED_EDGE ( 'NONE', *, *, #15421, .T. ) ;
#9011 = ORIENTED_EDGE ( 'NONE', *, *, #3981, .T. ) ;
#9010 = CARTESIAN_POINT ( 'NONE',  ( 13.49488892923315220, 21.89889427266717092, 1.242426148748663195 ) ) ;
#9012 = DIRECTION ( 'NONE',  ( 1.000000000000000000, 0.000000000000000000, 0.000000000000000000 ) ) ;
#9013 = B_SPLINE_CURVE_WITH_KNOTS ( 'NONE', 3,
 ( #22632, #22135, #11933, #27294, #9243, #24951 ),
 .UNSPECIFIED., .F., .F.,
 ( 4, 2, 4 ),
 ( 0.000000000000000000, 0.001111101121386790349, 0.002222202242773580697 ),
 .UNSPECIFIED. ) ;
#9014 = CARTESIAN_POINT ( 'NONE',  ( 22.11000000273118715, 1.573300977624590313, -1.942864903642426144 ) ) ;
#9015 = CARTESIAN_POINT ( 'NONE',  ( -23.54713438637982748, 4.195786794269684705, 1.499999999999999112 ) ) ;
#9016 = CARTESIAN_POINT ( 'NONE',  ( -17.85000000000000142, -10.96966150227469505, 4.000000000000000000 ) ) ;
#9017 = LINE ( 'NONE', #19237, #29535 ) ;
#9018 = CARTESIAN_POINT ( 'NONE',  ( 47.88941090692655678, -4.233884984401186991, 1.873788949266326664 ) ) ;
#9019 = CARTESIAN_POINT ( 'NONE',  ( -2.487550801365593589, 2.752080473201636845, -2.228590825266444142 ) ) ;
#9020 = CARTESIAN_POINT ( 'NONE',  ( 56.97280603064898941, -277.2763395528616002, -2.806473568333519353 ) ) ;
#9021 = ORIENTED_EDGE ( 'NONE', *, *, #3048, .T. ) ;
#9022 = AXIS2_PLACEMENT_3D ( 'NONE', #19434, #18880, #16677 ) ;
#9023 = DIRECTION ( 'NONE',  ( 0.000000000000000000, 0.000000000000000000, 1.000000000000000000 ) ) ;
#9024 = DIRECTION ( 'NONE',  ( 1.000000000000000000, -8.574039729943018344E-17, -0.000000000000000000 ) ) ;
#9026 = CARTESIAN_POINT ( 'NONE',  ( 6.883866601413088482, -7.883091392499345318, 3.754588506078578192 ) ) ;
#9025 = CARTESIAN_POINT ( 'NONE',  ( 6.524595126109736576, -2.112519041817556342, -8.397268106035234325 ) ) ;
#9027 = EDGE_CURVE ( 'NONE', #31957, #1852, #11397, .T. ) ;
#9028 = ORIENTED_EDGE ( 'NONE', *, *, #4757, .T. ) ;
#9029 = EDGE_CURVE ( 'NONE', #25776, #16558, #881, .T. ) ;
#9030 = AXIS2_PLACEMENT_3D ( 'NONE', #9043, #7230, #21767 ) ;
#9031 = DIRECTION ( 'NONE',  ( 0.000000000000000000, 0.000000000000000000, -1.000000000000000000 ) ) ;
#9032 = ORIENTED_EDGE ( 'NONE', *, *, #6548, .F. ) ;
#9033 = DIRECTION ( 'NONE',  ( 0.9816271834476637537, 0.000000000000000000, 0.1908089953765453872 ) ) ;
#9034 = EDGE_CURVE ( 'NONE', #18153, #5447, #16547, .T. ) ;
#9036 = EDGE_LOOP ( 'NONE', ( #24774, #21737, #24214, #33005 ) ) ;
#9035 = CARTESIAN_POINT ( 'NONE',  ( 102.3440361197693278, -2.855691808908399132, -3.994702627092255653 ) ) ;
#9037 = ORIENTED_EDGE ( 'NONE', *, *, #10444, .F. ) ;
#9038 =( REPRESENTATION_RELATIONSHIP ('NONE','NONE', #1085, #8974 ) REPRESENTATION_RELATIONSHIP_WITH_TRANSFORMATION ( #434 )SHAPE_REPRESENTATION_RELATIONSHIP( ) );
#9039 = PLANE ( 'NONE',  #31588 ) ;
#9041 = VERTEX_POINT ( 'NONE', #10907 ) ;
#9040 = CARTESIAN_POINT ( 'NONE',  ( -4.456262821554182629, -5.024290100364269485, -1.500000000000000000 ) ) ;
#9042 = CARTESIAN_POINT ( 'NONE',  ( 11.28452421127990135, 4.182904784596867209, -1.500000000000000000 ) ) ;
#9043 = CARTESIAN_POINT ( 'NONE',  ( -8.000050800000000351, 0.000000000000000000, 0.000000000000000000 ) ) ;
#9044 = DIRECTION ( 'NONE',  ( 0.000000000000000000, 0.000000000000000000, 1.000000000000000000 ) ) ;
#9045 = CARTESIAN_POINT ( 'NONE',  ( 8.690654615650263537, -10.89241706942853583, -1.000000000000000000 ) ) ;
#9047 = ORIENTED_EDGE ( 'NONE', *, *, #2273, .T. ) ;
#9046 = CARTESIAN_POINT ( 'NONE',  ( 108.0529299568327986, -18.83154032767301445, -4.758045365066062793 ) ) ;
#9048 = CARTESIAN_POINT ( 'NONE',  ( 6.524595395369781947, 3.538595500939588856, 7.902859683906627630 ) ) ;
#9049 = CIRCLE ( 'NONE', #27748, 6.248999999999999666 ) ;
#9050 = VECTOR ( 'NONE', #27991, 1000.000000000000000 ) ;
#9051 = LINE ( 'NONE', #2057, #4377 ) ;
#9052 = CARTESIAN_POINT ( 'NONE',  ( 18.72482702355224404, -6.253104344976480711, 3.390608483624313330 ) ) ;
#9053 = CARTESIAN_POINT ( 'NONE',  ( 24.51663722516862620, -17.45316359950712837, -1.478737313599387093 ) ) ;
#9054 = CARTESIAN_POINT ( 'NONE',  ( 18.68265047573912341, -6.724553502642427461, -4.522129901861164036 ) ) ;
#9055 = AXIS2_PLACEMENT_3D ( 'NONE', #22122, #32334, #29803 ) ;
#9056 = VERTEX_POINT ( 'NONE', #21112 ) ;
#9057 = DIRECTION ( 'NONE',  ( -0.08910563629484094528, -0.9960221812693187404, 0.000000000000000000 ) ) ;
#9058 = CARTESIAN_POINT ( 'NONE',  ( 7.249760686538666121, 7.347880794884119736E-16, -6.000000000000000000 ) ) ;
#9059 = DIRECTION ( 'NONE',  ( -0.4809547266710045288, -0.000000000000000000, -0.8767454310646958238 ) ) ;
#9060 = ORIENTED_EDGE ( 'NONE', *, *, #1132, .F. ) ;
#9061 = CARTESIAN_POINT ( 'NONE',  ( 0.000000000000000000, 0.000000000000000000, 0.000000000000000000 ) ) ;
#9062 = EDGE_CURVE ( 'NONE', #22797, #28496, #29497, .T. ) ;
#9063 = CARTESIAN_POINT ( 'NONE',  ( 2.589202905186835046, 9.453729690310147760, 4.126870756446492372 ) ) ;
#9064 = ORIENTED_EDGE ( 'NONE', *, *, #1843, .T. ) ;
#9065 = CARTESIAN_POINT ( 'NONE',  ( 6.706201599914444422, -13.33059280214037123, -1.500000000000000444 ) ) ;
#9066 = EDGE_CURVE ( 'NONE', #10505, #5926, #27249, .T. ) ;
#9067 = ORIENTED_EDGE ( 'NONE', *, *, #16290, .T. ) ;
#9068 = EDGE_CURVE ( 'NONE', #9919, #6843, #26313, .T. ) ;
#9069 = CIRCLE ( 'NONE', #2716, 0.5000000000000007772 ) ;
#9070 = B_SPLINE_CURVE_WITH_KNOTS ( 'NONE', 3,
 ( #24541, #31934, #27572, #29410, #2006, #27415, #4169, #4521 ),
 .UNSPECIFIED., .F., .F.,
 ( 4, 2, 2, 4 ),
 ( 2.851296420475814781E-07, 0.001262135616826467023, 0.001893060860418674688, 0.002523986104010882137 ),
 .UNSPECIFIED. ) ;
#9071 = ORIENTED_EDGE ( 'NONE', *, *, #2209, .T. ) ;
#9072 = CARTESIAN_POINT ( 'NONE',  ( -48.50000000000000000, -10.96966150227468972, 0.9999999999999991118 ) ) ;
#9074 = ORIENTED_EDGE ( 'NONE', *, *, #31084, .F. ) ;
#9073 = FACE_OUTER_BOUND ( 'NONE', #14574, .T. ) ;
#9075 = ORIENTED_EDGE ( 'NONE', *, *, #11395, .F. ) ;
#9076 = CARTESIAN_POINT ( 'NONE',  ( 23.86000000136559507, -0.9349337715887247047, 3.156283516753367824 ) ) ;
#9077 = ORIENTED_EDGE ( 'NONE', *, *, #9029, .T. ) ;
#9079 = VECTOR ( 'NONE', #33050, 1000.000000000000000 ) ;
#9078 = DIRECTION ( 'NONE',  ( 0.000000000000000000, -0.000000000000000000, 1.000000000000000000 ) ) ;
#9080 = CARTESIAN_POINT ( 'NONE',  ( 0.000000000000000000, -7.958834565716820464, 7.593217523260552326 ) ) ;
#9082 = VERTEX_POINT ( 'NONE', #9368 ) ;
#9081 = DIRECTION ( 'NONE',  ( 1.000000000000000000, 0.000000000000000000, 0.000000000000000000 ) ) ;
#9083 = CARTESIAN_POINT ( 'NONE',  ( 108.0291781248180598, -18.48951985539477505, -4.325670280508457921 ) ) ;
#9084 = DIRECTION ( 'NONE',  ( -0.000000000000000000, -0.000000000000000000, -1.000000000000000000 ) ) ;
#9085 = FACE_OUTER_BOUND ( 'NONE', #27522, .T. ) ;
#9086 = CARTESIAN_POINT ( 'NONE',  ( 3.499999999999999556, -1.179494851233943598, 6.136676046192483192 ) ) ;
#9087 = CARTESIAN_POINT ( 'NONE',  ( -0.4046470899337971106, -12.07320251013791790, -5.485967528433938867 ) ) ;
#9088 = CARTESIAN_POINT ( 'NONE',  ( 69.15727116336863389, -7.845927800133500440, -0.07017451552784023661 ) ) ;
#9089 = CARTESIAN_POINT ( 'NONE',  ( -29.35000000000000497, -10.96966150227469505, -11.50000000000000000 ) ) ;
#9090 = AXIS2_PLACEMENT_3D ( 'NONE', #27180, #16655, #29204 ) ;
#9091 = CIRCLE ( 'NONE', #6426, 8.749000000000002331 ) ;
#9092 = CARTESIAN_POINT ( 'NONE',  ( 5.887530024394190598, 7.753515897409886115, 3.218326717262283143 ) ) ;
#9093 = CARTESIAN_POINT ( 'NONE',  ( -5.509727295071408903, 5.993169562190665545, -2.952988490976575786 ) ) ;
#9094 = CARTESIAN_POINT ( 'NONE',  ( 20.74999999999999645, -5.000000000000005329, 6.123233995736771213E-16 ) ) ;
#9095 = AXIS2_PLACEMENT_3D ( 'NONE', #32976, #7728, #2548 ) ;
#9096 =( BOUNDED_SURFACE ( )  B_SPLINE_SURFACE ( 3, 2, ( 
 ( #13168, #8327, #28872 ),
 ( #23707, #26212, #3325 ),
 ( #30914, #7988, #15843 ),
 ( #18181, #16169, #13654 ) ),
 .UNSPECIFIED., .F., .F., .F. ) 
 B_SPLINE_SURFACE_WITH_KNOTS ( ( 4, 4 ),
 ( 3, 3 ),
 ( 0.0001475438429531535209, 0.0001830289614101955511 ),
 ( 0.000000000000000000, 1.000000000000000000 ),
 .UNSPECIFIED. ) 
 GEOMETRIC_REPRESENTATION_ITEM ( )  RATIONAL_B_SPLINE_SURFACE ( (
 ( 1.000000000000000000, 0.8123215895924797980, 1.000000000000000000),
 ( 1.000000000000000000, 0.7824045309858685959, 1.000000000000000000),
 ( 1.000000000000000000, 0.7465390509822480425, 1.000000000000000000),
 ( 1.000000000000000000, 0.7071067812051371471, 1.000000000000000000) ) ) 
 REPRESENTATION_ITEM ( '' )  SURFACE ( )  );
#9097 = ADVANCED_FACE ( 'NONE', ( #19578 ), #11597, .F. ) ;
#9098 = DIRECTION ( 'NONE',  ( 0.000000000000000000, 0.000000000000000000, 1.000000000000000000 ) ) ;
#9099 = CARTESIAN_POINT ( 'NONE',  ( -6.400050802731188426, -3.113457007523259268, 0.9222479816126455399 ) ) ;
#9100 = ORIENTED_EDGE ( 'NONE', *, *, #7048, .T. ) ;
#9101 = CARTESIAN_POINT ( 'NONE',  ( -7.150050800000000706, -3.113457007523259268, 0.9222479816126455399 ) ) ;
#9102 = AXIS2_PLACEMENT_3D ( 'NONE', #22415, #26950, #9031 ) ;
#9103 = EDGE_CURVE ( 'NONE', #10415, #31571, #9875, .T. ) ;
#9104 = CARTESIAN_POINT ( 'NONE',  ( 23.15209817170719120, -21.93517036684206900, -1.064739674281773185 ) ) ;
#9105 = CARTESIAN_POINT ( 'NONE',  ( -40.82415311671282865, -13.09326638694065359, 5.845147494867474869 ) ) ;
#9106 = VERTEX_POINT ( 'NONE', #5192 ) ;
#9107 = CARTESIAN_POINT ( 'NONE',  ( 8.571721676197185502, -11.50721971753343809, -1.500000000000000000 ) ) ;
#9108 = EDGE_LOOP ( 'NONE', ( #23287, #24232, #8913, #2475 ) ) ;
#9109 = CARTESIAN_POINT ( 'NONE',  ( 4.138787901720749396, -11.97482149199507084, 1.500000000000000000 ) ) ;
#9110 = APPROVAL_STATUS ( 'not_yet_approved' ) ;
#9111 = CIRCLE ( 'NONE', #1148, 11.00000000000000000 ) ;
#9113 = EDGE_CURVE ( 'NONE', #24368, #14256, #12697, .T. ) ;
#9112 = CARTESIAN_POINT ( 'NONE',  ( 7.249760686538667009, 6.147671362329219846, 6.226446564517938320 ) ) ;
#9114 = ORIENTED_EDGE ( 'NONE', *, *, #19701, .T. ) ;
#9115 = VECTOR ( 'NONE', #11280, 1000.000000000000000 ) ;
#9116 = CARTESIAN_POINT ( 'NONE',  ( -4.456246017397374359, -5.024161734168909099, 1.500000000000000666 ) ) ;
#9117 = AXIS2_PLACEMENT_3D ( 'NONE', #14856, #9361, #4685 ) ;
#9118 = CARTESIAN_POINT ( 'NONE',  ( 0.000000000000000000, 0.005878491403554959860, -7.047692205288322853 ) ) ;
#9119 = CARTESIAN_POINT ( 'NONE',  ( 28.67878734107521765, -6.190522357037703927, -4.312042181584450518 ) ) ;
#9120 = AXIS2_PLACEMENT_3D ( 'NONE', #3018, #8821, #13173 ) ;
#9121 = DIRECTION ( 'NONE',  ( -1.000000000000000000, 8.574039729943018344E-17, -0.000000000000000000 ) ) ;
#9122 = LINE ( 'NONE', #14301, #22519 ) ;
#9123 = ORIENTED_EDGE ( 'NONE', *, *, #4857, .T. ) ;
#9124 = EDGE_CURVE ( 'NONE', #11002, #17553, #30936, .T. ) ;
#9125 = CARTESIAN_POINT ( 'NONE',  ( 9.127968561342536091, 0.03517121848165041115, 1.257822814154217816 ) ) ;
#9126 = DIRECTION ( 'NONE',  ( -0.1027947991993878318, 0.9947025833170222153, 0.000000000000000000 ) ) ;
#9127 = DIRECTION ( 'NONE',  ( -1.000000000000000000, -0.000000000000000000, 0.000000000000000000 ) ) ;
#9128 = AXIS2_PLACEMENT_3D ( 'NONE', #1269, #13765, #18633 ) ;
#9130 = VERTEX_POINT ( 'NONE', #8012 ) ;
#9129 = CYLINDRICAL_SURFACE ( 'NONE', #18702, 8.500000000000000000 ) ;
#9131 = LINE ( 'NONE', #24859, #10847 ) ;
#9132 = CARTESIAN_POINT ( 'NONE',  ( 5.377543748152548986, -8.014274990069656823, 8.669741416787380218E-17 ) ) ;
#9133 = CARTESIAN_POINT ( 'NONE',  ( 3.249999999999999556, 7.360373001730919462, 4.729683950898899703 ) ) ;
#9134 = CARTESIAN_POINT ( 'NONE',  ( 0.6728000631949152543, 9.133409206458242835, 0.5626559338999654880 ) ) ;
#9135 = CARTESIAN_POINT ( 'NONE',  ( 5.885541615502094537, -1.090540896198865406, 8.322568858718550899 ) ) ;
#9136 = DIRECTION ( 'NONE',  ( -0.000000000000000000, 1.000000000000000000, -0.000000000000000000 ) ) ;
#9137 = CARTESIAN_POINT ( 'NONE',  ( 3.830085165118310759E-16, 4.467071865485471527, 1.625881193364712596 ) ) ;
#9138 = VERTEX_POINT ( 'NONE', #30282 ) ;
#9139 = EDGE_CURVE ( 'NONE', #10337, #21393, #30627, .T. ) ;
#9140 = AXIS2_PLACEMENT_3D ( 'NONE', #11055, #15901, #8713 ) ;
#9141 = ORIENTED_EDGE ( 'NONE', *, *, #16304, .F. ) ;
#9142 = AXIS2_PLACEMENT_3D ( 'NONE', #1103, #19000, #3776 ) ;
#9143 = CIRCLE ( 'NONE', #13417, 4.000000000000000000 ) ;
#9144 = DIRECTION ( 'NONE',  ( -1.000000000000000000, -0.000000000000000000, 0.000000000000000000 ) ) ;
#9145 = DIRECTION ( 'NONE',  ( 0.000000000000000000, 0.4067366430758010964, -0.9135454576426006446 ) ) ;
#9146 = VECTOR ( 'NONE', #13318, 1000.000000000000000 ) ;
#9147 = CARTESIAN_POINT ( 'NONE',  ( 102.7116376760606755, -2.711456868667907916, -5.695980980372493008 ) ) ;
#9148 = EDGE_CURVE ( 'NONE', #32897, #780, #7357, .T. ) ;
#9149 = CARTESIAN_POINT ( 'NONE',  ( 25.75999999999999446, 1.747856820561523028, 2.520532175753987580 ) ) ;
#9150 = CARTESIAN_POINT ( 'NONE',  ( 69.13676591393961246, -7.435400085124271641, 1.873789664672798727 ) ) ;
#9151 = ORIENTED_EDGE ( 'NONE', *, *, #19067, .F. ) ;
#9152 = CARTESIAN_POINT ( 'NONE',  ( 107.7451628514262723, 16.75912612768599885, -1.277591108513651097 ) ) ;
#9153 = EDGE_CURVE ( 'NONE', #16073, #4552, #7707, .T. ) ;
#9154 = VECTOR ( 'NONE', #18367, 1000.000000000000000 ) ;
#9155 = VECTOR ( 'NONE', #3572, 1000.000000000000114 ) ;
#9156 = EDGE_LOOP ( 'NONE', ( #31127, #11678, #8354, #23610 ) ) ;
#9157 = CALENDAR_DATE ( 2026, 6, 10 ) ;
#9158 = CARTESIAN_POINT ( 'NONE',  ( 85.03567598614395706, -5.202494821364011202, 3.996603857811756200 ) ) ;
#9159 = EDGE_CURVE ( 'NONE', #20999, #23780, #845, .T. ) ;
#9160 = FACE_OUTER_BOUND ( 'NONE', #25938, .T. ) ;
#9161 = AXIS2_PLACEMENT_3D ( 'NONE', #13720, #6540, #16742 ) ;
#9162 = PLANE ( 'NONE',  #15623 ) ;
#9163 = ORIENTED_EDGE ( 'NONE', *, *, #11199, .T. ) ;
#9164 = AXIS2_PLACEMENT_3D ( 'NONE', #9556, #1736, #19774 ) ;
#9165 = VERTEX_POINT ( 'NONE', #5041 ) ;
#9166 = CIRCLE ( 'NONE', #26876, 2.999999999999999556 ) ;
#9167 = DIRECTION ( 'NONE',  ( -0.000000000000000000, -0.000000000000000000, -1.000000000000000000 ) ) ;
#9168 = CARTESIAN_POINT ( 'NONE',  ( 5.377543748152549874, -6.940565734314570356, -4.007137495034885255 ) ) ;
#9169 = CIRCLE ( 'NONE', #3342, 2.524999999999999467 ) ;
#9170 = CARTESIAN_POINT ( 'NONE',  ( 25.35999999999999943, -1.573300977624594976, 1.942864903642425700 ) ) ;
#9172 = EDGE_CURVE ( 'NONE', #7709, #24619, #15218, .T. ) ;
#9171 = AXIS2_PLACEMENT_3D ( 'NONE', #9476, #6811, #16849 ) ;
#9173 = CARTESIAN_POINT ( 'NONE',  ( 0.4717033495752643857, -8.231128558055790023, -1.500000000000035305 ) ) ;
#9174 =( BOUNDED_CURVE ( )  B_SPLINE_CURVE ( 3, ( #17960, #20788, #8261, #30848 ),
 .UNSPECIFIED., .F., .F. ) 
 B_SPLINE_CURVE_WITH_KNOTS ( ( 4, 4 ),
 ( 4.712388980384688786, 4.894398194314031336 ),
 .UNSPECIFIED. ) 
 CURVE ( )  GEOMETRIC_REPRESENTATION_ITEM ( )  RATIONAL_B_SPLINE_CURVE ( ( 1.000000000000000000, 0.9972412918903137413, 0.9972412918903137413, 1.000000000000000000 ) ) 
 REPRESENTATION_ITEM ( '' )  );
#9176 = ORIENTED_EDGE ( 'NONE', *, *, #11575, .T. ) ;
#9175 = FACE_OUTER_BOUND ( 'NONE', #29643, .T. ) ;
#9177 = CARTESIAN_POINT ( 'NONE',  ( -4.337550801365595454, -3.368539882008727115, -1.828967928396028064 ) ) ;
#9178 = CIRCLE ( 'NONE', #26799, 10.99999999999999822 ) ;
#9179 = FACE_OUTER_BOUND ( 'NONE', #19056, .T. ) ;
#9180 = CARTESIAN_POINT ( 'NONE',  ( -59.04504500748983986, -4.696780627829411969, 5.309652175818544428 ) ) ;
#9181 = CARTESIAN_POINT ( 'NONE',  ( 7.249760686538667009, -3.748318449932238838, -7.906491560603703839 ) ) ;
#9182 = TOROIDAL_SURFACE ( 'NONE', #26293, 10.51776515689528502, 0.5000000000000000000 ) ;
#9183 = ORIENTED_EDGE ( 'NONE', *, *, #32026, .T. ) ;
#9185 = ORIENTED_EDGE ( 'NONE', *, *, #19361, .T. ) ;
#9184 = CARTESIAN_POINT ( 'NONE',  ( 2.838908144950905932, -0.000000000000000000, 1.380700491544036623 ) ) ;
#9186 = VECTOR ( 'NONE', #776, 999.9999999999998863 ) ;
#9187 = CARTESIAN_POINT ( 'NONE',  ( 14.84491886980558029, 10.18391468479282302, 1.500000000000000222 ) ) ;
#9188 = CARTESIAN_POINT ( 'NONE',  ( 5.887529755120531227, 8.194579018285292449, 1.823049025159214631 ) ) ;
#9189 = EDGE_CURVE ( 'NONE', #27064, #24925, #678, .T. ) ;
#9190 = CARTESIAN_POINT ( 'NONE',  ( 25.42250000136559507, -0.3178988483021076838, -3.024605502323848949 ) ) ;
#9191 = DIRECTION ( 'NONE',  ( 8.281886410780490073E-17, 0.9659258262890662028, 0.2588190451025284000 ) ) ;
#9192 = CIRCLE ( 'NONE', #15068, 7.144028715714068056 ) ;
#9193 = DIRECTION ( 'NONE',  ( -2.219124775574953145E-17, -0.2588190451025242367, 0.9659258262890673130 ) ) ;
#9194 = PRODUCT_DEFINITION_SHAPE ( 'NONE', 'NONE',  #33101 ) ;
#9195 = AXIS2_PLACEMENT_3D ( 'NONE', #31157, #18256, #15083 ) ;
#9196 = EDGE_CURVE ( 'NONE', #28480, #15957, #24168, .T. ) ;
#9197 = VECTOR ( 'NONE', #12578, 1000.000000000000000 ) ;
#9198 = CARTESIAN_POINT ( 'NONE',  ( 68.92628806523022433, -3.240579989648459946, 0.4367667217252174661 ) ) ;
#9199 = CARTESIAN_POINT ( 'NONE',  ( -2.887550801365593500, -2.752080473201636845, 2.228590825266444586 ) ) ;
#9200 = ORIENTED_EDGE ( 'NONE', *, *, #24252, .F. ) ;
#9201 = DIRECTION ( 'NONE',  ( 0.4999999999999978351, 0.8660254037844399289, 0.000000000000000000 ) ) ;
#9202 = ORIENTED_EDGE ( 'NONE', *, *, #27178, .F. ) ;
#9203 = CIRCLE ( 'NONE', #12438, 0.4500000000000000111 ) ;
#9204 = AXIS2_PLACEMENT_3D ( 'NONE', #1916, #12089, #9555 ) ;
#9205 = CARTESIAN_POINT ( 'NONE',  ( 18.93617721851659041, -3.890633339435721982, -4.522129901861162260 ) ) ;
#9208 = CARTESIAN_POINT ( 'NONE',  ( 107.9802352237659022, -17.78475425570491453, 4.325014068553558744 ) ) ;
#9207 = CARTESIAN_POINT ( 'NONE',  ( 5.612718383992090665, -1.622626842546708081, -8.054241895195646705 ) ) ;
#9206 = AXIS2_PLACEMENT_3D ( 'NONE', #23737, #28740, #13682 ) ;
#9209 = ORIENTED_EDGE ( 'NONE', *, *, #30795, .F. ) ;
#9210 = EDGE_CURVE ( 'NONE', #23697, #32838, #14014, .T. ) ;
#9211 = CARTESIAN_POINT ( 'NONE',  ( 20.49917871223711785, -21.72428526870503163, 1.411325660096738766 ) ) ;
#9212 = ORIENTED_EDGE ( 'NONE', *, *, #21813, .F. ) ;
#9213 = CARTESIAN_POINT ( 'NONE',  ( 108.0048053234951198, -18.13855757953442449, 3.636029349014985090 ) ) ;
#9215 = ORIENTED_EDGE ( 'NONE', *, *, #24107, .F. ) ;
#9214 = CARTESIAN_POINT ( 'NONE',  ( 69.01327448684355659, -4.971206343640002245, -3.995337163040377781 ) ) ;
#9216 = ORIENTED_EDGE ( 'NONE', *, *, #4664, .F. ) ;
#9217 = CARTESIAN_POINT ( 'NONE',  ( 6.530491751506348308, 6.030130624359257396, -6.216163082443004306 ) ) ;
#9218 = ADVANCED_FACE ( 'NONE', ( #2879 ), #7862, .F. ) ;
#9219 = CARTESIAN_POINT ( 'NONE',  ( 21.07875000068279903, 0.2896100032356176412, 2.755455120372265476 ) ) ;
#9221 = ORIENTED_EDGE ( 'NONE', *, *, #13816, .T. ) ;
#9220 = CARTESIAN_POINT ( 'NONE',  ( 5.994454021012749934, -18.63465724242956156, -1.500000000000001332 ) ) ;
#9222 = CIRCLE ( 'NONE', #16170, 6.000000000000000000 ) ;
#9223 = CARTESIAN_POINT ( 'NONE',  ( 10.13996510774097004, 2.320984940005466513, -1.500000000000000000 ) ) ;
#9224 = CARTESIAN_POINT ( 'NONE',  ( 8.960941058736720422, 0.001013528757996738161, -1.090795311548453661 ) ) ;
#9225 = CIRCLE ( 'NONE', #21015, 8.500000000000000000 ) ;
#9226 = DIRECTION ( 'NONE',  ( 1.000000000000000000, 0.000000000000000000, 0.000000000000000000 ) ) ;
#9227 = CARTESIAN_POINT ( 'NONE',  ( 7.192400643299275309, -7.644771086295416573, -1.000000000000000000 ) ) ;
#9229 = ORIENTED_EDGE ( 'NONE', *, *, #9891, .T. ) ;
#9228 = CARTESIAN_POINT ( 'NONE',  ( 107.5579200398152295, -18.92771086533201341, -4.650503970115479113 ) ) ;
#9230 = LINE ( 'NONE', #29806, #3951 ) ;
#9231 = VECTOR ( 'NONE', #24838, 1000.000000000000000 ) ;
#9232 = AXIS2_PLACEMENT_3D ( 'NONE', #5039, #18052, #8349 ) ;
#9233 = DIRECTION ( 'NONE',  ( 8.541412920197208721E-17, 0.9961946980917446570, 0.08715574274766814400 ) ) ;
#9234 = CARTESIAN_POINT ( 'NONE',  ( 35.29143477761595449, -7.046680052079512535, 3.390608481268459151 ) ) ;
#9235 = AXIS2_PLACEMENT_3D ( 'NONE', #1696, #11898, #6247 ) ;
#9236 = EDGE_CURVE ( 'NONE', #7359, #16254, #25748, .T. ) ;
#9237 = B_SPLINE_CURVE_WITH_KNOTS ( 'NONE', 3,
 ( #28218, #24889, #2000, #14836, #25036, #11146, #10655, #473 ),
 .UNSPECIFIED., .F., .F.,
 ( 4, 2, 2, 4 ),
 ( 4.445333154581480097E-17, 0.0001981427792172239224, 0.0003962855584344033926, 0.0007925711168687612487 ),
 .UNSPECIFIED. ) ;
#9238 = LINE ( 'NONE', #25103, #12899 ) ;
#9239 = DIRECTION ( 'NONE',  ( -1.000000000000000000, -0.000000000000000000, 0.000000000000000000 ) ) ;
#9240 = ORIENTED_EDGE ( 'NONE', *, *, #15460, .T. ) ;
#9241 = CARTESIAN_POINT ( 'NONE',  ( -6.250050800000000351, -2.853674364686378695, -1.549418761218566809 ) ) ;
#9242 = EDGE_CURVE ( 'NONE', #15936, #28186, #26843, .T. ) ;
#9243 = CARTESIAN_POINT ( 'NONE',  ( 101.6304955275590771, -1.577711174180971065, -1.868788699937914854 ) ) ;
#9244 = CYLINDRICAL_SURFACE ( 'NONE', #17811, 5.010000000000000675 ) ;
#9245 = VERTEX_POINT ( 'NONE', #16203 ) ;
#9246 = AXIS2_PLACEMENT_3D ( 'NONE', #31044, #13287, #31863 ) ;
#9247 = AXIS2_PLACEMENT_3D ( 'NONE', #3017, #29066, #13172 ) ;
#9248 = VECTOR ( 'NONE', #6858, 1000.000000000000000 ) ;
#9249 = CARTESIAN_POINT ( 'NONE',  ( -8.000050800000002127, 0.9238973724631623918, -3.354839762463424524 ) ) ;
#9250 = DIRECTION ( 'NONE',  ( 1.000000000000000000, -2.473959037481237219E-13, 0.000000000000000000 ) ) ;
#9252 = EDGE_LOOP ( 'NONE', ( #20743, #4867, #23701, #9672, #5030 ) ) ;
#9251 = VECTOR ( 'NONE', #7279, 1000.000000000000000 ) ;
#9253 = CARTESIAN_POINT ( 'NONE',  ( 7.227634085595994407, -5.813588965143285492, 1.000000000000000222 ) ) ;
#9254 = ORIENTED_EDGE ( 'NONE', *, *, #3666, .T. ) ;
#9255 = AXIS2_PLACEMENT_3D ( 'NONE', #21951, #9250, #29665 ) ;
#9256 = ORIENTED_EDGE ( 'NONE', *, *, #17497, .T. ) ;
#9257 = CARTESIAN_POINT ( 'NONE',  ( -2.619378609982116135, -0.1905507107691023216, 1.628225384166350764 ) ) ;
#9259 = ORIENTED_EDGE ( 'NONE', *, *, #31059, .F. ) ;
#9258 = CARTESIAN_POINT ( 'NONE',  ( 2.795120501772739185, -5.116149273377877726, 8.308193303464529222 ) ) ;
#9260 = ORIENTED_EDGE ( 'NONE', *, *, #5001, .F. ) ;
#9261 = CARTESIAN_POINT ( 'NONE',  ( 24.11000000136559507, -3.156283516753370488, -0.9349337715887220401 ) ) ;
#9262 = CC_DESIGN_APPROVAL ( #28044, ( #14051 ) ) ;
#9263 = EDGE_LOOP ( 'NONE', ( #14187, #13730, #27872 ) ) ;
#9264 = CARTESIAN_POINT ( 'NONE',  ( 56.97280603064898941, -277.2763395528616002, 2.334455007174216057 ) ) ;
#9265 = DIRECTION ( 'NONE',  ( 0.000000000000000000, 0.000000000000000000, 1.000000000000000000 ) ) ;
#9267 = ORIENTED_EDGE ( 'NONE', *, *, #19703, .F. ) ;
#9266 = CARTESIAN_POINT ( 'NONE',  ( 25.75999999999999801, -2.208672634433321348E-15, 0.000000000000000000 ) ) ;
#9268 = CARTESIAN_POINT ( 'NONE',  ( -40.27879340802675046, -12.50360960397076404, 5.500000000000000000 ) ) ;
#9269 = CARTESIAN_POINT ( 'NONE',  ( 7.249760686538667009, -8.437262856154147173, -2.318425219014316419 ) ) ;
#9270 = CARTESIAN_POINT ( 'NONE',  ( -56.55840490054024627, 0.08005089788804982398, 1.499999999999999112 ) ) ;
#9271 = CYLINDRICAL_SURFACE ( 'NONE', #18887, 6.248999999999999666 ) ;
#9272 = AXIS2_PLACEMENT_3D ( 'NONE', #9726, #23276, #30819 ) ;
#9273 = CIRCLE ( 'NONE', #22023, 8.500000000000000000 ) ;
#9274 = DIRECTION ( 'NONE',  ( 8.281886410780508561E-17, 0.9659258262890682012, -0.2588190451025209060 ) ) ;
#9275 = CARTESIAN_POINT ( 'NONE',  ( 0.000000000000000000, 37.67766952966368876, 0.000000000000000000 ) ) ;
#9276 = CARTESIAN_POINT ( 'NONE',  ( 3.249999999999999556, 0.000000000000000000, 0.000000000000000000 ) ) ;
#9277 = AXIS2_PLACEMENT_3D ( 'NONE', #6585, #1922, #22138 ) ;
#9278 = EDGE_CURVE ( 'NONE', #18474, #2818, #29086, .T. ) ;
#9279 = EDGE_CURVE ( 'NONE', #29481, #11371, #21223, .T. ) ;
#9280 = FACE_OUTER_BOUND ( 'NONE', #14995, .T. ) ;
#9281 = CARTESIAN_POINT ( 'NONE',  ( 1.668773398854301785E-16, 1.946309384392590935, 4.616489984850538519 ) ) ;
#9282 = PLANE ( 'NONE',  #6508 ) ;
#9283 = CC_DESIGN_APPROVAL ( #7982, ( #10350 ) ) ;
#9284 = CARTESIAN_POINT ( 'NONE',  ( 0.7212197624700831255, -2.263408446301279131, -8.661246924805441338 ) ) ;
#9285 = CARTESIAN_POINT ( 'NONE',  ( -7.350050802731187716, -0.3135853898029607456, 2.983565686104819648 ) ) ;
#9286 = ORIENTED_EDGE ( 'NONE', *, *, #2545, .T. ) ;
#9287 = CARTESIAN_POINT ( 'NONE',  ( -7.537550801365592967, -3.368539882008727115, -1.828967928396028064 ) ) ;
#9288 = LINE ( 'NONE', #24658, #23143 ) ;
#9289 = CARTESIAN_POINT ( 'NONE',  ( -17.45597128428592981, 0.000000000000000000, 11.00000000000000000 ) ) ;
#9290 = CARTESIAN_POINT ( 'NONE',  ( 7.278212735265134015, -5.482579124931374004, 1.000000000000000000 ) ) ;
#9291 = ORIENTED_EDGE ( 'NONE', *, *, #11893, .T. ) ;
#9292 = CARTESIAN_POINT ( 'NONE',  ( 0.000000000000000000, 0.000000000000000000, 0.000000000000000000 ) ) ;
#9293 = CARTESIAN_POINT ( 'NONE',  ( 11.20269353100511367, -13.34333142745220613, -1.500000000000000000 ) ) ;
#9294 = VECTOR ( 'NONE', #11616, 1000.000000000000000 ) ;
#9295 = VERTEX_POINT ( 'NONE', #847 ) ;
#9296 = CARTESIAN_POINT ( 'NONE',  ( 0.2074580698797141576, -5.485259797753295530, 1.769984832060537139 ) ) ;
#9297 = PERSON_AND_ORGANIZATION ( #6766, #25292 ) ;
#9298 = DIRECTION ( 'NONE',  ( 0.000000000000000000, 0.000000000000000000, 1.000000000000000000 ) ) ;
#9299 = ORIENTED_EDGE ( 'NONE', *, *, #5684, .T. ) ;
#9300 = CARTESIAN_POINT ( 'NONE',  ( -4.436766851201613626, -8.315976708237174719, 1.500000000000000222 ) ) ;
#9301 = CARTESIAN_POINT ( 'NONE',  ( -31.57659242536668032, -21.43932300455408679, -1.500000000000000000 ) ) ;
#9302 = CARTESIAN_POINT ( 'NONE',  ( 54.96823639741650425, -6.181812932762141166, -4.275175838000669692 ) ) ;
#9303 = CARTESIAN_POINT ( 'NONE',  ( 23.32053031413095567, -17.41627278853254168, -1.661539697404067484 ) ) ;
#9304 = CARTESIAN_POINT ( 'NONE',  ( 107.8102081147311964, -16.09624553401235048, -1.444131124663050159 ) ) ;
#9305 = VERTEX_POINT ( 'NONE', #11024 ) ;
#9306 = APPROVAL_PERSON_ORGANIZATION ( #14954, #15523, #105 ) ;
#9307 = FACE_OUTER_BOUND ( 'NONE', #5244, .T. ) ;
#9308 = DIRECTION ( 'NONE',  ( -1.000000000000000000, 0.000000000000000000, 0.000000000000000000 ) ) ;
#9309 = CARTESIAN_POINT ( 'NONE',  ( 18.91048367622525106, -4.177835576467572309, -3.093621903261461359 ) ) ;
#9310 = ADVANCED_FACE ( 'NONE', ( #21556 ), #20474, .T. ) ;
#9312 = ORIENTED_EDGE ( 'NONE', *, *, #31294, .T. ) ;
#9311 = CARTESIAN_POINT ( 'NONE',  ( 25.56220348721820201, -1.341958225229829886E-11, -2.827203487218203914 ) ) ;
#9313 = DIRECTION ( 'NONE',  ( 0.000000000000000000, 0.000000000000000000, 1.000000000000000000 ) ) ;
#9314 = CARTESIAN_POINT ( 'NONE',  ( 33.89057010690738991, 19.51744974835125035, -2.472434150641027895 ) ) ;
#9315 = CARTESIAN_POINT ( 'NONE',  ( -0.5616989984784648282, -12.44624546261723985, -4.522129901861166701 ) ) ;
#9316 = CARTESIAN_POINT ( 'NONE',  ( 18.96091535642496240, -3.614110606601104614, -2.184956778830005053 ) ) ;
#9317 = DIRECTION ( 'NONE',  ( -0.4999999999999982236, -0.8660254037844397068, 0.000000000000000000 ) ) ;
#9318 = CARTESIAN_POINT ( 'NONE',  ( 7.249760686538667009, -0.8180878109962448352, 8.711672189281424394 ) ) ;
#9319 = AXIS2_PLACEMENT_3D ( 'NONE', #29147, #4075, #31829 ) ;
#9320 = DIRECTION ( 'NONE',  ( 0.000000000000000000, 0.9659258262890668689, 0.2588190451025257355 ) ) ;
#9321 = CARTESIAN_POINT ( 'NONE',  ( 10.57125986779756843, -4.681538312723523276, 0.8254815157535098091 ) ) ;
#9322 = CARTESIAN_POINT ( 'NONE',  ( -26.97533405509228999, 5.021485087457022267, 2.117863293439079531 ) ) ;
#9323 = VERTEX_POINT ( 'NONE', #26242 ) ;
#9324 = CARTESIAN_POINT ( 'NONE',  ( -15.12340757463330654, 0.000000000000000000, -1.000000000000000222 ) ) ;
#9325 = VERTEX_POINT ( 'NONE', #3177 ) ;
#9326 = B_SPLINE_CURVE_WITH_KNOTS ( 'NONE', 3,
 ( #26219, #3162, #21206, #30920, #829, #23375, #13319, #18379, #21056, #3019 ),
 .UNSPECIFIED., .F., .F.,
 ( 4, 2, 2, 2, 4 ),
 ( -4.729241382666856280E-06, 0.0005792517583992175863, 0.0008712422582901618731, 0.001017237508235635697, 0.001163232758181109629 ),
 .UNSPECIFIED. ) ;
#9327 = CARTESIAN_POINT ( 'NONE',  ( -7.804531657079157192, -1.883076972206379818, -2.325406398514292761 ) ) ;
#9328 = CARTESIAN_POINT ( 'NONE',  ( 3.499999999999999556, 0.000000000000000000, 0.000000000000000000 ) ) ;
#9329 = EDGE_CURVE ( 'NONE', #15836, #18404, #31767, .T. ) ;
#9330 = CARTESIAN_POINT ( 'NONE',  ( 29.35001421184127324, -4.582605737176272953, -4.522129901861162260 ) ) ;
#9331 = ORGANIZATION ( 'NAUO-ORG8', 'UNSPECIFIED', 'UNSPECIFIED' ) ;
#9332 = CARTESIAN_POINT ( 'NONE',  ( 25.43628654896337693, -17.54453578616444176, -1.000000000000000000 ) ) ;
#9333 = LINE ( 'NONE', #6819, #19956 ) ;
#9334 = ORIENTED_EDGE ( 'NONE', *, *, #1479, .T. ) ;
#9335 = CARTESIAN_POINT ( 'NONE',  ( 56.97280603064898941, -277.2763395528616002, 0.000000000000000000 ) ) ;
#9336 = EDGE_LOOP ( 'NONE', ( #30750, #6499, #8243, #11947, #1492, #15163, #20903, #15483, #20131, #7252, #18109, #23789, #24847, #29215, #1259, #8668, #18810, #8434, #22337 ) ) ;
#9337 = APPROVAL_DATE_TIME ( #14181, #12877 ) ;
#9338 = ADVANCED_FACE ( 'NONE', ( #6007 ), #31422, .T. ) ;
#9339 = CARTESIAN_POINT ( 'NONE',  ( 85.03565147854187956, -5.202094871745851279, 3.997237729527196137 ) ) ;
#9340 = B_SPLINE_CURVE_WITH_KNOTS ( 'NONE', 3,
 ( #12112, #12261, #15278, #28003, #4930, #15114, #22471, #5102 ),
 .UNSPECIFIED., .F., .F.,
 ( 4, 2, 2, 4 ),
 ( 0.000000000000000000, 0.5000000000000000000, 0.7500000000000000000, 1.000000000000000000 ),
 .UNSPECIFIED. ) ;
#9341 = CARTESIAN_POINT ( 'NONE',  ( -3.700050802731187805, 1.549418761218566143, -2.853674364686379583 ) ) ;
#9342 = CYLINDRICAL_SURFACE ( 'NONE', #12944, 5.010000000000000675 ) ;
#9343 = EDGE_CURVE ( 'NONE', #14512, #18387, #3388, .T. ) ;
#9344 = ORIENTED_EDGE ( 'NONE', *, *, #27894, .F. ) ;
#9345 = ORIENTED_EDGE ( 'NONE', *, *, #6160, .F. ) ;
#9346 = CARTESIAN_POINT ( 'NONE',  ( 24.25111450864415730, -3.256483526998273983E-15, 2.499999999999998668 ) ) ;
#9347 = DIRECTION ( 'NONE',  ( 0.8660254037844399289, -0.4999999999999978906, 0.000000000000000000 ) ) ;
#9348 = CARTESIAN_POINT ( 'NONE',  ( 25.10999999999999943, 1.942864903642424146, 1.573300977624592534 ) ) ;
#9349 = CARTESIAN_POINT ( 'NONE',  ( 8.533814948527936650, -14.05305963826104332, -1.499999999999999556 ) ) ;
#9351 = ORIENTED_EDGE ( 'NONE', *, *, #4743, .F. ) ;
#9350 = CARTESIAN_POINT ( 'NONE',  ( 7.064423659272766720, 3.748318449932021679, -7.906491560605039659 ) ) ;
#9352 = CARTESIAN_POINT ( 'NONE',  ( -4.187550801365593323, 0.3701630799359330593, -3.521866450007987037 ) ) ;
#9353 = CARTESIAN_POINT ( 'NONE',  ( 25.75999999999999801, -1.838216977691246972E-15, 3.024999999999999911 ) ) ;
#9354 = CARTESIAN_POINT ( 'NONE',  ( 102.5305753040692736, -0.1042037546421159255, 0.07017451552782062729 ) ) ;
#9356 = EDGE_CURVE ( 'NONE', #9547, #30308, #16346, .T. ) ;
#9355 = DIRECTION ( 'NONE',  ( 7.472768010112043792E-18, 0.08715574274766818563, -0.9961946980917447680 ) ) ;
#9357 = ORIENTED_EDGE ( 'NONE', *, *, #21003, .T. ) ;
#9359 = ORIENTED_EDGE ( 'NONE', *, *, #29310, .F. ) ;
#9358 = CARTESIAN_POINT ( 'NONE',  ( 2.542834076925224007, 1.635051133492022979E-17, 1.603031904926282891 ) ) ;
#9360 = EDGE_CURVE ( 'NONE', #7095, #30379, #31682, .T. ) ;
#9361 = DIRECTION ( 'NONE',  ( -0.000000000000000000, -0.000000000000000000, -1.000000000000000000 ) ) ;
#9362 = CARTESIAN_POINT ( 'NONE',  ( 3.529825581556927552E-16, 4.116875700062083254, 2.376879293651078751 ) ) ;
#9363 = EDGE_CURVE ( 'NONE', #25317, #22609, #11353, .T. ) ;
#9364 = CARTESIAN_POINT ( 'NONE',  ( -16.89591873025416646, 10.24026612823045035, 1.500000000000111910 ) ) ;
#9365 = CARTESIAN_POINT ( 'NONE',  ( -23.54713438637982748, 18.46223496596754288, 1.773004750130224627 ) ) ;
#9366 = DIRECTION ( 'NONE',  ( -0.000000000000000000, 0.000000000000000000, 1.000000000000000000 ) ) ;
#9367 = CARTESIAN_POINT ( 'NONE',  ( 5.887530180601098451, 7.076866030741313374, 4.515817126386032498 ) ) ;
#9368 = CARTESIAN_POINT ( 'NONE',  ( 3.499999999999999556, -2.652816298622381996, -5.657964889053610058 ) ) ;
#9369 = CARTESIAN_POINT ( 'NONE',  ( -3.787550801365593411, -0.3701630799359326152, 3.521866450007987037 ) ) ;
#9370 = ORIENTED_EDGE ( 'NONE', *, *, #1623, .F. ) ;
#9371 = CARTESIAN_POINT ( 'NONE',  ( 56.97280603064898941, -277.2763395528616002, -0.4463807625373608645 ) ) ;
#9372 = ORIENTED_EDGE ( 'NONE', *, *, #7423, .F. ) ;
#9373 = EDGE_CURVE ( 'NONE', #29856, #18979, #29529, .T. ) ;
#9374 = DIRECTION ( 'NONE',  ( 1.000000000000000000, -0.000000000000000000, -0.000000000000000000 ) ) ;
#9375 = CARTESIAN_POINT ( 'NONE',  ( 29.38825086720287771, -3.456623792456554156, -2.713652344655542503 ) ) ;
#9376 = CARTESIAN_POINT ( 'NONE',  ( -34.48223484310472031, 0.5000000000000000000, -2.482234843104711430 ) ) ;
#9377 = VERTEX_POINT ( 'NONE', #13521 ) ;
#9378 =( BOUNDED_SURFACE ( )  B_SPLINE_SURFACE ( 3, 1, ( 
 ( #26644, #18808 ),
 ( #6109, #13919 ),
 ( #16292, #26502 ),
 ( #3603, #10783 ) ),
 .UNSPECIFIED., .F., .F., .F. ) 
 B_SPLINE_SURFACE_WITH_KNOTS ( ( 4, 4 ),
 ( 2, 2 ),
 ( 0.000000000000000000, 1.000000000000000000 ),
 ( 0.000000000000000000, 1.000000000000000000 ),
 .UNSPECIFIED. ) 
 GEOMETRIC_REPRESENTATION_ITEM ( )  RATIONAL_B_SPLINE_SURFACE ( (
 ( 1.000000000000000000, 1.000000000000000000),
 ( 0.6539698177806696489, 0.6539698177806696489),
 ( 0.6539698177806696489, 0.6539698177806696489),
 ( 1.000000000000000000, 1.000000000000000000) ) ) 
 REPRESENTATION_ITEM ( '' )  SURFACE ( )  );
#9379 = DIRECTION ( 'NONE',  ( 0.9816271834476637537, 0.000000000000000000, -0.1908089953765453872 ) ) ;
#9380 = ORIENTED_EDGE ( 'NONE', *, *, #10100, .T. ) ;
#9381 = DIRECTION ( 'NONE',  ( 0.000000000000000000, 0.000000000000000000, -1.000000000000000000 ) ) ;
#9383 = VERTEX_POINT ( 'NONE', #28900 ) ;
#9382 = CARTESIAN_POINT ( 'NONE',  ( 18.86040190548595419, -4.737649260393223649, -3.995970707755712947 ) ) ;
#9384 = EDGE_LOOP ( 'NONE', ( #25734, #932, #11183, #27876 ) ) ;
#9385 = EDGE_CURVE ( 'NONE', #8778, #5623, #6172, .T. ) ;
#9386 = DIRECTION ( 'NONE',  ( -0.000000000000000000, -0.000000000000000000, -1.000000000000000000 ) ) ;
#9387 = FACE_OUTER_BOUND ( 'NONE', #3081, .T. ) ;
#9389 = ORIENTED_EDGE ( 'NONE', *, *, #22705, .F. ) ;
#9388 = CARTESIAN_POINT ( 'NONE',  ( -0.3438197445875938452, -15.06918786293965873, -1.500000000000000000 ) ) ;
#9390 = LINE ( 'NONE', #29800, #18293 ) ;
#9391 = CARTESIAN_POINT ( 'NONE',  ( 22.48500000000000298, -2.486304738420683780, 0.2613211581691335383 ) ) ;
#9392 = FACE_OUTER_BOUND ( 'NONE', #28631, .T. ) ;
#9393 = EDGE_CURVE ( 'NONE', #25587, #7938, #31512, .T. ) ;
#9394 = DIRECTION ( 'NONE',  ( -1.000000000000000000, -0.000000000000000000, -0.000000000000000000 ) ) ;
#9396 = ORIENTED_EDGE ( 'NONE', *, *, #16311, .F. ) ;
#9395 = CARTESIAN_POINT ( 'NONE',  ( 107.9493514742475071, -17.34003594554901539, -4.558238555758752142 ) ) ;
#9397 = EDGE_CURVE ( 'NONE', #11731, #24612, #29951, .T. ) ;
#9398 = CARTESIAN_POINT ( 'NONE',  ( 2.857988133323936530, -7.318787950819720223, 6.150950518044190574 ) ) ;
#9399 = CARTESIAN_POINT ( 'NONE',  ( 23.48500000273119070, 0.2613211581691317065, 2.486304738420681559 ) ) ;
#9400 = CARTESIAN_POINT ( 'NONE',  ( 23.42250000136559862, 1.913930629741522838, -2.363507492473150062 ) ) ;
#9401 = FACE_OUTER_BOUND ( 'NONE', #9108, .T. ) ;
#9402 = DIRECTION ( 'NONE',  ( -1.000000000000000000, 0.000000000000000000, 0.000000000000000000 ) ) ;
#9403 = CARTESIAN_POINT ( 'NONE',  ( 0.7632845268398871230, 8.734705317681626724, -0.4999240074894737984 ) ) ;
#9404 = ORIENTED_EDGE ( 'NONE', *, *, #31164, .F. ) ;
#9405 = CARTESIAN_POINT ( 'NONE',  ( -33.89057010690739702, 19.51744974835125035, 2.472434150641035444 ) ) ;
#9406 = CARTESIAN_POINT ( 'NONE',  ( 4.749760686538667009, -1.391664247347174754, -7.892520144992448472 ) ) ;
#9407 = DIRECTION ( 'NONE',  ( -1.000000000000000000, 2.473959037481237219E-13, 0.000000000000000000 ) ) ;
#9408 = ORIENTED_EDGE ( 'NONE', *, *, #14129, .T. ) ;
#9409 = EDGE_CURVE ( 'NONE', #4399, #12332, #19948, .T. ) ;
#9410 = CC_DESIGN_PERSON_AND_ORGANIZATION_ASSIGNMENT ( #19883, #22057, ( #17797 ) ) ;
#9411 = DIRECTION ( 'NONE',  ( -1.000000000000000000, 0.000000000000000000, 0.000000000000000000 ) ) ;
#9412 = CARTESIAN_POINT ( 'NONE',  ( 3.673334745431914072, 0.0007210401945499157229, -1.066984883845929932 ) ) ;
#9413 = VERTEX_POINT ( 'NONE', #9332 ) ;
#9414 = DIRECTION ( 'NONE',  ( -1.000000000000000000, -0.000000000000000000, 0.000000000000000000 ) ) ;
#9415 = VERTEX_POINT ( 'NONE', #21863 ) ;
#9416 = ORIENTED_EDGE ( 'NONE', *, *, #13858, .F. ) ;
#9418 = VERTEX_POINT ( 'NONE', #4158 ) ;
#9417 = CARTESIAN_POINT ( 'NONE',  ( 19.72835230534419537, -21.42792461751441735, -1.670332045613319050 ) ) ;
#9419 = ORIENTED_EDGE ( 'NONE', *, *, #3629, .T. ) ;
#9420 = CARTESIAN_POINT ( 'NONE',  ( 10.00000000000000000, 1.625881193364696831, 4.467071865485476856 ) ) ;
#9421 = EDGE_CURVE ( 'NONE', #14956, #20879, #16857, .T. ) ;
#9422 = ORIENTED_EDGE ( 'NONE', *, *, #15212, .F. ) ;
#9423 = CARTESIAN_POINT ( 'NONE',  ( 4.749760686538667009, -4.007137495034764463, -6.940565734314639634 ) ) ;
#9424 = CARTESIAN_POINT ( 'NONE',  ( -2.511343449419940921, 1.323625320507516134, 3.284597389079960461 ) ) ;
#9426 = ORIENTED_EDGE ( 'NONE', *, *, #30961, .F. ) ;
#9425 = CARTESIAN_POINT ( 'NONE',  ( 23.86142584454780646, -3.703306447632950249, -1.529339877351986621 ) ) ;
#9427 = DIRECTION ( 'NONE',  ( -1.000000000000000000, 0.000000000000000000, 0.000000000000000000 ) ) ;
#9428 = FACE_OUTER_BOUND ( 'NONE', #22066, .T. ) ;
#9429 = CARTESIAN_POINT ( 'NONE',  ( 23.29750000136559862, -0.3178988483021076838, -3.024605502323848949 ) ) ;
#9430 = CARTESIAN_POINT ( 'NONE',  ( 107.5951944728457477, -19.46454432635805532, 3.536284406030664407 ) ) ;
#9431 = CYLINDRICAL_SURFACE ( 'NONE', #23086, 2.999999999999999112 ) ;
#9432 = DIRECTION ( 'NONE',  ( -1.000000000000000000, 0.000000000000000000, 0.000000000000000000 ) ) ;
#9433 = CARTESIAN_POINT ( 'NONE',  ( 0.1574692421720941260, 7.841623826006872910, -7.165523657698227744 ) ) ;
#9434 = CARTESIAN_POINT ( 'NONE',  ( 34.48223484310472031, 0.5000000000000000000, -2.552009564962230304 ) ) ;
#9435 = FACE_OUTER_BOUND ( 'NONE', #2541, .T. ) ;
#9436 = CARTESIAN_POINT ( 'NONE',  ( 12.44989959798877877, 0.000000000000000000, 2.482234843104759392 ) ) ;
#9437 = B_SPLINE_CURVE_WITH_KNOTS ( 'NONE', 3,
 ( #28761, #31613, #1363, #18725, #29257, #26741, #29419, #11048, #21732, #19224 ),
 .UNSPECIFIED., .F., .F.,
 ( 4, 2, 2, 2, 4 ),
 ( 1.968338519012299431E-07, 0.0005467928198071732564, 0.001093388805762445307, 0.001639984791717717357, 0.002186580777672989841 ),
 .UNSPECIFIED. ) ;
#9438 = CARTESIAN_POINT ( 'NONE',  ( 48.06508596181272708, -7.548662730768715079, 4.522129901861163148 ) ) ;
#9439 = EDGE_CURVE ( 'NONE', #22736, #9882, #29000, .T. ) ;
#9440 = CARTESIAN_POINT ( 'NONE',  ( -7.000050802731188071, -0.9222479816126459840, -3.113457007523259268 ) ) ;
#9441 = ORIENTED_EDGE ( 'NONE', *, *, #7676, .F. ) ;
#9442 = CARTESIAN_POINT ( 'NONE',  ( -3.450050800000000084, 2.853674364686379583, 1.549418761218565921 ) ) ;
#9443 = CARTESIAN_POINT ( 'NONE',  ( 21.32535692059145660, -21.82495604402121003, -1.318256435726663955 ) ) ;
#9444 = CARTESIAN_POINT ( 'NONE',  ( -4.050050802731187005, -2.331437884370912705, 1.887961173149512062 ) ) ;
#9445 = VERTEX_POINT ( 'NONE', #1650 ) ;
#9446 = CARTESIAN_POINT ( 'NONE',  ( 0.000000000000000000, 0.000000000000000000, 0.000000000000000000 ) ) ;
#9447 = CARTESIAN_POINT ( 'NONE',  ( 7.189332377417054332, -9.531173777828719551, -1.500000000000000666 ) ) ;
#9448 = EDGE_LOOP ( 'NONE', ( #10488, #11268, #1170, #19198 ) ) ;
#9449 = CARTESIAN_POINT ( 'NONE',  ( 10.98820359953467829, -14.84698140496809415, 1.499999999999999112 ) ) ;
#9450 = APPROVAL_ROLE ( '' ) ;
#9451 = DIRECTION ( 'NONE',  ( -1.000000000000000000, -0.000000000000000000, -0.000000000000000000 ) ) ;
#9452 = ORIENTED_EDGE ( 'NONE', *, *, #23315, .T. ) ;
#9453 = CARTESIAN_POINT ( 'NONE',  ( 9.350000000000001421, 0.000000000000000000, -1.000000000000000000 ) ) ;
#9454 = EDGE_CURVE ( 'NONE', #12752, #32996, #31171, .T. ) ;
#9455 = ADVANCED_FACE ( 'NONE', ( #17007 ), #29584, .T. ) ;
#9456 = CARTESIAN_POINT ( 'NONE',  ( 13.78291618757655712, 7.586155849071186452, -1.050000000000000044 ) ) ;
#9457 = CARTESIAN_POINT ( 'NONE',  ( 102.4197966183807296, -3.949332865022705086, -4.074610060379797005 ) ) ;
#9458 = CARTESIAN_POINT ( 'NONE',  ( -56.71071518287084245, 0.7496615022747066259, 1.500000000000000000 ) ) ;
#9459 = CARTESIAN_POINT ( 'NONE',  ( 16.36487458112951643, 19.37645981759113312, 4.629213727441584325 ) ) ;
#9460 = EDGE_CURVE ( 'NONE', #31644, #15187, #6033, .T. ) ;
#9461 = VERTEX_POINT ( 'NONE', #32271 ) ;
#9462 = CARTESIAN_POINT ( 'NONE',  ( 8.870145747188287189, 0.000000000000000000, 1.000000000000000000 ) ) ;
#9463 = CARTESIAN_POINT ( 'NONE',  ( 23.11934981620009921, -21.92529594990386599, -1.124851831741316754 ) ) ;
#9464 = DIRECTION ( 'NONE',  ( 1.000000000000000000, -0.000000000000000000, -0.000000000000000000 ) ) ;
#9466 = ORIENTED_EDGE ( 'NONE', *, *, #25932, .F. ) ;
#9465 = FACE_OUTER_BOUND ( 'NONE', #1926, .T. ) ;
#9467 = CARTESIAN_POINT ( 'NONE',  ( 2.274274201625327230, 0.000000000000000000, 0.000000000000000000 ) ) ;
#9468 = PRODUCT_DEFINITION_SHAPE ( 'NONE', 'NONE',  #25774 ) ;
#9469 = LINE ( 'NONE', #17165, #28858 ) ;
#9470 = CARTESIAN_POINT ( 'NONE',  ( 13.65718777918027271, -19.09288791508984318, -4.522129901861166701 ) ) ;
#9471 = CYLINDRICAL_SURFACE ( 'NONE', #22482, 2.999999999999999112 ) ;
#9472 = DIRECTION ( 'NONE',  ( -8.326672684688674053E-17, -0.3746065934159164001, 0.9271838545667857590 ) ) ;
#9473 = CARTESIAN_POINT ( 'NONE',  ( 6.880160201030087741, 0.6895871680713152596, 8.703862158141010497 ) ) ;
#9474 = CARTESIAN_POINT ( 'NONE',  ( -23.54713438637982748, 18.90773822806172433, 2.000000000000000000 ) ) ;
#9475 = FACE_OUTER_BOUND ( 'NONE', #29311, .T. ) ;
#9476 = CARTESIAN_POINT ( 'NONE',  ( 25.75999999999999801, -2.208672634433321348E-15, 0.000000000000000000 ) ) ;
#9477 = ORIENTED_EDGE ( 'NONE', *, *, #10053, .T. ) ;
#9478 = CARTESIAN_POINT ( 'NONE',  ( 7.064632918400242545, 2.318425219014231597, 8.437262856154173818 ) ) ;
#9479 = ORIENTED_EDGE ( 'NONE', *, *, #16510, .T. ) ;
#9480 = CARTESIAN_POINT ( 'NONE',  ( -5.854531657079158791, 2.846291840500173365, 1.545410377633946952 ) ) ;
#9481 = CARTESIAN_POINT ( 'NONE',  ( 1.750000000000000222, 8.357095590591338663, -1.552080310331533486 ) ) ;
#9482 = B_SPLINE_CURVE_WITH_KNOTS ( 'NONE', 3,
 ( #31756, #13183, #18391, #21368 ),
 .UNSPECIFIED., .F., .F.,
 ( 4, 4 ),
 ( -6.746902117120830621E-06, 2.872315617951276588E-05 ),
 .UNSPECIFIED. ) ;
#9483 = CYLINDRICAL_SURFACE ( 'NONE', #15127, 3.000000000000000444 ) ;
#9484 = DIRECTION ( 'NONE',  ( 0.000000000000000000, 0.9945218953682729568, 0.1045284632676570513 ) ) ;
#9485 = CARTESIAN_POINT ( 'NONE',  ( 0.000000000000000000, 7.944914065997111585, 7.533794289458081828 ) ) ;
#9486 = ORIENTED_EDGE ( 'NONE', *, *, #1830, .T. ) ;
#9487 = CARTESIAN_POINT ( 'NONE',  ( 10.55147673363119232, -4.116875700062100130, 2.376879293651050329 ) ) ;
#9488 = EDGE_CURVE ( 'NONE', #31265, #28329, #12757, .T. ) ;
#9489 = ORIENTED_EDGE ( 'NONE', *, *, #28864, .F. ) ;
#9490 = SHAPE_DEFINITION_REPRESENTATION ( #25521, #13478 ) ;
#9491 = CARTESIAN_POINT ( 'NONE',  ( 40.88396545762024203, -6.891784699261402913, 4.001040184481850837 ) ) ;
#9492 = EDGE_CURVE ( 'NONE', #2199, #7501, #32345, .T. ) ;
#9493 = EDGE_CURVE ( 'NONE', #21158, #1567, #15100, .T. ) ;
#9494 = CARTESIAN_POINT ( 'NONE',  ( 9.350000000000001421, 0.000000000000000000, -1.000000000000000000 ) ) ;
#9496 = CARTESIAN_POINT ( 'NONE',  ( 0.000000000000000000, 0.000000000000000000, 0.000000000000000000 ) ) ;
#9495 = CARTESIAN_POINT ( 'NONE',  ( 7.064632940817598517, 3.748318449932297014, 7.906491560603678082 ) ) ;
#9497 = ORIENTED_EDGE ( 'NONE', *, *, #1402, .F. ) ;
#9498 = DIRECTION ( 'NONE',  ( 0.000000000000000000, 0.9063077870366529343, -0.4226182617406930020 ) ) ;
#9499 = CARTESIAN_POINT ( 'NONE',  ( -2.712550801365592790, -3.675193018007245627, 1.088641768524163389 ) ) ;
#9500 = CARTESIAN_POINT ( 'NONE',  ( 22.86000000000000298, 1.573300977624590313, -1.942864903642426144 ) ) ;
#9501 = CARTESIAN_POINT ( 'NONE',  ( 1.653263284061800453, -10.31364870257782762, -1.500000000000000222 ) ) ;
#9503 = ORIENTED_EDGE ( 'NONE', *, *, #12064, .T. ) ;
#9502 = FACE_OUTER_BOUND ( 'NONE', #10974, .T. ) ;
#9504 = CARTESIAN_POINT ( 'NONE',  ( -4.437550801365594211, -3.675193018007246071, 1.088641768524163167 ) ) ;
#9505 = DIRECTION ( 'NONE',  ( -0.9993908270190956511, -0.03489949670250350189, 1.734723475976808475E-15 ) ) ;
#9506 = CARTESIAN_POINT ( 'NONE',  ( 10.56870887191539587, 1.625881193364757449, -4.467071865485455540 ) ) ;
#9507 = SPHERICAL_SURFACE ( 'NONE', #31178, 0.5000000000000000000 ) ;
#9508 = VERTEX_POINT ( 'NONE', #6979 ) ;
#9510 = EDGE_LOOP ( 'NONE', ( #23887, #32510, #21007, #2010, #16606, #5004 ) ) ;
#9509 = PLANE ( 'NONE',  #5381 ) ;
#9511 = DIRECTION ( 'NONE',  ( 1.000000000000000000, 0.000000000000000000, 0.000000000000000000 ) ) ;
#9512 = CARTESIAN_POINT ( 'NONE',  ( 3.499999999999999556, 0.000000000000000000, 0.000000000000000000 ) ) ;
#9513 = CARTESIAN_POINT ( 'NONE',  ( -17.31779044994511096, 15.08866638674220084, 1.500000000000000000 ) ) ;
#9514 = CARTESIAN_POINT ( 'NONE',  ( -6.207304909706597762, -1.062355717592095017, -2.999999999999999556 ) ) ;
#9515 = CARTESIAN_POINT ( 'NONE',  ( 10.32252699260177131, -19.71148491318491480, -1.500000000000157208 ) ) ;
#9516 = CARTESIAN_POINT ( 'NONE',  ( 6.038145208238975492, 7.104833038995711725, 4.620191422127150283 ) ) ;
#9517 = EDGE_CURVE ( 'NONE', #18225, #26613, #19698, .T. ) ;
#9518 = CARTESIAN_POINT ( 'NONE',  ( 41.34457103395083521, -4.143788916012135282, 1.529340246549222737 ) ) ;
#9519 = LINE ( 'NONE', #32958, #15106 ) ;
#9520 = ORIENTED_EDGE ( 'NONE', *, *, #7638, .T. ) ;
#9521 = DIRECTION ( 'NONE',  ( -1.000000000000000000, 0.000000000000000000, 0.000000000000000000 ) ) ;
#9522 = ORIENTED_EDGE ( 'NONE', *, *, #22371, .T. ) ;
#9523 = EDGE_CURVE ( 'NONE', #17424, #25915, #17264, .T. ) ;
#9524 = DIRECTION ( 'NONE',  ( -1.000000000000000000, 8.574039729943017111E-17, -0.000000000000000000 ) ) ;
#9525 = CARTESIAN_POINT ( 'NONE',  ( -23.34999999999999432, -10.96966150227470393, -22.25000000000000000 ) ) ;
#9526 = ADVANCED_FACE ( 'NONE', ( #4007 ), #14005, .F. ) ;
#9527 = CARTESIAN_POINT ( 'NONE',  ( 10.00000000000000000, 2.376879293651121383, -4.116875700062057497 ) ) ;
#9528 = ADVANCED_FACE ( 'NONE', ( #11516 ), #31921, .F. ) ;
#9529 = ORIENTED_EDGE ( 'NONE', *, *, #8162, .F. ) ;
#9530 = CARTESIAN_POINT ( 'NONE',  ( 3.499999999999999556, 0.000000000000000000, 0.000000000000000000 ) ) ;
#9531 = PERSON ( 'NAUO-PER2', 'UNSPECIFIED', 'UNSPECIFIED', ('UNSPECIFIED'), ('UNSPECIFIED'), ('UNSPECIFIED') ) ;
#9532 = ORIENTED_EDGE ( 'NONE', *, *, #26274, .T. ) ;
#9533 = DIRECTION ( 'NONE',  ( 0.000000000000000000, 0.000000000000000000, -1.000000000000000000 ) ) ;
#9535 = EDGE_LOOP ( 'NONE', ( #7284, #27539, #7441, #19358 ) ) ;
#9534 = CARTESIAN_POINT ( 'NONE',  ( 84.96577320347208229, -4.062152178867207475, -3.998505472924086313 ) ) ;
#9536 = EDGE_CURVE ( 'NONE', #29208, #8502, #15181, .T. ) ;
#9537 = ORIENTED_EDGE ( 'NONE', *, *, #10127, .F. ) ;
#9538 = CARTESIAN_POINT ( 'NONE',  ( 23.36000000000000298, -1.573300977624594976, 1.942864903642425700 ) ) ;
#9539 = CARTESIAN_POINT ( 'NONE',  ( 69.09268213438589612, -2.232183665269761086, 0.07017451552782173751 ) ) ;
#9541 = ORIENTED_EDGE ( 'NONE', *, *, #2689, .T. ) ;
#9540 = DIRECTION ( 'NONE',  ( 0.000000000000000000, -0.2588190451025251804, 0.9659258262890670910 ) ) ;
#9542 = CARTESIAN_POINT ( 'NONE',  ( 25.73836023340754409, 18.89938647777091418, -1.500000000000000000 ) ) ;
#9543 = CARTESIAN_POINT ( 'NONE',  ( 0.000000000000000000, 0.000000000000000000, 0.000000000000000000 ) ) ;
#9544 = CARTESIAN_POINT ( 'NONE',  ( 3.249999999999999556, 0.000000000000000000, 0.000000000000000000 ) ) ;
#9545 = CARTESIAN_POINT ( 'NONE',  ( 7.594557537343171738, -2.555973540833195390, -1.500000000000000000 ) ) ;
#9547 = VERTEX_POINT ( 'NONE', #28208 ) ;
#9546 = CARTESIAN_POINT ( 'NONE',  ( 107.5140540107968548, -18.29027999154679307, -5.137983268504266121 ) ) ;
#9548 = DIRECTION ( 'NONE',  ( 0.000000000000000000, 1.000000000000000000, 0.000000000000000000 ) ) ;
#9549 = EDGE_CURVE ( 'NONE', #7869, #12104, #19162, .T. ) ;
#9550 = DIRECTION ( 'NONE',  ( 0.000000000000000000, -0.9961946980917461003, 0.08715574274765135188 ) ) ;
#9551 = CARTESIAN_POINT ( 'NONE',  ( 25.73500000136559507, 1.570731468192929858, 2.892927487894329186 ) ) ;
#9552 = FACE_OUTER_BOUND ( 'NONE', #6254, .T. ) ;
#9553 = CARTESIAN_POINT ( 'NONE',  ( 26.13024263984371842, 21.17433810686647533, -4.621439243524461560 ) ) ;
#9554 = ORIENTED_EDGE ( 'NONE', *, *, #16072, .F. ) ;
#9555 = DIRECTION ( 'NONE',  ( -0.1437473352844943209, 0.000000000000000000, 0.9896144216807913896 ) ) ;
#9556 = CARTESIAN_POINT ( 'NONE',  ( 34.92557263839314885, 0.5000000000000000000, -2.487612133692604921 ) ) ;
#9557 = CARTESIAN_POINT ( 'NONE',  ( -7.237550801365593145, 3.675193018007246959, -1.088641768524161391 ) ) ;
#9558 = ORIENTED_EDGE ( 'NONE', *, *, #20518, .T. ) ;
#9559 = VECTOR ( 'NONE', #24102, 1000.000000000000114 ) ;
#9560 =( BOUNDED_CURVE ( )  B_SPLINE_CURVE ( 3, ( #14200, #1515, #16881, #14706 ),
 .UNSPECIFIED., .F., .F. ) 
 B_SPLINE_CURVE_WITH_KNOTS ( ( 4, 4 ),
 ( 4.712388980383416914, 4.904375198102664868 ),
 .UNSPECIFIED. ) 
 CURVE ( )  GEOMETRIC_REPRESENTATION_ITEM ( )  RATIONAL_B_SPLINE_CURVE ( ( 1.000000000000000000, 0.9969307989114565283, 0.9969307989114565283, 1.000000000000000000 ) ) 
 REPRESENTATION_ITEM ( '' )  );
#9561 = FACE_OUTER_BOUND ( 'NONE', #25660, .T. ) ;
#9562 = EDGE_CURVE ( 'NONE', #2818, #30095, #708, .T. ) ;
#9563 = CARTESIAN_POINT ( 'NONE',  ( 2.648464616715308306, 0.1990047044050247960, -1.630908343631500168 ) ) ;
#9564 = ORIENTED_EDGE ( 'NONE', *, *, #15452, .F. ) ;
#9565 = CARTESIAN_POINT ( 'NONE',  ( 108.4602224094689547, 20.74085989589476497, 1.491071325085251864 ) ) ;
#9566 = EDGE_CURVE ( 'NONE', #16376, #6370, #20182, .T. ) ;
#9567 = ORIENTED_EDGE ( 'NONE', *, *, #13071, .F. ) ;
#9568 = ORIENTED_EDGE ( 'NONE', *, *, #12708, .F. ) ;
#9569 = CARTESIAN_POINT ( 'NONE',  ( -2.715612589025598211, -0.5453662152015974485, 1.748464016170372393 ) ) ;
#9571 = EDGE_LOOP ( 'NONE', ( #594, #23018, #5676, #8204 ) ) ;
#9570 = DIRECTION ( 'NONE',  ( 0.000000000000000000, 0.2079116908177532919, 0.9781476007338070211 ) ) ;
#9572 = VERTEX_POINT ( 'NONE', #30905 ) ;
#9573 = CARTESIAN_POINT ( 'NONE',  ( 23.04750000136559862, -3.024605502323851169, 0.3178988483021052969 ) ) ;
#9574 = EDGE_CURVE ( 'NONE', #7938, #926, #18576, .T. ) ;
#9576 = ORIENTED_EDGE ( 'NONE', *, *, #30491, .F. ) ;
#9575 = CIRCLE ( 'NONE', #26671, 8.749000000000002331 ) ;
#9577 = CARTESIAN_POINT ( 'NONE',  ( 0.7632845268398872340, -2.223716399045631231, 8.461683424509299556 ) ) ;
#9579 = ORIENTED_EDGE ( 'NONE', *, *, #30965, .F. ) ;
#9578 = CARTESIAN_POINT ( 'NONE',  ( 23.84149738812702779, -4.050734785793495440, -2.184956778827896962 ) ) ;
#9580 = CIRCLE ( 'NONE', #14926, 5.010000000000000675 ) ;
#9581 = LINE ( 'NONE', #32863, #20278 ) ;
#9582 = CARTESIAN_POINT ( 'NONE',  ( 0.000000000000000000, -4.057423117305330784, -8.475820894093018865 ) ) ;
#9583 = CARTESIAN_POINT ( 'NONE',  ( 24.86000000136559862, -0.9349337715887248157, 3.156283516753367824 ) ) ;
#9584 = DIRECTION ( 'NONE',  ( -1.000000000000000000, 8.574039729943018344E-17, 0.000000000000000000 ) ) ;
#9585 = ADVANCED_FACE ( 'NONE', ( #30755 ), #12511, .T. ) ;
#9586 = VECTOR ( 'NONE', #22158, 1000.000000000000000 ) ;
#9587 = CARTESIAN_POINT ( 'NONE',  ( 17.84081991000783063, -19.48375781953909325, -5.485967528433938867 ) ) ;
#9588 = CARTESIAN_POINT ( 'NONE',  ( 107.3476768466315150, -15.88628154573193463, -1.500000000000000444 ) ) ;
#9589 = CARTESIAN_POINT ( 'NONE',  ( 0.3045633657612876743, 7.698316278340462837, -6.808202580038895668 ) ) ;
#9590 = DIRECTION ( 'NONE',  ( -0.000000000000000000, 0.9063077870366497146, -0.4226182617406997744 ) ) ;
#9591 = CARTESIAN_POINT ( 'NONE',  ( -0.2493515011842071527, -1.403010508276806068, 5.485967528433933538 ) ) ;
#9592 = CARTESIAN_POINT ( 'NONE',  ( 0.08467178533536702523, 9.416764032208575941, 5.239665997527495733 ) ) ;
#9593 = CIRCLE ( 'NONE', #20834, 0.4999999999999996669 ) ;
#9594 = CARTESIAN_POINT ( 'NONE',  ( 84.37491783462850492, -2.359815117480457136, -0.07017451552781628354 ) ) ;
#9595 = B_SPLINE_CURVE_WITH_KNOTS ( 'NONE', 3,
 ( #3181, #23554, #19199, #14503, #26904, #27057, #24224, #21866, #32425, #3836 ),
 .UNSPECIFIED., .F., .F.,
 ( 4, 2, 2, 2, 4 ),
 ( 0.000000000000000000, 0.0009905218478212184617, 0.001981043695642436923, 0.002971565543463655385, 0.003962087391284873847 ),
 .UNSPECIFIED. ) ;
#9596 = CARTESIAN_POINT ( 'NONE',  ( -23.54713438637982748, 10.61651369059875272, 9.545881648375194928 ) ) ;
#9597 = CARTESIAN_POINT ( 'NONE',  ( -6.900050802731187538, 1.549418761218566143, -2.853674364686379583 ) ) ;
#9598 = EDGE_LOOP ( 'NONE', ( #14318, #26629, #14340, #32343, #173, #4804 ) ) ;
#9599 = CARTESIAN_POINT ( 'NONE',  ( -4.650050799999999818, -2.853674364686378695, -1.549418761218566809 ) ) ;
#9600 = AXIS2_PLACEMENT_3D ( 'NONE', #29253, #6337, #29757 ) ;
#9601 = CIRCLE ( 'NONE', #4271, 6.248999999999999666 ) ;
#9602 = B_SPLINE_CURVE_WITH_KNOTS ( 'NONE', 3,
 ( #27050, #29083, #1153, #26563, #13820, #8670, #28896, #29387, #18886, #6003 ),
 .UNSPECIFIED., .F., .F.,
 ( 4, 2, 2, 2, 4 ),
 ( 2.740849916244211241E-07, 0.0005478761651001725578, 0.001095478245208722241, 0.001643080325317271707, 0.002190682405425821606 ),
 .UNSPECIFIED. ) ;
#9603 = CARTESIAN_POINT ( 'NONE',  ( 4.749760686538667009, -4.007137495034861274, 6.940565734314584567 ) ) ;
#9604 = EDGE_CURVE ( 'NONE', #16071, #442, #625, .T. ) ;
#9605 = CARTESIAN_POINT ( 'NONE',  ( -4.100050802731187716, -1.549418761218565255, 2.853674364686380471 ) ) ;
#9606 = VERTEX_POINT ( 'NONE', #23695 ) ;
#9607 = DIRECTION ( 'NONE',  ( 1.000000000000000000, 0.000000000000000000, 0.000000000000000000 ) ) ;
#9608 = CARTESIAN_POINT ( 'NONE',  ( 34.99999999999998579, 0.5000000000000000000, 2.982234843104954791 ) ) ;
#9609 = VECTOR ( 'NONE', #20136, 1000.000000000000000 ) ;
#9610 = ORIENTED_EDGE ( 'NONE', *, *, #27391, .F. ) ;
#9611 = CARTESIAN_POINT ( 'NONE',  ( 101.7323099454754072, -3.043813463936519526, -4.171867813696918503 ) ) ;
#9612 = PERSON_AND_ORGANIZATION_ROLE ( 'creator' ) ;
#9613 = CARTESIAN_POINT ( 'NONE',  ( -3.122314033877883927E-16, -3.641590349731949505, 3.055657119358789142 ) ) ;
#9614 = ORIENTED_EDGE ( 'NONE', *, *, #18500, .F. ) ;
#9615 = CARTESIAN_POINT ( 'NONE',  ( -1.924689738998526689, -13.55751938318336514, 1.500000000000000222 ) ) ;
#9616 = ORIENTED_EDGE ( 'NONE', *, *, #28994, .T. ) ;
#9617 = DIRECTION ( 'NONE',  ( 1.000000000000000000, 0.000000000000000000, 0.000000000000000000 ) ) ;
#9618 = CARTESIAN_POINT ( 'NONE',  ( 18.79826502154305601, -5.432214915643744924, -4.312042181587000478 ) ) ;
#9619 = PLANE ( 'NONE',  #8067 ) ;
#9620 = CARTESIAN_POINT ( 'NONE',  ( 107.8717334959383010, -16.22235636682134441, -1.414040860180981740 ) ) ;
#9621 = ORIENTED_EDGE ( 'NONE', *, *, #26751, .T. ) ;
#9622 = AXIS2_PLACEMENT_3D ( 'NONE', #19396, #4516, #6991 ) ;
#9623 = CARTESIAN_POINT ( 'NONE',  ( 7.249760686538667009, -7.530955069117533540, 2.741043480754901118 ) ) ;
#9624 = DIRECTION ( 'NONE',  ( 0.000000000000000000, 0.000000000000000000, 1.000000000000000000 ) ) ;
#9626 = EDGE_CURVE ( 'NONE', #29952, #29340, #13495, .T. ) ;
#9625 = AXIS2_PLACEMENT_3D ( 'NONE', #21408, #11050, #29110 ) ;
#9627 = ORIENTED_EDGE ( 'NONE', *, *, #24276, .T. ) ;
#9628 = APPROVAL ( #28597, 'UNSPECIFIED' ) ;
#9629 = DIRECTION ( 'NONE',  ( 0.000000000000000000, 0.000000000000000000, 1.000000000000000000 ) ) ;
#9630 = CIRCLE ( 'NONE', #22457, 12.49867430706168570 ) ;
#9631 = LINE ( 'NONE', #22199, #14951 ) ;
#9632 = CARTESIAN_POINT ( 'NONE',  ( 6.357667975083864498, -3.797112024431965160, -7.724391461487830846 ) ) ;
#9633 = DIRECTION ( 'NONE',  ( 0.4809547266710045843, 0.000000000000000000, -0.8767454310646957127 ) ) ;
#9634 = CARTESIAN_POINT ( 'NONE',  ( 7.249760686538667009, 6.226446564518003157, -6.147671362329155009 ) ) ;
#9635 = AXIS2_PLACEMENT_3D ( 'NONE', #7957, #601, #2623 ) ;
#9636 = CIRCLE ( 'NONE', #24597, 5.000000000000000888 ) ;
#9637 = CARTESIAN_POINT ( 'NONE',  ( -8.000050799999998574, 3.039769662057022703, 1.609430221797942595 ) ) ;
#9638 = CARTESIAN_POINT ( 'NONE',  ( 3.249999999999999556, 4.729683950898978750, -7.360373001730866171 ) ) ;
#9639 = CARTESIAN_POINT ( 'NONE',  ( -56.63828291323059716, 0.1160565766146929301, -1.359003754613687720 ) ) ;
#9640 = CARTESIAN_POINT ( 'NONE',  ( 0.000000000000000000, -3.573533178329543425, -5.126388750707261188 ) ) ;
#9641 = ORIENTED_EDGE ( 'NONE', *, *, #12471, .T. ) ;
#9642 = DIRECTION ( 'NONE',  ( -1.000000000000000000, 0.000000000000000000, 0.000000000000000000 ) ) ;
#9643 = EDGE_LOOP ( 'NONE', ( #28786, #7364, #11097, #5023 ) ) ;
#9644 = EDGE_CURVE ( 'NONE', #27615, #29098, #18848, .T. ) ;
#9645 = CARTESIAN_POINT ( 'NONE',  ( -6.004531657079157370, 2.325406398514293205, -1.883076972206379374 ) ) ;
#9646 = CARTESIAN_POINT ( 'NONE',  ( -23.54713438637982748, 3.520075575296777171, 1.500000000000000000 ) ) ;
#9647 = EDGE_CURVE ( 'NONE', #9418, #10650, #7667, .T. ) ;
#9648 = AXIS2_PLACEMENT_3D ( 'NONE', #7848, #32942, #15014 ) ;
#9649 = CARTESIAN_POINT ( 'NONE',  ( 4.749760686538667009, -2.741043480754877582, -7.530955069117540646 ) ) ;
#9650 = DIRECTION ( 'NONE',  ( -1.000000000000000000, -0.000000000000000000, -0.000000000000000000 ) ) ;
#9651 = DIRECTION ( 'NONE',  ( -0.1027947991993878041, 0.9947025833170221043, 0.000000000000000000 ) ) ;
#9652 = ORIENTED_EDGE ( 'NONE', *, *, #587, .F. ) ;
#9653 = CARTESIAN_POINT ( 'NONE',  ( 21.36097421961354925, -21.76718868951427055, 1.410897148389129052 ) ) ;
#9654 = AXIS2_PLACEMENT_3D ( 'NONE', #25483, #14932, #24978 ) ;
#9655 = AXIS2_PLACEMENT_3D ( 'NONE', #30779, #25562, #33094 ) ;
#9656 = VECTOR ( 'NONE', #30412, 1000.000000000000114 ) ;
#9657 = ORIENTED_EDGE ( 'NONE', *, *, #11160, .F. ) ;
#9658 = APPROVAL_STATUS ( 'not_yet_approved' ) ;
#9659 = CARTESIAN_POINT ( 'NONE',  ( 85.03540396179919014, -5.198055548956801886, 4.003573871842650789 ) ) ;
#9660 = AXIS2_PLACEMENT_3D ( 'NONE', #5544, #15725, #18900 ) ;
#9661 = CARTESIAN_POINT ( 'NONE',  ( 7.249760686538667009, 4.973063321323977881, -7.199384779417068891 ) ) ;
#9664 = CARTESIAN_POINT ( 'NONE',  ( 3.122314033877864698E-16, 3.641590349731929965, 3.055657119358814011 ) ) ;
#9663 = B_SPLINE_CURVE_WITH_KNOTS ( 'NONE', 3,
 ( #23401, #27755, #20423, #25935, #15376, #10384, #20593, #8024, #30802, #20901, #12556, #18223, #23256, #17912, #30640, #18062, #25763, #3043, #7367, #7719, #28251, #4863, #15047, #28103, #13198, #25583, #5361, #15546, #28436, #2892, #25267, #22759, #5548, #359, #13057, #32967, #10036, #22910, #20247, #7527, #17733, #16, #27942, #5050, #15227, #2538 ),
 .UNSPECIFIED., .F., .F.,
 ( 4, 2, 2, 2, 2, 2, 2, 2, 2, 2, 2, 2, 2, 2, 2, 2, 2, 2, 2, 2, 2, 2, 4 ),
 ( 0.02194255756287339515, 0.02262812102983364701, 0.02331368449679389887, 0.02399924796375415073, 0.02468481143071440259, 0.02605593836463490631, 0.02674150183159515470, 0.02742706529855539963, 0.02879819223247589641, 0.03016931916639639319, 0.03085488263335664505, 0.03154044610031689344, 0.03291157303423739022, 0.03428269996815789394, 0.03565382690207839073, 0.03702495383599889445, 0.03839608076991939123, 0.03908164423687963962, 0.03976720770383988801, 0.04113833463776038479, 0.04182389810472063318, 0.04250946157168088158, 0.04388058850560139224 ),
 .UNSPECIFIED. ) ;
#9662 = DIRECTION ( 'NONE',  ( 0.000000000000000000, -0.5735764363510352792, -0.8191520442889993481 ) ) ;
#9665 = EDGE_LOOP ( 'NONE', ( #15201, #5538, #7077, #3115 ) ) ;
#9666 = PLANE ( 'NONE',  #156 ) ;
#9667 = CARTESIAN_POINT ( 'NONE',  ( 3.499999999999999556, 0.005878491403456947983, 7.047692205288324629 ) ) ;
#9668 = CARTESIAN_POINT ( 'NONE',  ( 24.92250000136559507, 0.3178988483021036315, 3.024605502323848949 ) ) ;
#9669 = B_SPLINE_CURVE_WITH_KNOTS ( 'NONE', 3,
 ( #413, #31188, #17799, #13254, #26140, #10935 ),
 .UNSPECIFIED., .F., .F.,
 ( 4, 2, 4 ),
 ( 0.000000000000000000, 0.001111101124806939712, 0.002222202249613879424 ),
 .UNSPECIFIED. ) ;
#9670 = CARTESIAN_POINT ( 'NONE',  ( 3.091618246663842218, -11.74990798379343104, -1.759199118974999587 ) ) ;
#9672 = ORIENTED_EDGE ( 'NONE', *, *, #15312, .F. ) ;
#9671 = CARTESIAN_POINT ( 'NONE',  ( 41.06247019076344884, -19.55897407381494091, 1.500000000000000444 ) ) ;
#9673 = CARTESIAN_POINT ( 'NONE',  ( -4.287550801365592967, -2.228590825266444586, -2.752080473201636401 ) ) ;
#9674 = DIRECTION ( 'NONE',  ( -1.000000000000000000, 8.574039729943018344E-17, 0.000000000000000000 ) ) ;
#9675 = CIRCLE ( 'NONE', #28373, 297.9387600756452343 ) ;
#9676 = CARTESIAN_POINT ( 'NONE',  ( 110.0070906499164352, 18.03948353657134263, 4.621439243524390506 ) ) ;
#9677 = CARTESIAN_POINT ( 'NONE',  ( 21.75111450864415730, -1.283275288181523244E-15, -2.499999999999998668 ) ) ;
#9678 = EDGE_LOOP ( 'NONE', ( #32933, #27486, #4064, #795 ) ) ;
#9680 = ORIENTED_EDGE ( 'NONE', *, *, #32026, .F. ) ;
#9679 = CARTESIAN_POINT ( 'NONE',  ( 3.499999999999999556, -5.233522515400055752, -4.720195129223329289 ) ) ;
#9681 = CIRCLE ( 'NONE', #14459, 5.010000000000000675 ) ;
#9682 = VECTOR ( 'NONE', #27624, 1000.000000000000114 ) ;
#9684 = VECTOR ( 'NONE', #6079, 1000.000000000000000 ) ;
#9683 = FACE_OUTER_BOUND ( 'NONE', #7276, .T. ) ;
#9685 = DIRECTION ( 'NONE',  ( -0.000000000000000000, -1.000000000000000000, -0.000000000000000000 ) ) ;
#9686 = APPLICATION_CONTEXT ( 'configuration controlled 3d designs of mechanical parts and assemblies' ) ;
#9687 = CIRCLE ( 'NONE', #25802, 8.749000000000002331 ) ;
#9688 = ADVANCED_FACE ( 'NONE', ( #957 ), #18514, .F. ) ;
#9689 = CARTESIAN_POINT ( 'NONE',  ( -20.12358435285846170, 17.65690804191476460, 1.499999999999999778 ) ) ;
#9690 = EDGE_CURVE ( 'NONE', #7539, #2628, #9225, .T. ) ;
#9691 = VECTOR ( 'NONE', #250, 1000.000000000000000 ) ;
#9692 = CARTESIAN_POINT ( 'NONE',  ( -2.037945749704288773E-16, -2.376879293651036118, -4.116875700062107235 ) ) ;
#9693 = CARTESIAN_POINT ( 'NONE',  ( -0.3252456059815400646, -14.55958727885318993, -1.745204947688217434 ) ) ;
#9694 = VECTOR ( 'NONE', #27679, 1000.000000000000000 ) ;
#9695 = B_SPLINE_CURVE_WITH_KNOTS ( 'NONE', 3,
 ( #19555, #24730, #31933, #29409, #6504, #25398, #25552, #22880 ),
 .UNSPECIFIED., .F., .F.,
 ( 4, 2, 2, 4 ),
 ( 2.024520226827691372E-07, 0.001227962984610853547, 0.001841843250904936927, 0.002455723517199020090 ),
 .UNSPECIFIED. ) ;
#9696 = LINE ( 'NONE', #27592, #24173 ) ;
#9697 = CARTESIAN_POINT ( 'NONE',  ( 68.92885037296282746, -3.291915072450619650, 0.8105619191588775418 ) ) ;
#9698 = CARTESIAN_POINT ( 'NONE',  ( -45.71000000000000085, -10.96999999999998643, 5.700000000000000178 ) ) ;
#9699 = ORIENTED_EDGE ( 'NONE', *, *, #18466, .F. ) ;
#9700 = CARTESIAN_POINT ( 'NONE',  ( 2.382865613620175349, 0.000000000000000000, 1.508259000770581615 ) ) ;
#9701 = VERTEX_POINT ( 'NONE', #5492 ) ;
#9702 = CARTESIAN_POINT ( 'NONE',  ( 3.499999999999999556, 4.561279057474472154, -4.271385531633124621 ) ) ;
#9703 = DIRECTION ( 'NONE',  ( 5.605325231750056938E-16, 0.3746065934159164557, -0.9271838545667855369 ) ) ;
#9704 = CARTESIAN_POINT ( 'NONE',  ( -15.12340757463330654, -21.93932300455815465, -1.000000000000000222 ) ) ;
#9705 = VERTEX_POINT ( 'NONE', #21337 ) ;
#9706 = AXIS2_PLACEMENT_3D ( 'NONE', #32700, #6429, #14437 ) ;
#9707 = VECTOR ( 'NONE', #31236, 1000.000000000000000 ) ;
#9708 = DIRECTION ( 'NONE',  ( -3.623545766764241739E-17, -0.4226182617407029385, 0.9063077870366482713 ) ) ;
#9709 = ORIENTED_EDGE ( 'NONE', *, *, #14889, .T. ) ;
#9710 = CARTESIAN_POINT ( 'NONE',  ( 3.063284526845909017, -8.734705317652711187, 0.4999240074859884198 ) ) ;
#9712 = VERTEX_POINT ( 'NONE', #10990 ) ;
#9711 = CARTESIAN_POINT ( 'NONE',  ( 18.85907022888673978, -4.752534732131552531, -4.018750267668782961 ) ) ;
#9713 = ORIENTED_EDGE ( 'NONE', *, *, #2918, .T. ) ;
#9714 = TOROIDAL_SURFACE ( 'NONE', #4908, 298.6457063863958865, 4.000000000000000888 ) ;
#9715 = DIRECTION ( 'NONE',  ( 1.000000000000000000, 0.000000000000000000, 0.000000000000000000 ) ) ;
#9716 = CIRCLE ( 'NONE', #12912, 11.00000000000000000 ) ;
#9717 = CARTESIAN_POINT ( 'NONE',  ( 23.95058674323524528, -2.449331254389988999, 1.010822989962091301 ) ) ;
#9719 = ORIENTED_EDGE ( 'NONE', *, *, #25925, .T. ) ;
#9718 = FACE_OUTER_BOUND ( 'NONE', #26003, .T. ) ;
#9720 = CARTESIAN_POINT ( 'NONE',  ( 6.524595551582240027, 4.857153507487949717, 7.168326838404958323 ) ) ;
#9721 = CARTESIAN_POINT ( 'NONE',  ( 9.192617927958343316, 0.08611596088385929659, -1.322472180770059014 ) ) ;
#9722 = DIRECTION ( 'NONE',  ( 0.000000000000000000, 0.000000000000000000, 1.000000000000000000 ) ) ;
#9723 = CARTESIAN_POINT ( 'NONE',  ( 2.589202987961084279, 10.07394153291405914, -2.218054364314494986 ) ) ;
#9725 = ORIENTED_EDGE ( 'NONE', *, *, #18364, .T. ) ;
#9724 = CARTESIAN_POINT ( 'NONE',  ( 107.4538619861916402, -17.41535791789517518, -4.649137322120033389 ) ) ;
#9726 = CARTESIAN_POINT ( 'NONE',  ( -56.32770133515838040, 0.5000000000000000000, -1.050000000000000044 ) ) ;
#9727 = ADVANCED_FACE ( 'NONE', ( #23513 ), #29049, .T. ) ;
#9728 = CIRCLE ( 'NONE', #20961, 1.676012832569465205 ) ;
#9729 = CARTESIAN_POINT ( 'NONE',  ( 5.489321606599602887, -2.678948506461278800, -7.664118171219022280 ) ) ;
#9730 = CARTESIAN_POINT ( 'NONE',  ( 23.61000000136559507, 3.156283516753366047, 0.9349337715887203748 ) ) ;
#9731 = TOROIDAL_SURFACE ( 'NONE', #29502, 5.500000000000000000, 0.5000000000000000000 ) ;
#9732 = AXIS2_PLACEMENT_3D ( 'NONE', #19275, #9239, #26628 ) ;
#9733 = CARTESIAN_POINT ( 'NONE',  ( 10.00000000000000000, 1.625881193364757449, -4.467071865485455540 ) ) ;
#9734 = CIRCLE ( 'NONE', #26320, 11.00000000000000000 ) ;
#9735 = CARTESIAN_POINT ( 'NONE',  ( -2.506063600758156262, 0.4999999999999998890, 1.500000000000000000 ) ) ;
#9736 = DIRECTION ( 'NONE',  ( -1.000000000000000000, 0.000000000000000000, 0.000000000000000000 ) ) ;
#9737 = ORIENTED_EDGE ( 'NONE', *, *, #7124, .T. ) ;
#9738 = CARTESIAN_POINT ( 'NONE',  ( 45.78962651942645579, 26.61627915917710041, 1.508259000770581837 ) ) ;
#9739 = CIRCLE ( 'NONE', #12847, 8.025310301077736241 ) ;
#9740 = ADVANCED_FACE ( 'NONE', ( #8317 ), #26201, .T. ) ;
#9741 = CIRCLE ( 'NONE', #12941, 0.9999999999999991118 ) ;
#9742 = CARTESIAN_POINT ( 'NONE',  ( -3.608283490412316094E-16, -4.208382051008173086, -2.718385644597219208 ) ) ;
#9743 = CARTESIAN_POINT ( 'NONE',  ( -6.687550801365594211, -2.228590825266444586, -2.752080473201636401 ) ) ;
#9744 = ORIENTED_EDGE ( 'NONE', *, *, #12334, .F. ) ;
#9745 = CIRCLE ( 'NONE', #10825, 11.00000000000000000 ) ;
#9746 = CARTESIAN_POINT ( 'NONE',  ( -4.104821569164996770E-16, -4.787500056513356306, -1.476463073999686015 ) ) ;
#9747 = ADVANCED_FACE ( 'NONE', ( #813 ), #21191, .F. ) ;
#9748 = CARTESIAN_POINT ( 'NONE',  ( 2.949938889207336601, 0.4708014538555321260, -1.389575531037015477 ) ) ;
#9749 = ORIENTED_EDGE ( 'NONE', *, *, #28864, .T. ) ;
#9750 = LINE ( 'NONE', #1565, #21439 ) ;
#9751 = VERTEX_POINT ( 'NONE', #28860 ) ;
#9752 = VERTEX_POINT ( 'NONE', #13644 ) ;
#9753 = CARTESIAN_POINT ( 'NONE',  ( 107.4500593345376558, -17.36019228850485163, -4.522129901861164925 ) ) ;
#9754 = VECTOR ( 'NONE', #20773, 1000.000000000000000 ) ;
#9756 = ORIENTED_EDGE ( 'NONE', *, *, #17737, .T. ) ;
#9755 = CARTESIAN_POINT ( 'NONE',  ( 0.000000000000000000, -28.43932300454937590, -1.500000000000000000 ) ) ;
#9757 = EDGE_CURVE ( 'NONE', #22601, #7258, #28485, .T. ) ;
#9758 = VERTEX_POINT ( 'NONE', #31543 ) ;
#9759 = CARTESIAN_POINT ( 'NONE',  ( 24.04750000136559507, -3.024605502323851169, 0.3178988483021052969 ) ) ;
#9760 = AXIS2_PLACEMENT_3D ( 'NONE', #21551, #16351, #26419 ) ;
#9761 = AXIS2_PLACEMENT_3D ( 'NONE', #21900, #14355, #16543 ) ;
#9762 = AXIS2_PLACEMENT_3D ( 'NONE', #3174, #5683, #13336 ) ;
#9763 = VERTEX_POINT ( 'NONE', #15834 ) ;
#9764 = CARTESIAN_POINT ( 'NONE',  ( 0.3045634402742549707, 9.425384029459882740, -4.096074720329697882 ) ) ;
#9766 = ORIENTED_EDGE ( 'NONE', *, *, #21455, .T. ) ;
#9765 = FACE_OUTER_BOUND ( 'NONE', #6864, .T. ) ;
#9767 = CARTESIAN_POINT ( 'NONE',  ( -56.73266014122250311, 0.2590449313022686884, -1.045342064611400446 ) ) ;
#9768 = EDGE_CURVE ( 'NONE', #12332, #4399, #30097, .T. ) ;
#9769 = AXIS2_PLACEMENT_3D ( 'NONE', #1977, #1629, #11819 ) ;
#9770 = DIRECTION ( 'NONE',  ( 0.000000000000000000, 0.000000000000000000, 1.000000000000000000 ) ) ;
#9771 = CARTESIAN_POINT ( 'NONE',  ( 25.54750000136559507, 3.024605502323846729, -0.3178988483021056854 ) ) ;
#9772 = CYLINDRICAL_SURFACE ( 'NONE', #6583, 2.999999999999999112 ) ;
#9773 = CARTESIAN_POINT ( 'NONE',  ( 107.9424804437600756, 20.70775667334615378, 1.742830623350447361 ) ) ;
#9774 = CARTESIAN_POINT ( 'NONE',  ( -50.60000000000000142, -10.96966150227468972, -0.2618072999578781590 ) ) ;
#9775 = CARTESIAN_POINT ( 'NONE',  ( 24.35085591271619876, -17.33674746172420811, 1.318654801572268553 ) ) ;
#9776 = EDGE_CURVE ( 'NONE', #12927, #18318, #13789, .T. ) ;
#9777 = ADVANCED_FACE ( 'NONE', ( #26044 ), #16323, .T. ) ;
#9778 = CYLINDRICAL_SURFACE ( 'NONE', #77, 5.000000000000000888 ) ;
#9779 = CARTESIAN_POINT ( 'NONE',  ( 54.77277180716814087, -8.244003004416214253, 0.02339150517593243869 ) ) ;
#9780 = VECTOR ( 'NONE', #28840, 1000.000000000000114 ) ;
#9781 = CARTESIAN_POINT ( 'NONE',  ( 5.377543748152548986, 7.892520144992435149, 1.391664247347255134 ) ) ;
#9782 = DIRECTION ( 'NONE',  ( 0.000000000000000000, 0.000000000000000000, 1.000000000000000000 ) ) ;
#9783 = VECTOR ( 'NONE', #16592, 1000.000000000000000 ) ;
#9784 = CARTESIAN_POINT ( 'NONE',  ( -30.08790297335274389, 4.402097243136376292, 5.181439978443226124 ) ) ;
#9785 = CARTESIAN_POINT ( 'NONE',  ( -2.000050802731187627, 3.113457007523260156, -0.9222479816126439855 ) ) ;
#9786 = EDGE_LOOP ( 'NONE', ( #10077, #6971, #7426, #29283 ) ) ;
#9787 = TOROIDAL_SURFACE ( 'NONE', #21022, 5.500000000000001776, 0.5000000000000000000 ) ;
#9788 = AXIS2_PLACEMENT_3D ( 'NONE', #19722, #14530, #7005 ) ;
#9789 = CARTESIAN_POINT ( 'NONE',  ( -2.800050800000000173, 2.331437884370912705, -1.887961173149511618 ) ) ;
#9790 = CIRCLE ( 'NONE', #15675, 5.009999999999999787 ) ;
#9791 = CARTESIAN_POINT ( 'NONE',  ( 0.08034253207385409767, 4.547003328335266659, 9.783802610460128335 ) ) ;
#9792 = DIRECTION ( 'NONE',  ( -0.4809547266710039182, 0.000000000000000000, 0.8767454310646960458 ) ) ;
#9793 = APPROVAL_PERSON_ORGANIZATION ( #6179, #19048, #16512 ) ;
#9794 = ORIENTED_EDGE ( 'NONE', *, *, #16956, .F. ) ;
#9795 = CARTESIAN_POINT ( 'NONE',  ( 3.499999999999999556, -6.700937042937072263, 2.183447440113167826 ) ) ;
#9796 = ADVANCED_FACE ( 'NONE', ( #15087 ), #24339, .T. ) ;
#9797 = EDGE_LOOP ( 'NONE', ( #19528, #11633, #21261, #17938 ) ) ;
#9798 = CARTESIAN_POINT ( 'NONE',  ( 21.04767255915003332, -17.06392231637734724, 1.500000000000000666 ) ) ;
#9799 = APPROVAL_STATUS ( 'not_yet_approved' ) ;
#9800 = DIRECTION ( 'NONE',  ( -1.000000000000000000, -0.000000000000000000, -0.000000000000000000 ) ) ;
#9801 = ORIENTED_EDGE ( 'NONE', *, *, #10496, .T. ) ;
#9802 = CARTESIAN_POINT ( 'NONE',  ( 5.994372355876373959, -18.63462559044425149, 1.499999999999998668 ) ) ;
#9803 = ORIENTED_EDGE ( 'NONE', *, *, #31759, .T. ) ;
#9804 = LINE ( 'NONE', #25001, #1621 ) ;
#9805 = VECTOR ( 'NONE', #9584, 1000.000000000000000 ) ;
#9806 = CARTESIAN_POINT ( 'NONE',  ( 69.05921145840204645, -5.891398902038758045, -4.215290682824791801 ) ) ;
#9807 = AXIS2_PLACEMENT_3D ( 'NONE', #18187, #827, #28573 ) ;
#9808 = CARTESIAN_POINT ( 'NONE',  ( -56.76324651597856530, 0.6586745643427850405, 1.499999999999941158 ) ) ;
#9809 = CARTESIAN_POINT ( 'NONE',  ( 107.9802527803230419, -17.78500706576073753, 4.325704939602341703 ) ) ;
#9810 =( BOUNDED_SURFACE ( )  B_SPLINE_SURFACE ( 1, 2, ( 
 ( #22280, #9551, #12403, #30470, #27287, #32986, #17756, #19766, #25100, #32833, #4404, #27625, #4218, #32651, #24599, #10055, #2217, #7063, #27777, #25291, #7385, #14390, #2404, #24944, #14588, #11927, #32490, #22127, #22624, #2058, #20118, #12229, #22436, #30311, #4889, #9730, #19960, #30164, #9400, #15071, #29809, #7237, #6883, #17426, #4726, #14896, #17074, #27966, #25605, #2718, #233, #26106, #28124, #15753, #18249, #20767, #3066, #15397, #5572, #30967, #380, #28462, #17933, #12891, #3211, #18083, #28623, #10555, #28273, #31307, #5223, #23111, #13078, #10405, #5070, #20615, #30822, #7890, #13373, #5384, #25957 ),
 ( #15574, #13221, #8049, #23421, #528, #25789, #2915, #23589, #23279, #5718, #10716, #710, #12726, #20929, #31149, #10900, #8236, #18432, #10225, #8381, #15898, #21107, #15247, #25451, #2559, #22928, #39, #20447, #30667, #7741, #24250, #14203, #13710, #23762, #14041, #8867, #11543, #28938, #16238, #21741, #1190, #31621, #876, #28768, #5858, #24067, #31949, #18578, #16383, #16044, #13856, #16728, #11388, #21587, #9014, #26932, #19231, #8528, #3550, #26276, #31451, #31793, #19074, #1020, #29115, #29430, #3390, #13555, #23911, #29262, #11053, #11204, #21412, #26749, #11696, #18734, #24400, #21894, #8709, #6348, #1368 ) ),
 .UNSPECIFIED., .F., .F., .F. ) 
 B_SPLINE_SURFACE_WITH_KNOTS ( ( 2, 2 ),
 ( 3, 2, 2, 2, 2, 2, 2, 2, 2, 2, 2, 2, 2, 2, 2, 2, 2, 2, 2, 2, 2, 2, 2, 2, 2, 2, 2, 2, 2, 2, 2, 2, 2, 2, 2, 2, 2, 2, 2, 2, 3 ),
 ( 0.000000000000000000, 1.000000000000000000 ),
 ( 0.000000000000000000, 0.02500000000000000139, 0.05000000000000000278, 0.07499999999999999722, 0.1000000000000000056, 0.1250000000000000000, 0.1499999999999999944, 0.1749999999999999889, 0.2000000000000000111, 0.2250000000000000056, 0.2500000000000000000, 0.2750000000000000222, 0.2999999999999999889, 0.3250000000000000111, 0.3499999999999999778, 0.3750000000000000000, 0.4000000000000000222, 0.4249999999999999889, 0.4500000000000000111, 0.4749999999999999778, 0.5000000000000000000, 0.5250000000000000222, 0.5500000000000000444, 0.5749999999999999556, 0.5999999999999999778, 0.6250000000000000000, 0.6500000000000000222, 0.6750000000000000444, 0.6999999999999999556, 0.7249999999999999778, 0.7500000000000000000, 0.7750000000000000222, 0.8000000000000000444, 0.8249999999999999556, 0.8499999999999999778, 0.8750000000000000000, 0.9000000000000000222, 0.9250000000000000444, 0.9499999999999999556, 0.9749999999999999778, 1.000000000000000000 ),
 .UNSPECIFIED. ) 
 GEOMETRIC_REPRESENTATION_ITEM ( )  RATIONAL_B_SPLINE_SURFACE ( (
 ( 1.000000000000000000, 0.9238795325112867385, 1.000000000000000000, 0.9238795325112867385, 1.000000000000000000, 0.9238795325112867385, 1.000000000000000000, 0.9238795325112867385, 1.000000000000000000, 0.9238795325112867385, 1.000000000000000000, 0.9238795325112867385, 1.000000000000000000, 0.9238795325112867385, 1.000000000000000000, 0.9238795325112867385, 1.000000000000000000, 0.9238795325112867385, 1.000000000000000000, 0.9238795325112867385, 1.000000000000000000, 0.9238795325112867385, 1.000000000000000000, 0.9238795325112867385, 1.000000000000000000, 0.9238795325112867385, 1.000000000000000000, 0.9238795325112867385, 1.000000000000000000, 0.9238795325112867385, 1.000000000000000000, 0.9238795325112867385, 1.000000000000000000, 0.9238795325112867385, 1.000000000000000000, 0.9238795325112867385, 1.000000000000000000, 0.9238795325112867385, 1.000000000000000000, 0.9238795325112867385, 1.000000000000000000, 0.9238795325112867385, 1.000000000000000000, 0.9238795325112867385, 1.000000000000000000, 0.9238795325112867385, 1.000000000000000000, 0.9238795325112867385, 1.000000000000000000, 0.9238795325112867385, 1.000000000000000000, 0.9238795325112867385, 1.000000000000000000, 0.9238795325112867385, 1.000000000000000000, 0.9238795325112867385, 1.000000000000000000, 0.9238795325112867385, 1.000000000000000000, 0.9238795325112867385, 1.000000000000000000, 0.9238795325112867385, 1.000000000000000000, 0.9238795325112867385, 1.000000000000000000, 0.9238795325112867385, 1.000000000000000000, 0.9238795325112867385, 1.000000000000000000, 0.9238795325112867385, 1.000000000000000000, 0.9238795325112867385, 1.000000000000000000, 0.9238795325112867385, 1.000000000000000000, 0.9238795325112867385, 1.000000000000000000, 0.9238795325112867385, 1.000000000000000000, 0.9238795325112867385, 1.000000000000000000),
 ( 1.000000000000000000, 0.9238795325112867385, 1.000000000000000000, 0.9238795325112867385, 1.000000000000000000, 0.9238795325112867385, 1.000000000000000000, 0.9238795325112867385, 1.000000000000000000, 0.9238795325112867385, 1.000000000000000000, 0.9238795325112867385, 1.000000000000000000, 0.9238795325112867385, 1.000000000000000000, 0.9238795325112867385, 1.000000000000000000, 0.9238795325112867385, 1.000000000000000000, 0.9238795325112867385, 1.000000000000000000, 0.9238795325112867385, 1.000000000000000000, 0.9238795325112867385, 1.000000000000000000, 0.9238795325112867385, 1.000000000000000000, 0.9238795325112867385, 1.000000000000000000, 0.9238795325112867385, 1.000000000000000000, 0.9238795325112867385, 1.000000000000000000, 0.9238795325112867385, 1.000000000000000000, 0.9238795325112867385, 1.000000000000000000, 0.9238795325112867385, 1.000000000000000000, 0.9238795325112867385, 1.000000000000000000, 0.9238795325112867385, 1.000000000000000000, 0.9238795325112867385, 1.000000000000000000, 0.9238795325112867385, 1.000000000000000000, 0.9238795325112867385, 1.000000000000000000, 0.9238795325112867385, 1.000000000000000000, 0.9238795325112867385, 1.000000000000000000, 0.9238795325112867385, 1.000000000000000000, 0.9238795325112867385, 1.000000000000000000, 0.9238795325112867385, 1.000000000000000000, 0.9238795325112867385, 1.000000000000000000, 0.9238795325112867385, 1.000000000000000000, 0.9238795325112867385, 1.000000000000000000, 0.9238795325112867385, 1.000000000000000000, 0.9238795325112867385, 1.000000000000000000, 0.9238795325112867385, 1.000000000000000000, 0.9238795325112867385, 1.000000000000000000, 0.9238795325112867385, 1.000000000000000000, 0.9238795325112867385, 1.000000000000000000, 0.9238795325112867385, 1.000000000000000000, 0.9238795325112867385, 1.000000000000000000) ) ) 
 REPRESENTATION_ITEM ( '' )  SURFACE ( )  );
#9811 = CARTESIAN_POINT ( 'NONE',  ( 107.5617944031221640, -18.98359742639815551, -4.522129901861166701 ) ) ;
#9812 = VECTOR ( 'NONE', #32880, 999.9999999999998863 ) ;
#9813 = ADVANCED_FACE ( 'NONE', ( #29538 ), #22637, .T. ) ;
#9814 = CARTESIAN_POINT ( 'NONE',  ( 21.44478664388827127, -21.75412686751143099, -1.457848360901668139 ) ) ;
#9815 = VECTOR ( 'NONE', #10607, 1000.000000000000000 ) ;
#9816 = DIRECTION ( 'NONE',  ( 0.000000000000000000, 0.7431448254773954654, -0.6691306063588569053 ) ) ;
#9818 = VERTEX_POINT ( 'NONE', #24482 ) ;
#9817 = CARTESIAN_POINT ( 'NONE',  ( -3.200050802731187360, -3.113457007523259268, 0.9222479816126455399 ) ) ;
#9819 = CARTESIAN_POINT ( 'NONE',  ( 21.42250000273118715, 1.291182301015469047, 2.378061970571981654 ) ) ;
#9820 = DIRECTION ( 'NONE',  ( -0.1908089953765452762, 0.000000000000000000, 0.9816271834476639757 ) ) ;
#9821 = CARTESIAN_POINT ( 'NONE',  ( 79.92595492699416582, 21.43178168691304819, -1.491740999229419273 ) ) ;
#9822 = DIRECTION ( 'NONE',  ( 0.000000000000000000, 0.000000000000000000, -1.000000000000000000 ) ) ;
#9823 = EDGE_CURVE ( 'NONE', #8686, #21913, #18339, .T. ) ;
#9824 = LOCAL_TIME ( 16, 7, 10.00000000000000000, #11847 ) ;
#9825 = EDGE_CURVE ( 'NONE', #30917, #6888, #3443, .T. ) ;
#9826 = CARTESIAN_POINT ( 'NONE',  ( -32.37020706055090358, 18.00000000000000355, 3.000000000000004441 ) ) ;
#9827 = FACE_OUTER_BOUND ( 'NONE', #13202, .T. ) ;
#9828 = CARTESIAN_POINT ( 'NONE',  ( -56.31962101169892065, 0.2221239435922897909, -1.416967151343360376 ) ) ;
#9829 = CARTESIAN_POINT ( 'NONE',  ( 23.24441267594672311, -21.93876234581717810, 1.082412871822684419 ) ) ;
#9830 = ORIENTED_EDGE ( 'NONE', *, *, #31243, .T. ) ;
#9831 = CARTESIAN_POINT ( 'NONE',  ( -5.312550801365592434, 1.088641768524161613, 3.675193018007247403 ) ) ;
#9832 = ORIENTED_EDGE ( 'NONE', *, *, #6571, .T. ) ;
#9833 = CARTESIAN_POINT ( 'NONE',  ( -7.054531657079158080, -2.846291840500172921, -1.545410377633947618 ) ) ;
#9834 = B_SPLINE_CURVE_WITH_KNOTS ( 'NONE', 3,
 ( #772, #3930, #31843, #16285, #13756, #18972, #21299, #14104, #24131, #24304, #9065, #29158, #10954, #1417, #21787, #6246, #31995, #19292, #15945, #13431, #3268, #23652, #31354, #18626, #28820, #16110, #26342, #18798, #3449, #13605, #23811, #31502, #8587, #7250, #6746, #2239, #27484, #30177 ),
 .UNSPECIFIED., .F., .F.,
 ( 4, 2, 2, 2, 2, 2, 2, 2, 2, 2, 2, 2, 2, 2, 2, 2, 2, 2, 4 ),
 ( 2.954127631045189498E-16, 0.003856977557342960126, 0.007713955114685625350, 0.01157093267202828971, 0.01349942145069962102, 0.01542791022937095233, 0.01735639900804228711, 0.01832064339737795103, 0.01928488778671362189, 0.02121337656538495320, 0.02217762095472062753, 0.02314186534405629492, 0.02362398753872413382, 0.02410610973339196578, 0.02507035412272764011, 0.02603459851206331443, 0.02699884290139898529, 0.02892733168007033048, 0.03085582045874168261 ),
 .UNSPECIFIED. ) ;
#9835 = CARTESIAN_POINT ( 'NONE',  ( -29.41021809322157310, 5.485000000000014531, 1.500000000000000000 ) ) ;
#9836 = CARTESIAN_POINT ( 'NONE',  ( 85.38119660045754244, -6.034158634414237277, -4.522129901861164036 ) ) ;
#9837 = CARTESIAN_POINT ( 'NONE',  ( 0.1347475173545765736, -7.019624077805855400, 1.774480656747167373 ) ) ;
#9838 = LINE ( 'NONE', #17864, #7650 ) ;
#9839 = VERTEX_POINT ( 'NONE', #22789 ) ;
#9840 = DIRECTION ( 'NONE',  ( 0.000000000000000000, 0.000000000000000000, 1.000000000000000000 ) ) ;
#9841 = EDGE_CURVE ( 'NONE', #22601, #5630, #10835, .T. ) ;
#9842 = APPROVAL ( #25391, 'UNSPECIFIED' ) ;
#9843 = VERTEX_POINT ( 'NONE', #26674 ) ;
#9844 = CARTESIAN_POINT ( 'NONE',  ( 6.037141879243262288, -5.096219216992895262, 6.770886333893406217 ) ) ;
#9845 = COORDINATED_UNIVERSAL_TIME_OFFSET ( 0, 0, .AHEAD. ) ;
#9846 = EDGE_CURVE ( 'NONE', #32461, #12125, #7432, .T. ) ;
#9847 = CARTESIAN_POINT ( 'NONE',  ( 102.4219044191236918, -3.979760264920891188, 4.023790184227316047 ) ) ;
#9848 = B_SPLINE_CURVE_WITH_KNOTS ( 'NONE', 3,
 ( #20038, #126, #23007, #33051, #22702, #10124 ),
 .UNSPECIFIED., .F., .F.,
 ( 4, 2, 4 ),
 ( -6.833360019735199612E-06, 0.0003895853402124996290, 0.0007860040404447344534 ),
 .UNSPECIFIED. ) ;
#9849 = CARTESIAN_POINT ( 'NONE',  ( 19.01016806367753631, -3.063564188380631048, -0.8125824237644804215 ) ) ;
#9851 = CARTESIAN_POINT ( 'NONE',  ( 6.037141752603385925, -0.4483113388087880957, -8.462586328878542119 ) ) ;
#9850 = CARTESIAN_POINT ( 'NONE',  ( 0.7212197917577903850, 7.537903528354217286, -4.829101774917270440 ) ) ;
#9852 = ORIENTED_EDGE ( 'NONE', *, *, #19013, .T. ) ;
#9853 = PLANE ( 'NONE',  #16725 ) ;
#9854 = CARTESIAN_POINT ( 'NONE',  ( 0.000000000000000000, 3.673940397442060361E-16, 3.000000000000000444 ) ) ;
#9855 = EDGE_CURVE ( 'NONE', #9082, #1245, #32213, .T. ) ;
#9856 = CARTESIAN_POINT ( 'NONE',  ( 24.23500000136559507, -3.156283516753370044, -0.9349337715887220401 ) ) ;
#9857 = CARTESIAN_POINT ( 'NONE',  ( 0.7551355282337928188, -8.141491703254255086, -1.499999999999999556 ) ) ;
#9859 = VERTEX_POINT ( 'NONE', #16818 ) ;
#9858 = CARTESIAN_POINT ( 'NONE',  ( 71.53201042711403090, -18.09776336788796058, 0.9788672205888330202 ) ) ;
#9860 = AXIS2_PLACEMENT_3D ( 'NONE', #6125, #13778, #4110 ) ;
#9861 = CARTESIAN_POINT ( 'NONE',  ( -4.887550801365593500, 2.752080473201636845, -2.228590825266444142 ) ) ;
#9862 = DIRECTION ( 'NONE',  ( -0.000000000000000000, -0.000000000000000000, -1.000000000000000000 ) ) ;
#9863 = DIRECTION ( 'NONE',  ( 0.1767573132311704154, 0.9842544651762052954, 0.000000000000000000 ) ) ;
#9864 = DIRECTION ( 'NONE',  ( -1.000000000000000000, -0.000000000000000000, 0.000000000000000000 ) ) ;
#9865 = ORIENTED_EDGE ( 'NONE', *, *, #14649, .F. ) ;
#9867 = ORIENTED_EDGE ( 'NONE', *, *, #9196, .F. ) ;
#9866 = CARTESIAN_POINT ( 'NONE',  ( 24.37248106196387454, -17.41561295275149135, 1.432003413861882901 ) ) ;
#9868 = CARTESIAN_POINT ( 'NONE',  ( 8.930755659325141593, 0.5000000000000008882, 1.500000000000000000 ) ) ;
#9869 = CARTESIAN_POINT ( 'NONE',  ( 7.249760686538667009, 8.466096581343482086, 2.210816291636243047 ) ) ;
#9870 = CARTESIAN_POINT ( 'NONE',  ( 20.92250000136559507, 0.3178988483021036315, 3.024605502323848949 ) ) ;
#9871 = CARTESIAN_POINT ( 'NONE',  ( 0.000000000000000000, 6.745408891279541130, 5.171987904998129437 ) ) ;
#9872 = CARTESIAN_POINT ( 'NONE',  ( -1.201691756929461397, -13.92897885394997992, -1.500000000000556222 ) ) ;
#9873 = CARTESIAN_POINT ( 'NONE',  ( 7.249760686538667009, -1.391664247347281780, 7.892520144992429820 ) ) ;
#9874 = B_SPLINE_CURVE_WITH_KNOTS ( 'NONE', 3,
 ( #9168, #19401, #32436, #29599, #1665, #14695, #22379, #14336, #17206, #17379 ),
 .UNSPECIFIED., .F., .F.,
 ( 4, 2, 2, 2, 4 ),
 ( 2.571685856657688708E-07, 0.0005478592107668807691, 0.001095461252948095677, 0.001643063295129310476, 0.002190665337310524624 ),
 .UNSPECIFIED. ) ;
#9875 = LINE ( 'NONE', #12547, #21509 ) ;
#9876 = CARTESIAN_POINT ( 'NONE',  ( 0.5640493910637699448, 7.306425354220341006, 6.134141009795914812 ) ) ;
#9877 = ORIENTED_EDGE ( 'NONE', *, *, #14637, .F. ) ;
#9878 = CARTESIAN_POINT ( 'NONE',  ( 34.48223484310469189, 0.5000000000000000000, 2.982234843104950350 ) ) ;
#9879 = EDGE_CURVE ( 'NONE', #32541, #5413, #22393, .T. ) ;
#9880 = APPLICATION_PROTOCOL_DEFINITION ( 'international standard', 'config_control_design', 1994, #15441 ) ;
#9881 = DIRECTION ( 'NONE',  ( 2.473959037481237219E-13, 1.000000000000000000, -0.000000000000000000 ) ) ;
#9882 = VERTEX_POINT ( 'NONE', #1602 ) ;
#9883 = CARTESIAN_POINT ( 'NONE',  ( 107.4928421713820086, 18.16941992634724201, -4.994310381140683930 ) ) ;
#9884 = EDGE_LOOP ( 'NONE', ( #15229, #11235, #3240, #32947 ) ) ;
#9885 = DIRECTION ( 'NONE',  ( 1.000000000000000000, 0.000000000000000000, 0.000000000000000000 ) ) ;
#9887 = VERTEX_POINT ( 'NONE', #21995 ) ;
#9886 = CARTESIAN_POINT ( 'NONE',  ( 18.85967421310764536, -4.745783400722740630, -4.008637382318521070 ) ) ;
#9888 = ORIENTED_EDGE ( 'NONE', *, *, #29350, .F. ) ;
#9889 = ADVANCED_FACE ( 'NONE', ( #4737 ), #32223, .T. ) ;
#9890 = CARTESIAN_POINT ( 'NONE',  ( -34.92557263839314885, 0.5000000000000000000, 2.487612133692613359 ) ) ;
#9891 = EDGE_CURVE ( 'NONE', #12410, #2199, #2813, .T. ) ;
#9892 = CARTESIAN_POINT ( 'NONE',  ( 10.52034268205830614, 3.672404558090085480, -3.407865132560142563 ) ) ;
#9893 = CARTESIAN_POINT ( 'NONE',  ( -31.57659242536668742, -28.43932300454937590, -0.9999999999999997780 ) ) ;
#9895 = ORIENTED_EDGE ( 'NONE', *, *, #30148, .F. ) ;
#9894 = DIRECTION ( 'NONE',  ( -8.541412920197212419E-17, -0.9961946980917449901, -0.08715574274766552110 ) ) ;
#9896 = CARTESIAN_POINT ( 'NONE',  ( 34.48223484310472031, 0.5000000000000000000, -2.552009564962230304 ) ) ;
#9897 = CARTESIAN_POINT ( 'NONE',  ( 21.26379237082032247, 16.93099014934048441, 1.500000000000000222 ) ) ;
#9898 = ADVANCED_FACE ( 'NONE', ( #6780 ), #3786, .F. ) ;
#9899 = DIRECTION ( 'NONE',  ( -1.000000000000000000, -0.000000000000000000, 0.000000000000000000 ) ) ;
#9900 = CARTESIAN_POINT ( 'NONE',  ( 2.274274201625309910, -1.464956435139646462, 10.90201369670501386 ) ) ;
#9902 = ORIENTED_EDGE ( 'NONE', *, *, #10674, .T. ) ;
#9901 = CARTESIAN_POINT ( 'NONE',  ( 108.0288784395952320, -18.48520446273847995, -4.337460765736292245 ) ) ;
#9903 = DIRECTION ( 'NONE',  ( 0.03487826274237469659, 0.9987827659587182882, 0.03487826274237468965 ) ) ;
#9904 = CARTESIAN_POINT ( 'NONE',  ( 10.52034268205830259, 3.055657119358849094, -3.641590349731898879 ) ) ;
#9905 = CARTESIAN_POINT ( 'NONE',  ( 23.27353278736380204, -21.94187821002792660, 1.000000000000000000 ) ) ;
#9906 = CARTESIAN_POINT ( 'NONE',  ( 107.6996442589674103, 19.35565155597527109, -4.612695725900422872 ) ) ;
#9907 = DIRECTION ( 'NONE',  ( 0.1437473352845043406, 0.000000000000000000, -0.9896144216807899463 ) ) ;
#9908 = CARTESIAN_POINT ( 'NONE',  ( 109.3697760341437970, 14.49066428361112813, 0.4463807625373157340 ) ) ;
#9909 = ORIENTED_EDGE ( 'NONE', *, *, #17866, .F. ) ;
#9910 = CARTESIAN_POINT ( 'NONE',  ( 6.883866601413091146, -4.949663153219582945, 7.193114723270793931 ) ) ;
#9911 = CARTESIAN_POINT ( 'NONE',  ( -2.007992423166597984, -0.3178988483021057410, 3.024605502323848949 ) ) ;
#9912 = CARTESIAN_POINT ( 'NONE',  ( -6.437550801365593323, 3.675193018007246959, -1.088641768524161391 ) ) ;
#9913 = ORIENTED_EDGE ( 'NONE', *, *, #28715, .F. ) ;
#9914 = DIRECTION ( 'NONE',  ( -1.000000000000000000, 0.000000000000000000, 0.000000000000000000 ) ) ;
#9915 = CARTESIAN_POINT ( 'NONE',  ( 10.52034268205830614, -3.641590349731950393, 3.055657119358789142 ) ) ;
#9916 = CARTESIAN_POINT ( 'NONE',  ( 2.712282326253041553, -0.4283266402566512365, -1.500000000000000666 ) ) ;
#9917 = EDGE_LOOP ( 'NONE', ( #4731, #26470, #5804 ) ) ;
#9918 = CARTESIAN_POINT ( 'NONE',  ( 108.3721138247593814, 20.25023653042131144, 2.537511488057705655 ) ) ;
#9919 = VERTEX_POINT ( 'NONE', #2232 ) ;
#9920 = ADVANCED_FACE ( 'NONE', ( #12419 ), #1300, .T. ) ;
#9921 = DIRECTION ( 'NONE',  ( 0.000000000000000000, 0.000000000000000000, 1.000000000000000000 ) ) ;
#9922 = VERTEX_POINT ( 'NONE', #28284 ) ;
#9923 = CYLINDRICAL_SURFACE ( 'NONE', #1739, 6.248999999999999666 ) ;
#9925 = EDGE_LOOP ( 'NONE', ( #1661, #12177, #21382 ) ) ;
#9924 = DIRECTION ( 'NONE',  ( 0.000000000000000000, 1.000000000000000000, -1.224646799147353207E-16 ) ) ;
#9926 = VERTEX_POINT ( 'NONE', #5395 ) ;
#9927 = DIRECTION ( 'NONE',  ( -0.000000000000000000, 0.3746065934159164001, -0.9271838545667856479 ) ) ;
#9928 = ORIENTED_EDGE ( 'NONE', *, *, #19522, .F. ) ;
#9929 = CARTESIAN_POINT ( 'NONE',  ( -3.683682291401270757E-13, 9.884132761439586190, -4.709950686175258916 ) ) ;
#9931 = ORIENTED_EDGE ( 'NONE', *, *, #30900, .F. ) ;
#9930 = CARTESIAN_POINT ( 'NONE',  ( 21.36097421961354925, -21.76718868951427055, 1.410897148389129052 ) ) ;
#9932 = CARTESIAN_POINT ( 'NONE',  ( 9.302055952193859056, 0.2457637073201327793, 1.049999999999999822 ) ) ;
#9933 = CARTESIAN_POINT ( 'NONE',  ( 21.00111451137534146, -1.283275288181523244E-15, -2.499999999999998668 ) ) ;
#9934 = CARTESIAN_POINT ( 'NONE',  ( 3.249999999999999556, 0.000000000000000000, 0.000000000000000000 ) ) ;
#9935 = CARTESIAN_POINT ( 'NONE',  ( 107.8351701702616197, 20.11025589396474444, 3.017643035989555411 ) ) ;
#9936 = DIRECTION ( 'NONE',  ( -0.000000000000000000, 0.000000000000000000, 1.000000000000000000 ) ) ;
#9937 = DIRECTION ( 'NONE',  ( 1.000000000000000000, -8.574039729943018344E-17, -0.000000000000000000 ) ) ;
#9938 = DIRECTION ( 'NONE',  ( 1.000000000000000000, -0.000000000000000000, 0.000000000000000000 ) ) ;
#9939 = CARTESIAN_POINT ( 'NONE',  ( 47.75999538435722513, -8.435302152663906483, -0.02339150517595086839 ) ) ;
#9940 = CARTESIAN_POINT ( 'NONE',  ( 25.75999999999999801, -2.208672634433321348E-15, 0.000000000000000000 ) ) ;
#9941 = CARTESIAN_POINT ( 'NONE',  ( 7.249760686538667009, -2.210816291636271025, 8.466096581343474980 ) ) ;
#9942 = CARTESIAN_POINT ( 'NONE',  ( -14.85000000000000142, -10.96966150227469328, 1.500000000000000000 ) ) ;
#9943 = EDGE_CURVE ( 'NONE', #11449, #7955, #15038, .T. ) ;
#9944 = CARTESIAN_POINT ( 'NONE',  ( -3.000050802731188071, -0.9222479816126459840, -3.113457007523259268 ) ) ;
#9945 = ORIENTED_EDGE ( 'NONE', *, *, #10674, .F. ) ;
#9946 = CARTESIAN_POINT ( 'NONE',  ( -7.787550801365593856, -0.3701630799359326152, 3.521866450007987037 ) ) ;
#9947 = EDGE_CURVE ( 'NONE', #2193, #20203, #15406, .T. ) ;
#9948 = CARTESIAN_POINT ( 'NONE',  ( -15.00280984543113583, -21.93932300455818307, 1.000000000000000000 ) ) ;
#9949 = DIRECTION ( 'NONE',  ( 0.000000000000000000, 0.3090169943749482284, -0.9510565162951533091 ) ) ;
#9950 = ORIENTED_EDGE ( 'NONE', *, *, #4615, .F. ) ;
#9951 = CARTESIAN_POINT ( 'NONE',  ( 10.56870887191539587, -4.467071865485484850, 1.625881193364682620 ) ) ;
#9952 = CYLINDRICAL_SURFACE ( 'NONE', #13483, 0.5000000000000000000 ) ;
#9953 = CARTESIAN_POINT ( 'NONE',  ( 107.9809968313877562, -17.79572121599716539, 4.354976952678953239 ) ) ;
#9954 = VERTEX_POINT ( 'NONE', #10066 ) ;
#9955 = CARTESIAN_POINT ( 'NONE',  ( 2.898548264872579328, 7.988558554883838703, 5.028941032539350431 ) ) ;
#9956 = COORDINATED_UNIVERSAL_TIME_OFFSET ( 0, 0, .AHEAD. ) ;
#9957 = CARTESIAN_POINT ( 'NONE',  ( 74.44693909927218556, -23.04272217940714995, -0.9788672205760856615 ) ) ;
#9959 = ADVANCED_FACE ( 'NONE', ( #5232 ), #8246, .F. ) ;
#9958 = VERTEX_POINT ( 'NONE', #13380 ) ;
#9960 = CARTESIAN_POINT ( 'NONE',  ( -3.262323615140995781, -10.74303876590519558, 1.743566368971870340 ) ) ;
#9961 = MANIFOLD_SOLID_BREP ( 'Shell1', #4414 ) ;
#9962 = EDGE_CURVE ( 'NONE', #7257, #9966, #538, .T. ) ;
#9963 = ORIENTED_EDGE ( 'NONE', *, *, #1222, .T. ) ;
#9964 = DIRECTION ( 'NONE',  ( 0.9947025833170223263, 0.1027947991993880261, 0.000000000000000000 ) ) ;
#9966 = VERTEX_POINT ( 'NONE', #7901 ) ;
#9965 = CARTESIAN_POINT ( 'NONE',  ( -8.000050800000000351, 3.673940397442060361E-16, 3.000000000000000444 ) ) ;
#9967 = DIRECTION ( 'NONE',  ( -0.000000000000000000, -0.000000000000000000, 1.000000000000000000 ) ) ;
#9969 = CARTESIAN_POINT ( 'NONE',  ( 10.00000000000000000, 4.681538312723528605, -0.8254815157534771686 ) ) ;
#9968 = ADVANCED_BREP_SHAPE_REPRESENTATION ( '', ( #21573, #2865 ), #8690 ) ;
#9970 = CARTESIAN_POINT ( 'NONE',  ( 107.6641765185768378, -20.45809951660586634, 1.500000000000000000 ) ) ;
#9971 = EDGE_CURVE ( 'NONE', #22295, #32366, #28935, .T. ) ;
#9972 = CARTESIAN_POINT ( 'NONE',  ( 0.000000000000000000, 1.975651141462238858, 10.82112760146736719 ) ) ;
#9973 = VERTEX_POINT ( 'NONE', #28632 ) ;
#9974 = CARTESIAN_POINT ( 'NONE',  ( 21.17250000273118715, 2.378061970571979433, -1.291182301015470602 ) ) ;
#9975 = CARTESIAN_POINT ( 'NONE',  ( -4.250050802731187183, 1.887961173149511618, 2.331437884370912705 ) ) ;
#9976 = DIRECTION ( 'NONE',  ( -0.03488359650710735893, -0.9989355049964836475, 0.03018263660036427792 ) ) ;
#9977 = CARTESIAN_POINT ( 'NONE',  ( 0.000000000000000000, 0.000000000000000000, 0.000000000000000000 ) ) ;
#9978 = EDGE_CURVE ( 'NONE', #30423, #6480, #5583, .T. ) ;
#9979 = DIRECTION ( 'NONE',  ( 1.000000000000000000, 0.000000000000000000, 0.000000000000000000 ) ) ;
#9980 = CARTESIAN_POINT ( 'NONE',  ( -7.150050802731187538, -2.983565686104819648, -0.3135853898029605791 ) ) ;
#9981 = CARTESIAN_POINT ( 'NONE',  ( -56.42282546612280925, 0.008325373391011687066, -1.141662625959267707 ) ) ;
#9982 = CARTESIAN_POINT ( 'NONE',  ( 18.60402535544292490, -7.603424548862588672, 0.07017451552782096036 ) ) ;
#9983 = VERTEX_POINT ( 'NONE', #23288 ) ;
#9984 = CARTESIAN_POINT ( 'NONE',  ( -5.912550801365592967, -3.675193018007246071, 1.088641768524163167 ) ) ;
#9985 = ORIENTED_EDGE ( 'NONE', *, *, #11427, .T. ) ;
#9986 = CARTESIAN_POINT ( 'NONE',  ( -6.504531657079157370, -0.3127741368606806738, 2.975847129947406522 ) ) ;
#9987 = CARTESIAN_POINT ( 'NONE',  ( 21.98500000136559507, -0.9349337715887248157, 3.156283516753367824 ) ) ;
#9988 = CARTESIAN_POINT ( 'NONE',  ( 108.0119342731779284, 18.24461466697532686, 4.475534541203948891 ) ) ;
#9989 = CARTESIAN_POINT ( 'NONE',  ( 85.45070076415650817, -7.158483446666923378, -2.713652344655543391 ) ) ;
#9990 = CARTESIAN_POINT ( 'NONE',  ( 3.249999999999999556, -6.807171995660629804, 6.478011392632865295 ) ) ;
#9991 = EDGE_LOOP ( 'NONE', ( #15353, #14610 ) ) ;
#9992 = CARTESIAN_POINT ( 'NONE',  ( 0.1255855353822278031, 9.314797388872380068, 5.239665997526921970 ) ) ;
#9993 =( BOUNDED_CURVE ( )  B_SPLINE_CURVE ( 3, ( #9735, #11737, #19274, #22129 ),
 .UNSPECIFIED., .F., .F. ) 
 B_SPLINE_CURVE_WITH_KNOTS ( ( 4, 4 ),
 ( 4.712388980384689674, 6.283185307179586232 ),
 .UNSPECIFIED. ) 
 CURVE ( )  GEOMETRIC_REPRESENTATION_ITEM ( )  RATIONAL_B_SPLINE_CURVE ( ( 1.000000000000000000, 0.8047378541243649375, 0.8047378541243649375, 1.000000000000000000 ) ) 
 REPRESENTATION_ITEM ( '' )  );
#9994 = CARTESIAN_POINT ( 'NONE',  ( 85.13613392229150634, -2.069934983084493751, -2.713652344655542503 ) ) ;
#9995 = VERTEX_POINT ( 'NONE', #27979 ) ;
#9996 = DATE_AND_TIME ( #27710, #2917 ) ;
#9997 = ADVANCED_FACE ( 'NONE', ( #25803 ), #30978, .T. ) ;
#9998 = CARTESIAN_POINT ( 'NONE',  ( 54.97695379321813647, -6.496789110673256928, 4.008637379606954987 ) ) ;
#9999 = ADVANCED_FACE ( 'NONE', ( #2927 ), #15256, .F. ) ;
#10000 = DIRECTION ( 'NONE',  ( 0.1767573132311711093, 0.9842544651762052954, 0.000000000000000000 ) ) ;
#10002 = DIRECTION ( 'NONE',  ( -1.000000000000000000, 8.574039729943019576E-17, -0.000000000000000000 ) ) ;
#10001 = CARTESIAN_POINT ( 'NONE',  ( 0.7632845268398871230, 0.000000000000000000, 0.000000000000000000 ) ) ;
#10003 = ORIENTED_EDGE ( 'NONE', *, *, #12400, .T. ) ;
#10004 = EDGE_CURVE ( 'NONE', #24556, #3406, #12735, .T. ) ;
#10005 = CARTESIAN_POINT ( 'NONE',  ( 107.9916441005483563, -18.73362038781918315, -4.428447085748415724 ) ) ;
#10006 = DIRECTION ( 'NONE',  ( 2.219124775574961157E-17, 0.2588190451025251249, -0.9659258262890670910 ) ) ;
#10007 = CARTESIAN_POINT ( 'NONE',  ( 23.11000000136559507, -2.892927487894331406, 1.570731468192932301 ) ) ;
#10008 = CARTESIAN_POINT ( 'NONE',  ( -3.687509558818933845E-13, 7.944914065997426889, -7.533794289458821680 ) ) ;
#10010 = ORIENTED_EDGE ( 'NONE', *, *, #14179, .F. ) ;
#10009 = CARTESIAN_POINT ( 'NONE',  ( 0.9232102171129921153, 0.000000000000000000, 4.522129901861157819 ) ) ;
#10011 = CARTESIAN_POINT ( 'NONE',  ( -4.662550801365592967, 3.521866450007987037, 0.3701630799359328372 ) ) ;
#10012 = CARTESIAN_POINT ( 'NONE',  ( 107.8941083086932196, 17.58851320481917213, -3.054550927624524626 ) ) ;
#10013 = CARTESIAN_POINT ( 'NONE',  ( -37.80541082197543545, 18.90773822806172433, 1.500000000000000222 ) ) ;
#10014 = CARTESIAN_POINT ( 'NONE',  ( 69.07074218555992218, -6.116471746196562975, -3.993434826118012371 ) ) ;
#10015 = ORIENTED_EDGE ( 'NONE', *, *, #8346, .F. ) ;
#10017 = ORIENTED_EDGE ( 'NONE', *, *, #12640, .T. ) ;
#10016 = CARTESIAN_POINT ( 'NONE',  ( 23.30536738592035562, -17.34558290870699793, 1.520589546897618716 ) ) ;
#10018 = EDGE_CURVE ( 'NONE', #21952, #6718, #6615, .T. ) ;
#10019 = CC_DESIGN_PERSON_AND_ORGANIZATION_ASSIGNMENT ( #3273, #21304, ( #8765 ) ) ;
#10020 = CARTESIAN_POINT ( 'NONE',  ( 7.249760686538667009, 0.000000000000000000, 0.000000000000000000 ) ) ;
#10021 = DIRECTION ( 'NONE',  ( 1.000000000000000000, -0.000000000000000000, -0.000000000000000000 ) ) ;
#10022 = DIRECTION ( 'NONE',  ( -1.000000000000000000, 8.574039729943022041E-17, 1.232595164407830946E-32 ) ) ;
#10023 = FACE_OUTER_BOUND ( 'NONE', #27685, .T. ) ;
#10024 = CARTESIAN_POINT ( 'NONE',  ( -0.05272361993596155066, -14.78973072807761469, -1.745421474541472007 ) ) ;
#10025 = CARTESIAN_POINT ( 'NONE',  ( 10.52034268205830259, -3.641590349731909537, -3.055657119358837992 ) ) ;
#10026 = CARTESIAN_POINT ( 'NONE',  ( 23.87614828266750777, -3.446665583148740719, 0.4367666033252894930 ) ) ;
#10027 = CARTESIAN_POINT ( 'NONE',  ( 102.8580990270160385, -4.820463887425400884, 4.522129901861162260 ) ) ;
#10028 = VERTEX_POINT ( 'NONE', #10240 ) ;
#10029 = LINE ( 'NONE', #7519, #32725 ) ;
#10030 = DATE_TIME_ROLE ( 'creation_date' ) ;
#10031 = ADVANCED_FACE ( 'NONE', ( #10567 ), #20626, .T. ) ;
#10032 = CARTESIAN_POINT ( 'NONE',  ( 3.499999999999999556, 0.000000000000000000, 0.000000000000000000 ) ) ;
#10033 = ORIENTED_EDGE ( 'NONE', *, *, #7356, .T. ) ;
#10034 = CARTESIAN_POINT ( 'NONE',  ( 107.9828715491437094, 18.08278195199847715, -4.992355932524864315 ) ) ;
#10035 = ORIENTED_EDGE ( 'NONE', *, *, #12115, .T. ) ;
#10036 = CARTESIAN_POINT ( 'NONE',  ( -19.57725484400670624, 17.02906325615838767, 1.807551478622768215 ) ) ;
#10038 = ORIENTED_EDGE ( 'NONE', *, *, #10765, .F. ) ;
#10037 = CARTESIAN_POINT ( 'NONE',  ( 18.85997003588157384, -4.742476695819044075, -4.003574682316953570 ) ) ;
#10039 = VERTEX_POINT ( 'NONE', #18091 ) ;
#10040 = CARTESIAN_POINT ( 'NONE',  ( -3.616018626656801960, -10.49347358198851943, 1.500000000000000000 ) ) ;
#10041 = CARTESIAN_POINT ( 'NONE',  ( -7.412550801365592967, -3.368539882008727115, -1.828967928396027842 ) ) ;
#10042 = FACE_OUTER_BOUND ( 'NONE', #31693, .T. ) ;
#10043 = CARTESIAN_POINT ( 'NONE',  ( 107.6226684525294814, -19.86014998405252641, -2.725480252158540839 ) ) ;
#10045 = ORIENTED_EDGE ( 'NONE', *, *, #22824, .T. ) ;
#10044 = LINE ( 'NONE', #20257, #19787 ) ;
#10046 = CARTESIAN_POINT ( 'NONE',  ( 25.25352962636571874, 18.67320858063204270, -1.500000000000117906 ) ) ;
#10047 = DIRECTION ( 'NONE',  ( 1.000000000000000000, -8.574039729943018344E-17, -0.000000000000000000 ) ) ;
#10048 = CARTESIAN_POINT ( 'NONE',  ( -4.161566758114229714, -8.294289541356487661, 1.499999999999999778 ) ) ;
#10049 = CARTESIAN_POINT ( 'NONE',  ( 2.437082469501525850, 10.45536235038314921, -2.117184480729003226 ) ) ;
#10051 = EDGE_LOOP ( 'NONE', ( #25127, #7761, #28582, #31280 ) ) ;
#10050 = LINE ( 'NONE', #15241, #8047 ) ;
#10052 = DIRECTION ( 'NONE',  ( -0.000000000000000000, -1.000000000000000000, -0.000000000000000000 ) ) ;
#10053 = EDGE_CURVE ( 'NONE', #16695, #17980, #23593, .T. ) ;
#10054 = CARTESIAN_POINT ( 'NONE',  ( 23.36000000273119070, 1.942864903642424146, 1.573300977624592534 ) ) ;
#10055 = CARTESIAN_POINT ( 'NONE',  ( 24.86000000136559862, -0.9349337715887248157, 3.156283516753367824 ) ) ;
#10056 = CARTESIAN_POINT ( 'NONE',  ( -60.31029867951531998, -5.485000000000005649, 1.500000000000000000 ) ) ;
#10057 = LINE ( 'NONE', #15399, #25168 ) ;
#10058 = CARTESIAN_POINT ( 'NONE',  ( 21.32535692059145660, -21.82495604402121003, -1.318256435726663955 ) ) ;
#10059 =( BOUNDED_SURFACE ( )  B_SPLINE_SURFACE ( 3, 2, ( 
 ( #19782, #14254, #14761 ),
 ( #26983, #12096, #27639 ),
 ( #24958, #9918, #12244 ),
 ( #27132, #9565, #29991 ) ),
 .UNSPECIFIED., .F., .F., .F. ) 
 B_SPLINE_SURFACE_WITH_KNOTS ( ( 4, 4 ),
 ( 3, 3 ),
 ( 0.000000000000000000, 0.003477590727847893522 ),
 ( 0.000000000000000000, 1.000000000000000000 ),
 .UNSPECIFIED. ) 
 GEOMETRIC_REPRESENTATION_ITEM ( )  RATIONAL_B_SPLINE_SURFACE ( (
 ( 1.000000000000000000, 0.7044453589051415943, 1.000000000000000000),
 ( 1.000000000000000000, 0.7044500455793978322, 1.000000000000000000),
 ( 1.000000000000000000, 0.7044547099242082222, 1.000000000000000000),
 ( 1.000000000000000000, 0.7044593522111542994, 1.000000000000000000) ) ) 
 REPRESENTATION_ITEM ( '' )  SURFACE ( )  );
#10060 = ORIENTED_EDGE ( 'NONE', *, *, #4138, .T. ) ;
#10061 = CARTESIAN_POINT ( 'NONE',  ( 15.28872660057386845, 20.76088595412476678, 4.629213727441584325 ) ) ;
#10062 = DIRECTION ( 'NONE',  ( 0.000000000000000000, 0.08715574274767322327, -0.9961946980917442129 ) ) ;
#10063 = CARTESIAN_POINT ( 'NONE',  ( -5.387550801365593500, -0.3701630799359326152, 3.521866450007987037 ) ) ;
#10064 = ORIENTED_EDGE ( 'NONE', *, *, #26957, .T. ) ;
#10065 = EDGE_CURVE ( 'NONE', #2638, #10880, #31159, .T. ) ;
#10066 = CARTESIAN_POINT ( 'NONE',  ( 12.44989959798878054, 0.000000000000000000, 2.482234843104759392 ) ) ;
#10067 = EDGE_CURVE ( 'NONE', #11832, #16893, #1196, .T. ) ;
#10068 = CARTESIAN_POINT ( 'NONE',  ( 5.489321676144491846, 7.082488557107348370, -3.969109389279891431 ) ) ;
#10069 = CARTESIAN_POINT ( 'NONE',  ( 5.612717990268488499, -8.213645783354285967, 0.1993707932846307540 ) ) ;
#10070 = VERTEX_POINT ( 'NONE', #18587 ) ;
#10071 = DIRECTION ( 'NONE',  ( 1.000000000000000000, -0.000000000000000000, -0.000000000000000000 ) ) ;
#10072 = VERTEX_POINT ( 'NONE', #29442 ) ;
#10073 = CARTESIAN_POINT ( 'NONE',  ( 5.377543748152549874, 2.741043480754926875, 7.530955069117522882 ) ) ;
#10074 = EDGE_LOOP ( 'NONE', ( #18884, #21558, #17332, #19039 ) ) ;
#10075 = CARTESIAN_POINT ( 'NONE',  ( 107.5184162292005539, -18.35373766169381327, 5.121412927745073951 ) ) ;
#10077 = ORIENTED_EDGE ( 'NONE', *, *, #23193, .F. ) ;
#10076 = DIRECTION ( 'NONE',  ( 1.000000000000000000, 0.000000000000000000, 0.000000000000000000 ) ) ;
#10078 = VERTEX_POINT ( 'NONE', #26944 ) ;
#10079 = DIRECTION ( 'NONE',  ( -1.000000000000000000, -0.000000000000000000, -0.000000000000000000 ) ) ;
#10080 = ORIENTED_EDGE ( 'NONE', *, *, #4648, .F. ) ;
#10081 = CARTESIAN_POINT ( 'NONE',  ( -50.60000000000000142, -10.96966150227468972, -1.000000000000000000 ) ) ;
#10083 = ORIENTED_EDGE ( 'NONE', *, *, #23501, .F. ) ;
#10082 = CARTESIAN_POINT ( 'NONE',  ( 1.828104818894226380, -1.262475772535087915, -1.500000000000000000 ) ) ;
#10084 = CARTESIAN_POINT ( 'NONE',  ( 8.161453797571457613, -14.35007110565979183, -1.755185239838192857 ) ) ;
#10085 = CARTESIAN_POINT ( 'NONE',  ( 23.24441267594537308, -21.93876234581703599, -1.082412871821091471 ) ) ;
#10086 = CARTESIAN_POINT ( 'NONE',  ( -17.45597128428593692, -25.93932300454937945, 11.00000000000000000 ) ) ;
#10087 = CARTESIAN_POINT ( 'NONE',  ( 4.749760686538667009, -8.014274990069656823, 8.669741416787380218E-17 ) ) ;
#10088 = CARTESIAN_POINT ( 'NONE',  ( -30.51827900900860158, 4.845260731991870351, 5.128141679950118714 ) ) ;
#10089 = CARTESIAN_POINT ( 'NONE',  ( 0.08473242718134026130, -9.416612898531354858, 5.239665997526856245 ) ) ;
#10090 = CARTESIAN_POINT ( 'NONE',  ( 25.43628654896174623, -17.54453578616395149, 1.000000000000000444 ) ) ;
#10091 = CARTESIAN_POINT ( 'NONE',  ( -4.637780547552199373, -6.332425682048902438, 0.9788672205877712029 ) ) ;
#10092 = CARTESIAN_POINT ( 'NONE',  ( 0.8407900506754618641, -11.56055812333405441, 4.522129901861156931 ) ) ;
#10093 = DIRECTION ( 'NONE',  ( 0.000000000000000000, 5.782411586589358033E-15, -1.000000000000000000 ) ) ;
#10094 = DIRECTION ( 'NONE',  ( 0.000000000000000000, 0.000000000000000000, 1.000000000000000000 ) ) ;
#10095 = EDGE_CURVE ( 'NONE', #448, #30410, #10910, .T. ) ;
#10096 = CARTESIAN_POINT ( 'NONE',  ( 41.44346753120584026, -6.883984642623635963, 5.695980980372492120 ) ) ;
#10097 = ADVANCED_FACE ( 'NONE', ( #11218 ), #24263, .T. ) ;
#10098 = CARTESIAN_POINT ( 'NONE',  ( -3.950050802731187360, -2.983565686104819648, -0.3135853898029605791 ) ) ;
#10099 = ORIENTED_EDGE ( 'NONE', *, *, #20101, .F. ) ;
#10100 = EDGE_CURVE ( 'NONE', #22217, #15150, #32158, .T. ) ;
#10101 = CARTESIAN_POINT ( 'NONE',  ( -6.487550801365593145, 2.752080473201636845, -2.228590825266444142 ) ) ;
#10102 = CARTESIAN_POINT ( 'NONE',  ( -3.830085165118321606E-16, -4.467071865485483961, 1.625881193364682620 ) ) ;
#10103 = CARTESIAN_POINT ( 'NONE',  ( 0.000000000000000000, 0.5000000000000000000, 1.000000000000000000 ) ) ;
#10104 = VERTEX_POINT ( 'NONE', #26460 ) ;
#10105 = CARTESIAN_POINT ( 'NONE',  ( 5.612974441954673210, -5.126870824538720228, -6.420536856479988508 ) ) ;
#10106 = ORIENTED_EDGE ( 'NONE', *, *, #11753, .T. ) ;
#10107 = CARTESIAN_POINT ( 'NONE',  ( 18.53107884607683076, -16.42960242685250449, 1.500000000000000000 ) ) ;
#10108 = COORDINATED_UNIVERSAL_TIME_OFFSET ( 0, 0, .AHEAD. ) ;
#10110 = ORIENTED_EDGE ( 'NONE', *, *, #14920, .T. ) ;
#10109 = DIRECTION ( 'NONE',  ( 0.000000000000000000, 0.000000000000000000, 1.000000000000000000 ) ) ;
#10111 = EDGE_LOOP ( 'NONE', ( #14561, #13120, #31791, #24702 ) ) ;
#10112 = CARTESIAN_POINT ( 'NONE',  ( 107.6641398346805545, -20.45810202417278134, -1.500000000000000000 ) ) ;
#10113 = VERTEX_POINT ( 'NONE', #8391 ) ;
#10114 = VECTOR ( 'NONE', #9427, 1000.000000000000000 ) ;
#10115 = CARTESIAN_POINT ( 'NONE',  ( 107.9932960675740219, -17.97282715741293302, -4.597091762064528631 ) ) ;
#10117 = ORIENTED_EDGE ( 'NONE', *, *, #24107, .T. ) ;
#10116 = FACE_OUTER_BOUND ( 'NONE', #8967, .T. ) ;
#10118 = CARTESIAN_POINT ( 'NONE',  ( 3.063284526839887167, 8.734705317681626724, -0.4999240074894737984 ) ) ;
#10119 = CYLINDRICAL_SURFACE ( 'NONE', #28331, 2.999999999999999112 ) ;
#10120 = CARTESIAN_POINT ( 'NONE',  ( 21.68866787702163634, -21.76712446977036919, -1.490904000146909159 ) ) ;
#10121 = CARTESIAN_POINT ( 'NONE',  ( -6.562942409646512765, -8.831141768130910875E-16, 2.999999999999999556 ) ) ;
#10122 = ORIENTED_EDGE ( 'NONE', *, *, #25580, .T. ) ;
#10123 = CARTESIAN_POINT ( 'NONE',  ( 5.612718825656738630, -6.163864706063985288, 5.432357446996388006 ) ) ;
#10124 = CARTESIAN_POINT ( 'NONE',  ( 107.1772993348646281, 16.40207914262226296, -1.491740999229418829 ) ) ;
#10125 = LINE ( 'NONE', #20349, #4875 ) ;
#10126 = CARTESIAN_POINT ( 'NONE',  ( 41.43369393131069245, -3.642920876114430495, -2.713652344655540727 ) ) ;
#10127 = EDGE_CURVE ( 'NONE', #13648, #20515, #4047, .T. ) ;
#10128 = CARTESIAN_POINT ( 'NONE',  ( 24.55981180825490640, -17.46058140477835963, 1.484973660491783143 ) ) ;
#10129 = DIRECTION ( 'NONE',  ( 0.000000000000000000, -1.000000000000000000, 0.000000000000000000 ) ) ;
#10130 = CARTESIAN_POINT ( 'NONE',  ( -56.37198679362065690, 0.002873736814589079782, -1.088637985230049621 ) ) ;
#10131 = DIRECTION ( 'NONE',  ( 0.000000000000000000, 0.4226182617407029385, -0.9063077870366482713 ) ) ;
#10132 = AXIS2_PLACEMENT_3D ( 'NONE', #29131, #5737, #15600 ) ;
#10133 = ORIENTED_EDGE ( 'NONE', *, *, #33071, .F. ) ;
#10134 = CARTESIAN_POINT ( 'NONE',  ( -5.762550801365593500, -2.228590825266444586, -2.752080473201636401 ) ) ;
#10135 = VERTEX_POINT ( 'NONE', #28776 ) ;
#10136 = ADVANCED_FACE ( 'NONE', ( #13564 ), #1378, .T. ) ;
#10137 = CARTESIAN_POINT ( 'NONE',  ( -5.054531657079158968, 2.846291840500173365, 1.545410377633946952 ) ) ;
#10138 = VECTOR ( 'NONE', #28118, 1000.000000000000000 ) ;
#10139 = CARTESIAN_POINT ( 'NONE',  ( 21.54750000136559507, 1.913930629741522838, -2.363507492473150062 ) ) ;
#10140 = EDGE_CURVE ( 'NONE', #9712, #10425, #3411, .T. ) ;
#10141 = FACE_OUTER_BOUND ( 'NONE', #1800, .T. ) ;
#10142 = CARTESIAN_POINT ( 'NONE',  ( 0.1152454363327600484, -6.520582226636352452, 1.773866594758318538 ) ) ;
#10143 = CARTESIAN_POINT ( 'NONE',  ( 107.9622325421415212, 20.81773585569407459, 1.508259000770582059 ) ) ;
#10144 = EDGE_LOOP ( 'NONE', ( #15954, #27666, #4329, #1575 ) ) ;
#10145 = CARTESIAN_POINT ( 'NONE',  ( 19.01480233880806381, -3.011762293215139330, 0.07017451552781951707 ) ) ;
#10146 = DIRECTION ( 'NONE',  ( -0.000000000000000000, -0.000000000000000000, -1.000000000000000000 ) ) ;
#10147 = EDGE_LOOP ( 'NONE', ( #17745, #28750, #1844, #21459 ) ) ;
#10148 = CARTESIAN_POINT ( 'NONE',  ( 5.612718383992088889, 1.622626842546764259, 8.054241895195636047 ) ) ;
#10149 = COORDINATED_UNIVERSAL_TIME_OFFSET ( 0, 0, .AHEAD. ) ;
#10150 = EDGE_CURVE ( 'NONE', #13056, #18479, #19244, .T. ) ;
#10151 = AXIS2_PLACEMENT_3D ( 'NONE', #8994, #17197, #24535 ) ;
#10152 = CARTESIAN_POINT ( 'NONE',  ( 54.97626768014088583, -6.471998454829187786, 4.043900691106972367 ) ) ;
#10153 = CIRCLE ( 'NONE', #2686, 0.5000000000000000000 ) ;
#10154 = CARTESIAN_POINT ( 'NONE',  ( 107.4500373638809947, -17.36019379023286646, 4.522129901861156931 ) ) ;
#10155 = CIRCLE ( 'NONE', #6961, 2.999999999999999556 ) ;
#10157 = CARTESIAN_POINT ( 'NONE',  ( 7.249760686538667009, 7.953573330858264789, -3.647351267791489882 ) ) ;
#10156 = CARTESIAN_POINT ( 'NONE',  ( 109.0479424394436734, 18.35604238244625819, -5.421472302580672142 ) ) ;
#10158 = VERTEX_POINT ( 'NONE', #11400 ) ;
#10159 = ADVANCED_FACE ( 'NONE', ( #29123 ), #11070, .F. ) ;
#10160 = DIRECTION ( 'NONE',  ( 0.4999999999999978906, 0.8660254037844398178, -0.000000000000000000 ) ) ;
#10161 = CARTESIAN_POINT ( 'NONE',  ( -52.69999999999999574, -10.96966150227468972, 7.500000000000000000 ) ) ;
#10162 = CARTESIAN_POINT ( 'NONE',  ( 23.23500000136559862, -3.156283516753370044, -0.9349337715887220401 ) ) ;
#10163 = CARTESIAN_POINT ( 'NONE',  ( 0.000000000000000000, 0.000000000000000000, 0.000000000000000000 ) ) ;
#10164 = AXIS2_PLACEMENT_3D ( 'NONE', #17927, #8969, #19684 ) ;
#10166 = ORIENTED_EDGE ( 'NONE', *, *, #16396, .T. ) ;
#10165 = DIRECTION ( 'NONE',  ( 0.000000000000000000, -0.9961946980917444350, -0.08715574274767159957 ) ) ;
#10167 = CARTESIAN_POINT ( 'NONE',  ( -7.562550801365593323, -2.752080473201636845, 2.228590825266444586 ) ) ;
#10168 = DIRECTION ( 'NONE',  ( 0.000000000000000000, 0.000000000000000000, 1.000000000000000000 ) ) ;
#10169 = EDGE_CURVE ( 'NONE', #10511, #32781, #132, .T. ) ;
#10170 = LINE ( 'NONE', #25238, #3344 ) ;
#10171 = CARTESIAN_POINT ( 'NONE',  ( 107.5617723795401872, -18.98359893170738744, -4.522129901861166701 ) ) ;
#10172 = ORIENTED_EDGE ( 'NONE', *, *, #31622, .T. ) ;
#10174 = ORIENTED_EDGE ( 'NONE', *, *, #3468, .T. ) ;
#10173 = CARTESIAN_POINT ( 'NONE',  ( 0.5640492184783271190, 3.576105523027020894, -8.844377740304885549 ) ) ;
#10175 = CARTESIAN_POINT ( 'NONE',  ( 24.08745121460989225, -17.31475877198389668, -1.374955925957151992 ) ) ;
#10176 = CARTESIAN_POINT ( 'NONE',  ( 107.7448119175622736, 19.60714374054428788, -4.075483440861804141 ) ) ;
#10177 = AXIS2_PLACEMENT_3D ( 'NONE', #24550, #4028, #14196 ) ;
#10178 = EDGE_CURVE ( 'NONE', #7714, #15085, #11896, .T. ) ;
#10179 = EDGE_CURVE ( 'NONE', #27014, #4554, #4927, .T. ) ;
#10180 = CARTESIAN_POINT ( 'NONE',  ( 23.36000000136559507, -1.570731468192933633, -2.892927487894330962 ) ) ;
#10181 = CIRCLE ( 'NONE', #4846, 5.000000000000001776 ) ;
#10182 = CARTESIAN_POINT ( 'NONE',  ( 7.249760686538667009, -4.973063321323826003, -7.199384779417172808 ) ) ;
#10183 = CARTESIAN_POINT ( 'NONE',  ( 2.288217443798745698, -16.46508028272004154, -1.747280182634695977 ) ) ;
#10184 = DIRECTION ( 'NONE',  ( -1.000000000000000000, 0.000000000000000000, 0.000000000000000000 ) ) ;
#10185 = CIRCLE ( 'NONE', #23005, 297.9387600756452912 ) ;
#10186 =( BOUNDED_CURVE ( )  B_SPLINE_CURVE ( 2, ( #597, #784, #23187, #10790, #18489, #28682, #5286, #10965, #8441, #31365, #5930 ),
 .UNSPECIFIED., .F., .F. ) 
 B_SPLINE_CURVE_WITH_KNOTS ( ( 3, 2, 2, 2, 2, 3 ),
 ( 0.1228822619934377414, 0.1250000000000000000, 0.1406250000000000000, 0.1562500000000000000, 0.1718750000000000000, 0.1853822619934377414 ),
 .UNSPECIFIED. ) 
 CURVE ( )  GEOMETRIC_REPRESENTATION_ITEM ( )  RATIONAL_B_SPLINE_CURVE ( ( 0.9821626249036861100, 0.9896829947469993893, 1.000000000000000000, 0.9238795325112867385, 1.000000000000000000, 0.9238795325112867385, 1.000000000000000000, 0.9238795325112867385, 1.000000000000000000, 0.9341965377642873491, 0.9821626249036861100 ) ) 
 REPRESENTATION_ITEM ( '' )  );
#10187 = CARTESIAN_POINT ( 'NONE',  ( 23.87614828266729461, -3.446665583135212874, 0.07017451549142075806 ) ) ;
#10188 = CARTESIAN_POINT ( 'NONE',  ( 107.9116956367129205, -16.79780125264633384, 2.301619431081807221 ) ) ;
#10189 = ORIENTED_EDGE ( 'NONE', *, *, #8146, .T. ) ;
#10190 = EDGE_CURVE ( 'NONE', #22736, #29357, #32624, .T. ) ;
#10191 = CARTESIAN_POINT ( 'NONE',  ( 0.3803104029207236003, -8.653113404385461394, 5.199400874759553481 ) ) ;
#10192 = CIRCLE ( 'NONE', #18739, 10.99999999999999822 ) ;
#10193 = APPROVAL_ROLE ( '' ) ;
#10194 = CARTESIAN_POINT ( 'NONE',  ( 0.000000000000000000, 37.67766952966368876, -3.750000000000000444 ) ) ;
#10195 = ORIENTED_EDGE ( 'NONE', *, *, #24583, .F. ) ;
#10196 = EDGE_CURVE ( 'NONE', #29352, #9973, #22101, .T. ) ;
#10197 = DIRECTION ( 'NONE',  ( 0.000000000000000000, 0.000000000000000000, 1.000000000000000000 ) ) ;
#10198 = ORIENTED_EDGE ( 'NONE', *, *, #16053, .T. ) ;
#10199 = CARTESIAN_POINT ( 'NONE',  ( -5.356376981307136909, 0.1572233378491222633, -3.000000000000000000 ) ) ;
#10201 = ORIENTED_EDGE ( 'NONE', *, *, #740, .T. ) ;
#10200 = CARTESIAN_POINT ( 'NONE',  ( 28.69289731897472961, -5.642913542083610956, -4.033870043669357308 ) ) ;
#10202 = AXIS2_PLACEMENT_3D ( 'NONE', #23835, #13945, #11467 ) ;
#10203 = ORIENTED_EDGE ( 'NONE', *, *, #15715, .F. ) ;
#10204 = CARTESIAN_POINT ( 'NONE',  ( -2.253815017383504316, 1.323625320507515690, 3.284597389079958685 ) ) ;
#10205 = DIRECTION ( 'NONE',  ( 0.000000000000000000, -0.5735764363510447161, -0.8191520442889927978 ) ) ;
#10206 = CIRCLE ( 'NONE', #31045, 6.999999999999998224 ) ;
#10207 = DIRECTION ( 'NONE',  ( 1.000000000000000000, 0.000000000000000000, -0.000000000000000000 ) ) ;
#10208 = VECTOR ( 'NONE', #5339, 1000.000000000000000 ) ;
#10209 = CARTESIAN_POINT ( 'NONE',  ( 102.9885081044300676, -6.698322160490901567, -0.07017451552783579571 ) ) ;
#10211 = ORIENTED_EDGE ( 'NONE', *, *, #26098, .T. ) ;
#10210 = LINE ( 'NONE', #25775, #32617 ) ;
#10212 = CARTESIAN_POINT ( 'NONE',  ( 107.6337546485926993, -20.01978338540836688, 2.398305884358065576 ) ) ;
#10213 = AXIS2_PLACEMENT_3D ( 'NONE', #23374, #478, #31746 ) ;
#10214 = CARTESIAN_POINT ( 'NONE',  ( 26.23173791223905837, 19.12152673998438601, 1.500000000000000000 ) ) ;
#10215 = CARTESIAN_POINT ( 'NONE',  ( -3.111318361680354805, -11.33170398610737450, 1.499999999999761080 ) ) ;
#10216 = AXIS2_PLACEMENT_3D ( 'NONE', #12750, #26132, #20958 ) ;
#10217 = CARTESIAN_POINT ( 'NONE',  ( 4.749760686538667009, 1.391664247347228045, 7.892520144992438702 ) ) ;
#10220 = EDGE_CURVE ( 'NONE', #8881, #8276, #14555, .T. ) ;
#10219 = ORIENTED_EDGE ( 'NONE', *, *, #30660, .T. ) ;
#10218 = CARTESIAN_POINT ( 'NONE',  ( 108.0286880956687412, -18.48246355754853454, -4.344949451024058718 ) ) ;
#10221 = CYLINDRICAL_SURFACE ( 'NONE', #26895, 0.5000000000000000000 ) ;
#10222 = VECTOR ( 'NONE', #12333, 1000.000000000000000 ) ;
#10223 = VECTOR ( 'NONE', #3124, 1000.000000000000000 ) ;
#10224 = CARTESIAN_POINT ( 'NONE',  ( -24.68599574654897211, 18.35914888252920463, 1.775473033787586363 ) ) ;
#10225 = CARTESIAN_POINT ( 'NONE',  ( 24.36000000273118715, 1.942864903642424146, 1.573300977624592534 ) ) ;
#10226 = ADVANCED_FACE ( 'NONE', ( #19433 ), #21992, .T. ) ;
#10227 = FACE_OUTER_BOUND ( 'NONE', #2894, .T. ) ;
#10228 = CARTESIAN_POINT ( 'NONE',  ( 3.063284526839887167, 5.538577986808899567, 6.772677083992407532 ) ) ;
#10229 = CARTESIAN_POINT ( 'NONE',  ( 17.33093461831547444, -21.43932300456618378, -1.500000000000000000 ) ) ;
#10230 = ORIENTED_EDGE ( 'NONE', *, *, #31449, .T. ) ;
#10231 = CARTESIAN_POINT ( 'NONE',  ( 0.000000000000000000, 0.000000000000000000, 0.000000000000000000 ) ) ;
#10232 = VECTOR ( 'NONE', #19076, 1000.000000000000000 ) ;
#10233 = MANIFOLD_SOLID_BREP ( 'Fillet2', #28586 ) ;
#10234 = LINE ( 'NONE', #25457, #27900 ) ;
#10235 = CARTESIAN_POINT ( 'NONE',  ( -5.887550801365593500, -2.228590825266444586, -2.752080473201636401 ) ) ;
#10236 = ORIENTED_EDGE ( 'NONE', *, *, #17075, .F. ) ;
#10237 = AXIS2_PLACEMENT_3D ( 'NONE', #24830, #22167, #21815 ) ;
#10238 = VECTOR ( 'NONE', #565, 1000.000000000000000 ) ;
#10239 = CIRCLE ( 'NONE', #10793, 5.009999999999999787 ) ;
#10240 = CARTESIAN_POINT ( 'NONE',  ( -5.520790571833112281, 0.5174497483512503493, -5.764727407554744332 ) ) ;
#10241 = FACE_BOUND ( 'NONE', #25520, .T. ) ;
#10242 = CARTESIAN_POINT ( 'NONE',  ( 13.13178786249840435, -17.31629153505178920, -4.522129901861164925 ) ) ;
#10244 = CARTESIAN_POINT ( 'NONE',  ( 24.24719734710406627, -17.18125539888338693, 1.000000000000000222 ) ) ;
#10243 = VECTOR ( 'NONE', #17883, 999.9999999999998863 ) ;
#10245 = VERTEX_POINT ( 'NONE', #4701 ) ;
#10246 = VECTOR ( 'NONE', #2246, 999.9999999999998863 ) ;
#10247 = EDGE_CURVE ( 'NONE', #28172, #29681, #22255, .T. ) ;
#10248 = AXIS2_PLACEMENT_3D ( 'NONE', #9496, #12673, #17376 ) ;
#10249 = FACE_OUTER_BOUND ( 'NONE', #32607, .T. ) ;
#10250 = ORIENTED_EDGE ( 'NONE', *, *, #27657, .T. ) ;
#10251 = CARTESIAN_POINT ( 'NONE',  ( -3.958196854299262826E-16, -4.616489984850546513, 1.946309384392575392 ) ) ;
#10253 = VERTEX_POINT ( 'NONE', #19583 ) ;
#10252 = FACE_OUTER_BOUND ( 'NONE', #11751, .T. ) ;
#10254 = VERTEX_POINT ( 'NONE', #1530 ) ;
#10255 = CARTESIAN_POINT ( 'NONE',  ( -31.69719015456885103, -21.93932300455405482, 1.000000000000000444 ) ) ;
#10256 = VERTEX_POINT ( 'NONE', #27256 ) ;
#10257 = DIRECTION ( 'NONE',  ( 0.1436597682917715446, 0.03489949670250103858, -0.9890115753135888532 ) ) ;
#10259 = ORIENTED_EDGE ( 'NONE', *, *, #7361, .F. ) ;
#10258 = CARTESIAN_POINT ( 'NONE',  ( 12.65465643788354200, -15.70291107026620914, 1.500000000000000000 ) ) ;
#10260 = AXIS2_PLACEMENT_3D ( 'NONE', #31908, #6469, #11014 ) ;
#10261 = CARTESIAN_POINT ( 'NONE',  ( 0.5105742983572999494, -4.179359922481789447, -1.765450449227109919 ) ) ;
#10262 = CIRCLE ( 'NONE', #29473, 6.818740222761507042 ) ;
#10263 = DIRECTION ( 'NONE',  ( 0.4851627901281758692, 0.000000000000000000, -0.8744238486426610946 ) ) ;
#10264 = AXIS2_PLACEMENT_3D ( 'NONE', #29187, #6274, #22281 ) ;
#10265 = DIRECTION ( 'NONE',  ( 0.000000000000000000, 0.000000000000000000, -1.000000000000000000 ) ) ;
#10266 = DIRECTION ( 'NONE',  ( 1.000000000000000000, 0.000000000000000000, 0.000000000000000000 ) ) ;
#10267 = EDGE_CURVE ( 'NONE', #16936, #16263, #26280, .T. ) ;
#10268 = AXIS2_PLACEMENT_3D ( 'NONE', #13077, #5717, #13372 ) ;
#10269 = VECTOR ( 'NONE', #9274, 1000.000000000000000 ) ;
#10270 = ADVANCED_FACE ( 'NONE', ( #1885 ), #21909, .T. ) ;
#10271 = CARTESIAN_POINT ( 'NONE',  ( 7.249760686538667009, 8.721381771256204729, 0.7071067811865429098 ) ) ;
#10272 = CARTESIAN_POINT ( 'NONE',  ( 34.48223484310472031, 0.5000000000000000000, -2.552009564962229859 ) ) ;
#10273 = PLANE ( 'NONE',  #25329 ) ;
#10274 = CIRCLE ( 'NONE', #24645, 0.5000000000000000000 ) ;
#10275 = DIRECTION ( 'NONE',  ( 1.000000000000000000, -0.000000000000000000, -0.000000000000000000 ) ) ;
#10276 = CARTESIAN_POINT ( 'NONE',  ( 84.65816297383790356, -6.961284151106942097, -0.07017451552783579571 ) ) ;
#10277 = DIRECTION ( 'NONE',  ( 1.000000000000000000, -8.574039729943018344E-17, -0.000000000000000000 ) ) ;
#10278 = CARTESIAN_POINT ( 'NONE',  ( 29.27523314209665983, -3.695744416148424527, -0.07017451552781628354 ) ) ;
#10279 = DIRECTION ( 'NONE',  ( 0.000000000000000000, -0.9063077870366558209, 0.4226182617406868403 ) ) ;
#10280 = CARTESIAN_POINT ( 'NONE',  ( -4.150050802731187538, -0.3135853898029607456, 2.983565686104819648 ) ) ;
#10281 = VERTEX_POINT ( 'NONE', #4549 ) ;
#10282 = CARTESIAN_POINT ( 'NONE',  ( -6.187550801365593323, -0.3701630799359326152, 3.521866450007987037 ) ) ;
#10283 = CIRCLE ( 'NONE', #10810, 2.999999999999999556 ) ;
#10284 = B_SPLINE_CURVE_WITH_KNOTS ( 'NONE', 3,
 ( #8051, #17761, #18085, #12579, #28467, #2920, #28276, #4893, #5072, #25453 ),
 .UNSPECIFIED., .F., .F.,
 ( 4, 2, 2, 2, 4 ),
 ( 2.571685856657688708E-07, 0.0005478592107668812028, 0.001095461252948096761, 0.001643063295129312210, 0.002190665337310527660 ),
 .UNSPECIFIED. ) ;
#10285 = DIRECTION ( 'NONE',  ( 0.4851627901281774236, 0.000000000000000000, 0.8744238486426602064 ) ) ;
#10286 = DIRECTION ( 'NONE',  ( -1.000000000000000000, -0.000000000000000000, -0.000000000000000000 ) ) ;
#10288 = VERTEX_POINT ( 'NONE', #14722 ) ;
#10287 = VECTOR ( 'NONE', #31577, 1000.000000000000000 ) ;
#10289 = CARTESIAN_POINT ( 'NONE',  ( 2.274274201625327230, 0.000000000000000000, 0.000000000000000000 ) ) ;
#10290 = DIRECTION ( 'NONE',  ( -1.000000000000000000, 0.000000000000000000, -8.654346879536960414E-15 ) ) ;
#10291 = TOROIDAL_SURFACE ( 'NONE', #28985, 4.499999999999997335, 0.5000000000000000000 ) ;
#10292 = VECTOR ( 'NONE', #6889, 1000.000000000000000 ) ;
#10293 = ORIENTED_EDGE ( 'NONE', *, *, #6755, .F. ) ;
#10294 = COORDINATED_UNIVERSAL_TIME_OFFSET ( 0, 0, .AHEAD. ) ;
#10295 = CIRCLE ( 'NONE', #32721, 0.4499999999999990119 ) ;
#10297 = ORIENTED_EDGE ( 'NONE', *, *, #17866, .T. ) ;
#10296 = DIRECTION ( 'NONE',  ( 0.000000000000000000, 0.000000000000000000, 1.000000000000000000 ) ) ;
#10298 = VERTEX_POINT ( 'NONE', #29627 ) ;
#10299 = DIRECTION ( 'NONE',  ( 0.000000000000000000, 0.000000000000000000, 1.000000000000000000 ) ) ;
#10300 = AXIS2_PLACEMENT_3D ( 'NONE', #11982, #16973, #24486 ) ;
#10301 = CIRCLE ( 'NONE', #8158, 3.250000000000002665 ) ;
#10302 = VERTEX_POINT ( 'NONE', #32127 ) ;
#10303 = DIRECTION ( 'NONE',  ( -7.472768010110281180E-18, -0.08715574274764853469, -0.9961946980917464334 ) ) ;
#10305 = ORIENTED_EDGE ( 'NONE', *, *, #25623, .T. ) ;
#10304 = CARTESIAN_POINT ( 'NONE',  ( -2.477544768930361130, -0.1796242917493272861, 3.046506040574583185 ) ) ;
#10306 = CARTESIAN_POINT ( 'NONE',  ( 29.18953645666585572, -9.308308156628573471, 1.010822989962089746 ) ) ;
#10307 = CARTESIAN_POINT ( 'NONE',  ( 2.274274201620948510, 9.915734732518576067, -4.762163868927066446 ) ) ;
#10308 = ADVANCED_FACE ( 'NONE', ( #24920 ), #12205, .T. ) ;
#10309 = PLANE ( 'NONE',  #2363 ) ;
#10310 = LINE ( 'NONE', #20529, #7643 ) ;
#10311 = EDGE_CURVE ( 'NONE', #28455, #9295, #1724, .T. ) ;
#10312 = ORIENTED_EDGE ( 'NONE', *, *, #17575, .T. ) ;
#10313 = CIRCLE ( 'NONE', #25809, 4.000000000000001776 ) ;
#10314 = EDGE_CURVE ( 'NONE', #12294, #9818, #32241, .T. ) ;
#10315 = AXIS2_PLACEMENT_3D ( 'NONE', #24221, #6486, #1340 ) ;
#10316 = CARTESIAN_POINT ( 'NONE',  ( 2.600000000000000089, -0.5000000000000000000, 1.500000000000000000 ) ) ;
#10317 = DIRECTION ( 'NONE',  ( 0.000000000000000000, -0.5735764363510565955, 0.8191520442889845821 ) ) ;
#10318 = CARTESIAN_POINT ( 'NONE',  ( 9.999999999999998224, -4.681538312723512618, -0.8254815157535732029 ) ) ;
#10319 = TOROIDAL_SURFACE ( 'NONE', #6566, 4.499999999999997335, 0.5000000000000000000 ) ;
#10320 = CIRCLE ( 'NONE', #23144, 3.024999999999999911 ) ;
#10321 = AXIS2_PLACEMENT_3D ( 'NONE', #16388, #3555, #8871 ) ;
#10322 = CARTESIAN_POINT ( 'NONE',  ( 23.20536337411656902, -21.93817982951601664, 1.034580775994869528 ) ) ;
#10323 = DIRECTION ( 'NONE',  ( -0.000000000000000000, -0.000000000000000000, 1.000000000000000000 ) ) ;
#10324 = CARTESIAN_POINT ( 'NONE',  ( -56.31570190716953306, 0.1700137493292786239, -1.377075300692550908 ) ) ;
#10325 = DIRECTION ( 'NONE',  ( -0.000000000000000000, 0.9063077870366511579, -0.4226182617406968323 ) ) ;
#10326 = ORIENTED_EDGE ( 'NONE', *, *, #31797, .F. ) ;
#10327 = CC_DESIGN_APPROVAL ( #3324, ( #4466 ) ) ;
#10328 = CARTESIAN_POINT ( 'NONE',  ( -6.712550801365593678, -3.675193018007246071, 1.088641768524163167 ) ) ;
#10329 = ORIENTED_EDGE ( 'NONE', *, *, #29608, .T. ) ;
#10330 = CARTESIAN_POINT ( 'NONE',  ( -3.104531657079157458, -2.975847129947406522, -0.3127741368606805072 ) ) ;
#10331 = CARTESIAN_POINT ( 'NONE',  ( 107.5865239920538698, 18.70770258647741358, 5.148154074928823043 ) ) ;
#10332 = CARTESIAN_POINT ( 'NONE',  ( 0.6825714480081905844, -9.110483382199172198, 1.769152918636197835 ) ) ;
#10333 = CARTESIAN_POINT ( 'NONE',  ( 13.25896750271793145, -14.28336940137698541, 1.500000000000000000 ) ) ;
#10334 = EDGE_LOOP ( 'NONE', ( #22980, #19725, #7910, #15449 ) ) ;
#10335 = CYLINDRICAL_SURFACE ( 'NONE', #27915, 4.000000000000001776 ) ;
#10336 = AXIS2_PLACEMENT_3D ( 'NONE', #21450, #26969, #8750 ) ;
#10337 = VERTEX_POINT ( 'NONE', #16675 ) ;
#10338 = CARTESIAN_POINT ( 'NONE',  ( 2.970200390942824509, -0.5647484629966927905, -9.143933199822400937 ) ) ;
#10340 = AXIS2_PLACEMENT_3D ( 'NONE', #25460, #2730, #23127 ) ;
#10339 = COORDINATED_UNIVERSAL_TIME_OFFSET ( 0, 0, .AHEAD. ) ;
#10341 = CARTESIAN_POINT ( 'NONE',  ( 85.03004892703806661, -5.110667302027010805, 4.112223744664014191 ) ) ;
#10342 = AXIS2_PLACEMENT_3D ( 'NONE', #28859, #11308, #5959 ) ;
#10343 = VECTOR ( 'NONE', #20667, 1000.000000000000000 ) ;
#10344 = VECTOR ( 'NONE', #26927, 1000.000000000000000 ) ;
#10345 = EDGE_CURVE ( 'NONE', #7709, #16071, #17810, .T. ) ;
#10346 = DIRECTION ( 'NONE',  ( -1.000000000000000000, -0.000000000000000000, -0.000000000000000000 ) ) ;
#10348 = CARTESIAN_POINT ( 'NONE',  ( 3.063284526839887167, 0.000000000000000000, 0.000000000000000000 ) ) ;
#10347 = CARTESIAN_POINT ( 'NONE',  ( 109.0732318695909129, 18.49686390823877957, -5.382000293758435028 ) ) ;
#10349 = ORIENTED_EDGE ( 'NONE', *, *, #19060, .T. ) ;
#10350 = SECURITY_CLASSIFICATION ( '', '', #21527 ) ;
#10351 = FACE_BOUND ( 'NONE', #16593, .T. ) ;
#10352 = CARTESIAN_POINT ( 'NONE',  ( 2.274274201625327230, 10.82112760146739028, -1.975651141462127391 ) ) ;
#10353 = CARTESIAN_POINT ( 'NONE',  ( 25.11000000136559507, -2.892927487894331406, 1.570731468192932301 ) ) ;
#10354 = DIRECTION ( 'NONE',  ( 0.000000000000000000, 0.8191520442889909104, 0.5735764363510474917 ) ) ;
#10356 = EDGE_LOOP ( 'NONE', ( #27096, #7547, #9945, #25389 ) ) ;
#10355 = CARTESIAN_POINT ( 'NONE',  ( 41.92799935459299832, -21.01937708444107500, 4.522129901861157819 ) ) ;
#10357 = CARTESIAN_POINT ( 'NONE',  ( -6.662550801365592967, -3.521866450007987037, -0.3701630799359323931 ) ) ;
#10358 = DIRECTION ( 'NONE',  ( -1.000000000000000000, -0.000000000000000000, 0.000000000000000000 ) ) ;
#10359 = LINE ( 'NONE', #13178, #7037 ) ;
#10360 = CARTESIAN_POINT ( 'NONE',  ( 0.000000000000000000, 0.000000000000000000, -1.000000000000000000 ) ) ;
#10361 = ORIENTED_EDGE ( 'NONE', *, *, #3830, .T. ) ;
#10363 = ORIENTED_EDGE ( 'NONE', *, *, #9159, .F. ) ;
#10362 = CARTESIAN_POINT ( 'NONE',  ( 23.85741365831481176, -17.28578219493698143, 1.405688364265740065 ) ) ;
#10364 = CIRCLE ( 'NONE', #10888, 11.00000000000000000 ) ;
#10365 = AXIS2_PLACEMENT_3D ( 'NONE', #5978, #21352, #5511 ) ;
#10366 = CARTESIAN_POINT ( 'NONE',  ( -34.30158461016502969, 20.00000000000000000, -1.818740222761504599 ) ) ;
#10367 = CARTESIAN_POINT ( 'NONE',  ( -8.049676575031998738, 0.000000000000000000, 0.000000000000000000 ) ) ;
#10368 = CARTESIAN_POINT ( 'NONE',  ( 22.67250000136559507, 3.024605502323846729, -0.3178988483021056854 ) ) ;
#10369 = CARTESIAN_POINT ( 'NONE',  ( 18.92745801356193169, -3.988096551856957550, 2.787782631236393804 ) ) ;
#10370 = CARTESIAN_POINT ( 'NONE',  ( -50.60000000000000142, -10.96966150227468972, 6.999999999999999112 ) ) ;
#10371 = LINE ( 'NONE', #3031, #10843 ) ;
#10372 = ADVANCED_FACE ( 'NONE', ( #13812 ), #31753, .T. ) ;
#10373 = LOCAL_TIME ( 16, 7, 10.00000000000000000, #24621 ) ;
#10374 = DIRECTION ( 'NONE',  ( 0.000000000000000000, 0.000000000000000000, 1.000000000000000000 ) ) ;
#10375 = CARTESIAN_POINT ( 'NONE',  ( 55.02116481234003942, -8.082960297853386322, 1.169950777205091663 ) ) ;
#10376 = VERTEX_POINT ( 'NONE', #29222 ) ;
#10377 = CARTESIAN_POINT ( 'NONE',  ( 2.274274201627370040, 7.958834565715812381, -7.593217523255793466 ) ) ;
#10378 = EDGE_CURVE ( 'NONE', #2795, #8885, #24655, .T. ) ;
#10379 = CARTESIAN_POINT ( 'NONE',  ( 29.38825086720287771, -3.456623792456554156, 2.713652344655542503 ) ) ;
#10380 = ORIENTED_EDGE ( 'NONE', *, *, #15628, .F. ) ;
#10381 = VECTOR ( 'NONE', #28659, 1000.000000000000000 ) ;
#10382 = CARTESIAN_POINT ( 'NONE',  ( 10.00000000000000178, -3.407865132560208288, 3.672404558090027304 ) ) ;
#10383 = ORIENTED_EDGE ( 'NONE', *, *, #7994, .T. ) ;
#10384 = CARTESIAN_POINT ( 'NONE',  ( -21.97225858583376734, 4.201001019271233261, 2.140550196716301201 ) ) ;
#10386 = ORIENTED_EDGE ( 'NONE', *, *, #14468, .T. ) ;
#10385 = CARTESIAN_POINT ( 'NONE',  ( 69.01493751667922538, -5.004537671629235795, -4.043901188646982447 ) ) ;
#10387 = ORIENTED_EDGE ( 'NONE', *, *, #3641, .T. ) ;
#10388 = EDGE_CURVE ( 'NONE', #6959, #4832, #21320, .T. ) ;
#10389 = EDGE_CURVE ( 'NONE', #9572, #3790, #8829, .T. ) ;
#10390 = CARTESIAN_POINT ( 'NONE',  ( 43.74661801760413482, -24.08792321988613594, 1.500000000000000000 ) ) ;
#10391 = CARTESIAN_POINT ( 'NONE',  ( -8.000050800000018114, 1.979734913925816908, -2.936190332390367086 ) ) ;
#10392 = DIRECTION ( 'NONE',  ( -8.541412920197221047E-17, -0.9961946980917455452, -0.08715574274765869323 ) ) ;
#10393 = CARTESIAN_POINT ( 'NONE',  ( 3.249999999999999556, 0.000000000000000000, 0.000000000000000000 ) ) ;
#10395 = EDGE_LOOP ( 'NONE', ( #7032, #31118, #3347, #12766, #4192 ) ) ;
#10394 = CARTESIAN_POINT ( 'NONE',  ( 0.000000000000000000, 0.000000000000000000, 0.000000000000000000 ) ) ;
#10396 = LINE ( 'NONE', #26096, #16679 ) ;
#10397 = DIRECTION ( 'NONE',  ( -0.000000000000000000, -0.000000000000000000, -1.000000000000000000 ) ) ;
#10398 = CARTESIAN_POINT ( 'NONE',  ( 3.379077383500962650, -17.49391738930246376, 1.500000000000001332 ) ) ;
#10399 = CARTESIAN_POINT ( 'NONE',  ( 21.36000000136559507, -1.570731468192933633, -2.892927487894330074 ) ) ;
#10400 = EDGE_CURVE ( 'NONE', #21228, #26019, #6308, .T. ) ;
#10402 = ORIENTED_EDGE ( 'NONE', *, *, #17436, .T. ) ;
#10401 = CARTESIAN_POINT ( 'NONE',  ( 18.86054332783663767, -4.736068442360261699, 3.993434336035624366 ) ) ;
#10403 = CARTESIAN_POINT ( 'NONE',  ( 0.7632845268458192667, 3.174628368984171889, -8.152713396062660323 ) ) ;
#10404 = CARTESIAN_POINT ( 'NONE',  ( -23.54713438637982748, 18.46223496596754288, 1.773004750130224627 ) ) ;
#10405 = CARTESIAN_POINT ( 'NONE',  ( 21.23500000136559507, -1.570731468192933633, -2.892927487894330074 ) ) ;
#10406 = LINE ( 'NONE', #7891, #30034 ) ;
#10407 = ADVANCED_FACE ( 'NONE', ( #19035 ), #29379, .T. ) ;
#10408 = CARTESIAN_POINT ( 'NONE',  ( 5.489343555808772201, 8.118190043691528857, -0.1039150536218743925 ) ) ;
#10409 = LINE ( 'NONE', #20619, #167 ) ;
#10410 = AXIS2_PLACEMENT_3D ( 'NONE', #18922, #4035, #32116 ) ;
#10411 = VERTEX_POINT ( 'NONE', #16495 ) ;
#10412 = CARTESIAN_POINT ( 'NONE',  ( -2.093800801365593323, -0.3701630799359326152, 3.521866450007987037 ) ) ;
#10413 = CARTESIAN_POINT ( 'NONE',  ( 5.377543748152548098, -2.789499415801756586E-14, 8.014274990069656823 ) ) ;
#10414 = CARTESIAN_POINT ( 'NONE',  ( -2.437550801365593767, 3.675193018007246959, -1.088641768524161391 ) ) ;
#10415 = VERTEX_POINT ( 'NONE', #18688 ) ;
#10416 = DIRECTION ( 'NONE',  ( 1.000000000000000000, 0.000000000000000000, 0.000000000000000000 ) ) ;
#10417 = CARTESIAN_POINT ( 'NONE',  ( 10.55147673363119232, 4.116875700062115229, -2.376879293651021019 ) ) ;
#10418 = CARTESIAN_POINT ( 'NONE',  ( 56.97280603064898941, -277.2763395528616002, -4.621439243524461560 ) ) ;
#10419 = CYLINDRICAL_SURFACE ( 'NONE', #24616, 0.4999999999999995559 ) ;
#10420 = EDGE_LOOP ( 'NONE', ( #5043, #2563, #7260, #23170 ) ) ;
#10421 = CARTESIAN_POINT ( 'NONE',  ( -40.38425638691331443, -12.81449853570765995, 5.500000000000000888 ) ) ;
#10422 = ORIENTED_EDGE ( 'NONE', *, *, #23022, .T. ) ;
#10423 = CARTESIAN_POINT ( 'NONE',  ( -2.626726202933858723, 0.09953226261353739779, 1.366272513173315772 ) ) ;
#10425 = VERTEX_POINT ( 'NONE', #23873 ) ;
#10424 = CARTESIAN_POINT ( 'NONE',  ( -2.994539215707400892, -0.08249776133298661329, 1.285182061456009439 ) ) ;
#10426 = VERTEX_POINT ( 'NONE', #981 ) ;
#10427 = CARTESIAN_POINT ( 'NONE',  ( 108.8978791464556508, 17.52043075494136204, -4.999054092451819642 ) ) ;
#10428 = EDGE_CURVE ( 'NONE', #32816, #16296, #6655, .T. ) ;
#10429 = EDGE_CURVE ( 'NONE', #8252, #5204, #16191, .T. ) ;
#10430 = ORIENTED_EDGE ( 'NONE', *, *, #9363, .F. ) ;
#10431 = CARTESIAN_POINT ( 'NONE',  ( -10.00000000000000000, 0.000000000000000000, 0.000000000000000000 ) ) ;
#10433 = VERTEX_POINT ( 'NONE', #26414 ) ;
#10432 = CARTESIAN_POINT ( 'NONE',  ( 3.499999999999999556, 2.871924938129881699, 6.435996203144517480 ) ) ;
#10434 = FACE_OUTER_BOUND ( 'NONE', #29046, .T. ) ;
#10435 = CARTESIAN_POINT ( 'NONE',  ( -5.706376978575949721, -0.1572233378491221800, 3.000000000000000000 ) ) ;
#10436 = CARTESIAN_POINT ( 'NONE',  ( 7.249760686538667009, -8.711672189281431500, 0.8180878109961559064 ) ) ;
#10437 = DIRECTION ( 'NONE',  ( -0.1027947991993878318, 0.9947025833170222153, 0.000000000000000000 ) ) ;
#10438 = DIRECTION ( 'NONE',  ( 0.000000000000000000, 0.000000000000000000, 1.000000000000000000 ) ) ;
#10439 = CARTESIAN_POINT ( 'NONE',  ( 107.9694961684101457, -17.63011453012341789, 4.008137637261066644 ) ) ;
#10440 = B_SPLINE_CURVE_WITH_KNOTS ( 'NONE', 3,
 ( #17419, #27616, #4717, #17566 ),
 .UNSPECIFIED., .F., .F.,
 ( 4, 4 ),
 ( 0.000000000000000000, 2.207496556392325519E-08 ),
 .UNSPECIFIED. ) ;
#10441 = LINE ( 'NONE', #15432, #7011 ) ;
#10442 = CARTESIAN_POINT ( 'NONE',  ( 6.705444383089634641, -13.33025968055571120, 1.499999999999998446 ) ) ;
#10443 = LINE ( 'NONE', #5754, #26415 ) ;
#10444 = EDGE_CURVE ( 'NONE', #21614, #8757, #31738, .T. ) ;
#10445 = CARTESIAN_POINT ( 'NONE',  ( -3.827997810768590359, -10.69410007036526267, 0.9788672205877712029 ) ) ;
#10446 = CARTESIAN_POINT ( 'NONE',  ( 101.9216173105994159, -5.769792427975438898, -0.02339150517595088921 ) ) ;
#10447 = APPROVAL ( #15341, 'UNSPECIFIED' ) ;
#10448 = CYLINDRICAL_SURFACE ( 'NONE', #12935, 5.010000000000000675 ) ;
#10449 = CARTESIAN_POINT ( 'NONE',  ( 84.37491783462775174, -2.359815117480508651, 0.07017451552782423552 ) ) ;
#10450 = CARTESIAN_POINT ( 'NONE',  ( 102.6609843814833027, -1.982062027707616192, 4.522129901861162260 ) ) ;
#10451 = CARTESIAN_POINT ( 'NONE',  ( 12.62440642364078514, 21.58543435044974856, -1.499999999999994893 ) ) ;
#10452 = ORIENTED_EDGE ( 'NONE', *, *, #4648, .T. ) ;
#10453 = CARTESIAN_POINT ( 'NONE',  ( -6.887550801365593500, -2.752080473201636845, 2.228590825266444586 ) ) ;
#10454 = CARTESIAN_POINT ( 'NONE',  ( 23.22564588060105706, -21.93932300456764395, -1.010482809524661629 ) ) ;
#10455 = CARTESIAN_POINT ( 'NONE',  ( 108.6457025336241031, 16.11621187055573046, 2.334455007174216057 ) ) ;
#10456 = ORIENTED_EDGE ( 'NONE', *, *, #9626, .T. ) ;
#10457 = DIRECTION ( 'NONE',  ( 0.9896144216807900573, -1.102680533460266556E-16, 0.1437473352845034802 ) ) ;
#10458 =( LENGTH_UNIT ( ) NAMED_UNIT ( * ) SI_UNIT ( .MILLI., .METRE. ) );
#10459 = ADVANCED_FACE ( 'NONE', ( #3816 ), #12954, .F. ) ;
#10460 = EDGE_LOOP ( 'NONE', ( #26057, #21837, #22147, #11138 ) ) ;
#10461 = B_SPLINE_CURVE_WITH_KNOTS ( 'NONE', 3,
 ( #22073, #32289, #21728, #1669, #3855, #19404, #19560, #27228, #9350, #11378 ),
 .UNSPECIFIED., .F., .F.,
 ( 4, 2, 2, 2, 4 ),
 ( 2.571685856669747810E-07, 0.0005478592107668818533, 0.001095461252948096761, 0.001643063295129311560, 0.002190665337310527226 ),
 .UNSPECIFIED. ) ;
#10462 = CARTESIAN_POINT ( 'NONE',  ( 102.8769692529049564, -5.092190445904433815, -0.07017451552783644797 ) ) ;
#10463 = ITEM_DEFINED_TRANSFORMATION ( 'NONE', 'NONE', #1240,  #2865 ) ;
#10465 = EDGE_LOOP ( 'NONE', ( #23470, #2744, #6556, #31070, #17136 ) ) ;
#10464 = CARTESIAN_POINT ( 'NONE',  ( -2.819379691724114512, -6.927609664243465026, -4.522129901861166701 ) ) ;
#10466 = VERTEX_POINT ( 'NONE', #6162 ) ;
#10467 = CARTESIAN_POINT ( 'NONE',  ( 0.2100627325166786463, 10.28094456385920807, 2.172043487456292610 ) ) ;
#10468 = ORIENTED_EDGE ( 'NONE', *, *, #10004, .F. ) ;
#10469 =( BOUNDED_CURVE ( )  B_SPLINE_CURVE ( 3, ( #9835, #30086, #27394, #24878 ),
 .UNSPECIFIED., .F., .F. ) 
 B_SPLINE_CURVE_WITH_KNOTS ( ( 4, 4 ),
 ( 5.261730470397909976, 7.304640143961260712 ),
 .UNSPECIFIED. ) 
 CURVE ( )  GEOMETRIC_REPRESENTATION_ITEM ( )  RATIONAL_B_SPLINE_CURVE ( ( 1.000000000000000000, 0.6814171464877621931, 0.6814171464877621931, 1.000000000000000000 ) ) 
 REPRESENTATION_ITEM ( '' )  );
#10471 = ORIENTED_EDGE ( 'NONE', *, *, #8916, .F. ) ;
#10470 = DIRECTION ( 'NONE',  ( 3.623545766764135120E-17, 0.4226182617406906705, 0.9063077870366539335 ) ) ;
#10472 = CARTESIAN_POINT ( 'NONE',  ( 69.42401195566041849, -8.835509274224046194, 0.07017451552781803215 ) ) ;
#10473 = CARTESIAN_POINT ( 'NONE',  ( 108.0887845003129542, -19.34783683432074142, 2.566390659084664350 ) ) ;
#10474 = CARTESIAN_POINT ( 'NONE',  ( 0.000000000000000000, 0.000000000000000000, 0.000000000000000000 ) ) ;
#10475 = DIRECTION ( 'NONE',  ( 0.000000000000000000, 1.000000000000000000, -0.000000000000000000 ) ) ;
#10476 = ORIENTED_EDGE ( 'NONE', *, *, #19494, .F. ) ;
#10477 = CARTESIAN_POINT ( 'NONE',  ( 21.00111451137534146, -1.283275288181523244E-15, -2.499999999999998668 ) ) ;
#10478 = CARTESIAN_POINT ( 'NONE',  ( 7.577572045913244736, 15.00000000000000178, 4.629213727441584325 ) ) ;
#10479 = CARTESIAN_POINT ( 'NONE',  ( 55.01406067017561696, -7.826279391976612487, -1.873789188487492430 ) ) ;
#10480 = CARTESIAN_POINT ( 'NONE',  ( -10.00000000000000000, 0.000000000000000000, 0.000000000000000000 ) ) ;
#10481 = EDGE_CURVE ( 'NONE', #16163, #27055, #26887, .T. ) ;
#10482 = CARTESIAN_POINT ( 'NONE',  ( -8.000050800000003903, -2.165465766649708357, 2.111084521466020103 ) ) ;
#10483 = CARTESIAN_POINT ( 'NONE',  ( 7.249760686538666121, 0.000000000000000000, 6.000000000000000000 ) ) ;
#10484 = CARTESIAN_POINT ( 'NONE',  ( -1.082681991931092158, 0.000000000000000000, -4.612695725900422872 ) ) ;
#10485 = CARTESIAN_POINT ( 'NONE',  ( 6.356382477965130562, -6.947086032709898440, -5.080803740829792581 ) ) ;
#10486 = ORIENTED_EDGE ( 'NONE', *, *, #7732, .F. ) ;
#10487 = CARTESIAN_POINT ( 'NONE',  ( -7.762550801365593500, 2.228590825266444142, 2.752080473201636845 ) ) ;
#10488 = ORIENTED_EDGE ( 'NONE', *, *, #21878, .T. ) ;
#10489 = CARTESIAN_POINT ( 'NONE',  ( -4.504531657079157370, 0.3127741368606810068, -2.975847129947406522 ) ) ;
#10490 = DIRECTION ( 'NONE',  ( -0.000000000000000000, -0.000000000000000000, -1.000000000000000000 ) ) ;
#10491 = CARTESIAN_POINT ( 'NONE',  ( 0.8040887157109507521, -3.277015635683791395, 1.762426081327307825 ) ) ;
#10492 = CARTESIAN_POINT ( 'NONE',  ( 24.38441422956826088, -17.22282062799385116, 1.499999999999444222 ) ) ;
#10493 = VERTEX_POINT ( 'NONE', #19184 ) ;
#10494 = EDGE_CURVE ( 'NONE', #16352, #1604, #14935, .T. ) ;
#10495 = CYLINDRICAL_SURFACE ( 'NONE', #27885, 0.5000000000000002220 ) ;
#10496 = EDGE_CURVE ( 'NONE', #9056, #29074, #9192, .T. ) ;
#10497 = ORIENTED_EDGE ( 'NONE', *, *, #15933, .F. ) ;
#10498 = CARTESIAN_POINT ( 'NONE',  ( 1.635980141547796585, -1.437409680492520936, 1.758786303110331906 ) ) ;
#10499 = EDGE_CURVE ( 'NONE', #4248, #29383, #2316, .T. ) ;
#10500 = APPROVAL_ROLE ( '' ) ;
#10501 = CARTESIAN_POINT ( 'NONE',  ( 18.77000516020590482, -5.748103448524430448, 4.150065909458478863 ) ) ;
#10502 = FACE_OUTER_BOUND ( 'NONE', #13913, .T. ) ;
#10504 = DIRECTION ( 'NONE',  ( 0.000000000000000000, -0.000000000000000000, 1.000000000000000000 ) ) ;
#10503 = DIRECTION ( 'NONE',  ( -1.000000000000000000, -0.000000000000000000, -0.000000000000000000 ) ) ;
#10505 = VERTEX_POINT ( 'NONE', #20189 ) ;
#10506 = DIRECTION ( 'NONE',  ( 0.000000000000000000, 0.000000000000000000, 1.000000000000000000 ) ) ;
#10507 = CARTESIAN_POINT ( 'NONE',  ( -12.44989959798873791, -0.06979899340500209104, -12.99999999999999645 ) ) ;
#10508 = CARTESIAN_POINT ( 'NONE',  ( 21.86000000136559507, 1.570731468192929858, 2.892927487894329186 ) ) ;
#10509 = CARTESIAN_POINT ( 'NONE',  ( 19.76529769139576587, -16.89702959469647325, -1.499999999998181677 ) ) ;
#10511 = VERTEX_POINT ( 'NONE', #27196 ) ;
#10510 = DIRECTION ( 'NONE',  ( 1.000000000000000000, -0.000000000000000000, -0.000000000000000000 ) ) ;
#10512 = CARTESIAN_POINT ( 'NONE',  ( -6.762550801365593500, -2.752080473201636845, 2.228590825266444586 ) ) ;
#10513 = DIRECTION ( 'NONE',  ( 1.000000000000000000, -8.574039729943018344E-17, -0.000000000000000000 ) ) ;
#10514 = CARTESIAN_POINT ( 'NONE',  ( -15.12340757463330654, -28.43932300454936879, -1.500000000000000000 ) ) ;
#10515 = MANIFOLD_SOLID_BREP ( 'Chamfer1', #13479 ) ;
#10516 = ORIENTED_EDGE ( 'NONE', *, *, #28340, .T. ) ;
#10517 = ORIENTED_EDGE ( 'NONE', *, *, #5915, .F. ) ;
#10518 = CARTESIAN_POINT ( 'NONE',  ( 24.01922593961184305, -17.30645187339492352, -1.384626276794869604 ) ) ;
#10519 = CARTESIAN_POINT ( 'NONE',  ( 0.000000000000000000, 8.475820894092974456, 4.057423117305423155 ) ) ;
#10520 = CARTESIAN_POINT ( 'NONE',  ( 22.23500000136559507, -3.156283516753370488, -0.9349337715887220401 ) ) ;
#10521 = CARTESIAN_POINT ( 'NONE',  ( 0.7212197624752669789, 2.263408446298215360, 8.661246924783316814 ) ) ;
#10522 = LINE ( 'NONE', #10860, #3912 ) ;
#10523 = CARTESIAN_POINT ( 'NONE',  ( 84.85832005755364094, -2.331047133796893878, 0.07017451552782270896 ) ) ;
#10524 = CARTESIAN_POINT ( 'NONE',  ( 18.60860417056574079, -7.552242585353607929, 0.8105616806061413104 ) ) ;
#10525 = VERTEX_POINT ( 'NONE', #17659 ) ;
#10526 = EDGE_CURVE ( 'NONE', #14136, #30361, #26811, .T. ) ;
#10527 = CARTESIAN_POINT ( 'NONE',  ( -31.57659242536668742, -27.93932300454937590, -0.9999999999999997780 ) ) ;
#10528 = EDGE_CURVE ( 'NONE', #3046, #25477, #22037, .T. ) ;
#10529 = EDGE_CURVE ( 'NONE', #24619, #19255, #15633, .T. ) ;
#10530 = PERSON_AND_ORGANIZATION_ROLE ( 'classification_officer' ) ;
#10531 = DIRECTION ( 'NONE',  ( 0.000000000000000000, -0.2588190451025207950, -0.9659258262890683122 ) ) ;
#10532 = ORIENTED_EDGE ( 'NONE', *, *, #31449, .F. ) ;
#10533 = DIRECTION ( 'NONE',  ( 0.000000000000000000, 0.9059606027152153906, 0.4233620038783403872 ) ) ;
#10534 = ORIENTED_EDGE ( 'NONE', *, *, #12845, .T. ) ;
#10535 = CARTESIAN_POINT ( 'NONE',  ( -5.150050802731186650, 2.983565686104819648, 0.3135853898029609677 ) ) ;
#10537 = ORIENTED_EDGE ( 'NONE', *, *, #20840, .F. ) ;
#10536 = CARTESIAN_POINT ( 'NONE',  ( 18.82056267271510208, -5.182971926406968244, -4.312042181581901445 ) ) ;
#10538 = VERTEX_POINT ( 'NONE', #24698 ) ;
#10539 = CARTESIAN_POINT ( 'NONE',  ( -2.253815017383503871, -0.3178988483021043532, 3.024605502323848061 ) ) ;
#10540 = CARTESIAN_POINT ( 'NONE',  ( -6.612550801365594033, -3.368539882008727115, -1.828967928396027842 ) ) ;
#10541 = DIRECTION ( 'NONE',  ( 0.000000000000000000, 0.000000000000000000, -1.000000000000000000 ) ) ;
#10542 = DIRECTION ( 'NONE',  ( -1.000000000000000000, 0.000000000000000000, 0.000000000000000000 ) ) ;
#10544 = VERTEX_POINT ( 'NONE', #14484 ) ;
#10543 = FACE_OUTER_BOUND ( 'NONE', #21791, .T. ) ;
#10545 = CARTESIAN_POINT ( 'NONE',  ( 9.149098621172166546, 18.06225657836807841, 4.629213727441584325 ) ) ;
#10546 = CARTESIAN_POINT ( 'NONE',  ( 23.81497248412561873, 17.93793532016357517, 1.050000000000000044 ) ) ;
#10547 = CARTESIAN_POINT ( 'NONE',  ( -4.548081766001798698, -6.140004230154746168, 1.499999999999999556 ) ) ;
#10548 = CARTESIAN_POINT ( 'NONE',  ( 25.48500000136559862, 2.892927487894327410, -1.570731468192931635 ) ) ;
#10549 = FACE_OUTER_BOUND ( 'NONE', #1958, .T. ) ;
#10551 = ORIENTED_EDGE ( 'NONE', *, *, #7313, .F. ) ;
#10550 = CARTESIAN_POINT ( 'NONE',  ( 22.00639167669224960, -21.80013755708282730, -1.499999999999999556 ) ) ;
#10552 = CARTESIAN_POINT ( 'NONE',  ( 10.00000000000000178, 0.6226916219172025091, 4.971152295393305387 ) ) ;
#10553 = ADVANCED_FACE ( 'NONE', ( #27867 ), #31112, .T. ) ;
#10554 = CARTESIAN_POINT ( 'NONE',  ( -29.56299279204132091, 14.30956982362833152, 1.874474774381077458 ) ) ;
#10555 = CARTESIAN_POINT ( 'NONE',  ( 21.61000000136559507, 3.156283516753366047, 0.9349337715887203748 ) ) ;
#10556 = CARTESIAN_POINT ( 'NONE',  ( -8.000050800000002127, 0.2098993114761400491, -2.993269680925520149 ) ) ;
#10557 = CARTESIAN_POINT ( 'NONE',  ( 3.499999999999999556, -4.147285340411747789, -5.698247474649445365 ) ) ;
#10558 = CARTESIAN_POINT ( 'NONE',  ( 5.533288710217197703, 0.000000000000000000, 5.777777777777793666 ) ) ;
#10559 = EDGE_CURVE ( 'NONE', #8809, #26222, #28110, .T. ) ;
#10560 = EDGE_LOOP ( 'NONE', ( #8216, #10064, #14982, #16908 ) ) ;
#10561 = DIRECTION ( 'NONE',  ( -1.000000000000000000, 0.000000000000000000, 0.000000000000000000 ) ) ;
#10562 = EDGE_CURVE ( 'NONE', #26729, #23098, #17171, .T. ) ;
#10563 = MANIFOLD_SOLID_BREP ( 'Revolve1', #5637 ) ;
#10564 = DIRECTION ( 'NONE',  ( 0.000000000000000000, 0.9945218953682729568, 0.1045284632676570374 ) ) ;
#10565 = EDGE_CURVE ( 'NONE', #5075, #21400, #15169, .T. ) ;
#10566 = EDGE_LOOP ( 'NONE', ( #13137, #13100, #377, #13180 ) ) ;
#10567 = FACE_OUTER_BOUND ( 'NONE', #11958, .T. ) ;
#10568 = CARTESIAN_POINT ( 'NONE',  ( 6.524595395369781947, -8.328507089302162214, -2.369138865965912721 ) ) ;
#10569 = EDGE_CURVE ( 'NONE', #24800, #15472, #9728, .T. ) ;
#10570 = DIRECTION ( 'NONE',  ( -1.000000000000000000, -0.000000000000000000, 0.000000000000000000 ) ) ;
#10572 = CARTESIAN_POINT ( 'NONE',  ( 107.9869154117469492, -17.88094730081049377, 4.507188101940097447 ) ) ;
#10571 = DIRECTION ( 'NONE',  ( -0.9960221812693187404, 0.08910563629484180570, 0.000000000000000000 ) ) ;
#10573 = ORIENTED_EDGE ( 'NONE', *, *, #1440, .T. ) ;
#10574 = CARTESIAN_POINT ( 'NONE',  ( -40.91822763088380555, -13.69660594212654914, 5.550376981476465410 ) ) ;
#10575 = ORIENTED_EDGE ( 'NONE', *, *, #8751, .T. ) ;
#10576 = CARTESIAN_POINT ( 'NONE',  ( 34.99744630603539974, 0.5000000000000000000, -2.982419344532999617 ) ) ;
#10578 = ORIENTED_EDGE ( 'NONE', *, *, #9690, .F. ) ;
#10577 = CARTESIAN_POINT ( 'NONE',  ( 108.3631332966649410, 20.50195487734757904, -1.437511512156359972 ) ) ;
#10579 = EDGE_CURVE ( 'NONE', #11907, #14398, #10940, .T. ) ;
#10580 = ORIENTED_EDGE ( 'NONE', *, *, #7674, .F. ) ;
#10581 = CARTESIAN_POINT ( 'NONE',  ( 5.489344046532321997, -4.149088721182480732, -6.978601450725530064 ) ) ;
#10582 = EDGE_CURVE ( 'NONE', #12204, #25155, #6549, .T. ) ;
#10583 = CARTESIAN_POINT ( 'NONE',  ( 10.00000000000000000, -3.024842911000719781, 3.993798362933299373 ) ) ;
#10585 = VERTEX_POINT ( 'NONE', #2482 ) ;
#10584 = CARTESIAN_POINT ( 'NONE',  ( 21.34939358370770535, -21.78237682584225254, 1.377397332511454353 ) ) ;
#10586 = CARTESIAN_POINT ( 'NONE',  ( 10.55147673363118876, -2.376879293651094294, 4.116875700062075261 ) ) ;
#10587 = CARTESIAN_POINT ( 'NONE',  ( 1.853623169654749159, -10.69666880112111684, -1.762806831122527118 ) ) ;
#10588 = DIRECTION ( 'NONE',  ( 0.000000000000000000, 0.000000000000000000, 1.000000000000000000 ) ) ;
#10589 = CARTESIAN_POINT ( 'NONE',  ( 25.46419143545908526, -18.07592536767254643, -1.500000000000000000 ) ) ;
#10590 = LINE ( 'NONE', #7151, #22953 ) ;
#10591 = CARTESIAN_POINT ( 'NONE',  ( 107.9730816776244069, -17.68174497084636343, 4.113993602947243033 ) ) ;
#10592 = EDGE_CURVE ( 'NONE', #481, #11524, #17851, .T. ) ;
#10593 = EDGE_CURVE ( 'NONE', #6331, #18408, #10891, .T. ) ;
#10594 = CARTESIAN_POINT ( 'NONE',  ( 0.000000000000000000, 0.000000000000000000, 0.000000000000000000 ) ) ;
#10595 = DIRECTION ( 'NONE',  ( 1.000000000000000000, 0.000000000000000000, 0.000000000000000000 ) ) ;
#10596 = DIRECTION ( 'NONE',  ( -0.000000000000000000, 0.000000000000000000, 1.000000000000000000 ) ) ;
#10597 = DIRECTION ( 'NONE',  ( -1.000000000000000000, 0.000000000000000000, 0.000000000000000000 ) ) ;
#10598 = CARTESIAN_POINT ( 'NONE',  ( 0.000000000000000000, -9.241976615262169403, 1.699438267350338982 ) ) ;
#10599 = ORIENTED_EDGE ( 'NONE', *, *, #9855, .F. ) ;
#10600 = LINE ( 'NONE', #8277, #19897 ) ;
#10601 = EDGE_CURVE ( 'NONE', #28083, #8736, #25527, .T. ) ;
#10602 = CARTESIAN_POINT ( 'NONE',  ( 48.01729800609908949, -4.703650321867185902, 4.522129901861162260 ) ) ;
#10603 = ADVANCED_FACE ( 'NONE', ( #8137 ), #13295, .F. ) ;
#10604 = DIRECTION ( 'NONE',  ( 0.000000000000000000, 0.000000000000000000, 1.000000000000000000 ) ) ;
#10605 = ORIENTED_EDGE ( 'NONE', *, *, #1838, .F. ) ;
#10606 = CARTESIAN_POINT ( 'NONE',  ( 25.47393414918137466, -2.112935325431762656, -1.751578099123880516 ) ) ;
#10607 = DIRECTION ( 'NONE',  ( -0.000000000000000000, -0.000000000000000000, -1.000000000000000000 ) ) ;
#10608 = ORIENTED_EDGE ( 'NONE', *, *, #28224, .F. ) ;
#10609 = DIRECTION ( 'NONE',  ( 0.000000000000000000, 0.000000000000000000, 1.000000000000000000 ) ) ;
#10610 =( NAMED_UNIT ( * ) PLANE_ANGLE_UNIT ( ) SI_UNIT ( $, .RADIAN. ) );
#10611 = EDGE_CURVE ( 'NONE', #31289, #6686, #29277, .T. ) ;
#10612 = ORIENTED_EDGE ( 'NONE', *, *, #14125, .T. ) ;
#10613 = CARTESIAN_POINT ( 'NONE',  ( 102.5484925806840835, -0.3622080806379225915, -1.915219082070890755 ) ) ;
#10614 = PERSON_AND_ORGANIZATION_ROLE ( 'classification_officer' ) ;
#10616 = ORIENTED_EDGE ( 'NONE', *, *, #14125, .F. ) ;
#10615 = DIRECTION ( 'NONE',  ( 0.000000000000000000, -0.7431448254773863615, -0.6691306063588670083 ) ) ;
#10617 = VERTEX_POINT ( 'NONE', #1432 ) ;
#10618 = DIRECTION ( 'NONE',  ( 2.498001805406600196E-13, 1.000000000000000000, 0.000000000000000000 ) ) ;
#10619 = EDGE_CURVE ( 'NONE', #21890, #15271, #22026, .T. ) ;
#10620 = ORIENTED_EDGE ( 'NONE', *, *, #13337, .T. ) ;
#10621 = APPROVAL ( #3936, 'UNKNOWN' ) ;
#10622 = CARTESIAN_POINT ( 'NONE',  ( -53.35155202832373078, 4.402097243136370963, 5.500000000000000000 ) ) ;
#10624 = ORIENTED_EDGE ( 'NONE', *, *, #3504, .T. ) ;
#10623 = CARTESIAN_POINT ( 'NONE',  ( -2.715578077270538682, -0.5452878916197804182, 1.748464050160077887 ) ) ;
#10625 = CARTESIAN_POINT ( 'NONE',  ( -15.09999999999999609, -27.93932300454937590, 1.500000000000000000 ) ) ;
#10626 = CARTESIAN_POINT ( 'NONE',  ( 108.1216519843055295, -19.82112042741262670, 1.596396689095263222 ) ) ;
#10627 = DIRECTION ( 'NONE',  ( 1.000000000000000000, 0.000000000000000000, 0.000000000000000000 ) ) ;
#10628 = DIRECTION ( 'NONE',  ( 0.000000000000000000, 0.000000000000000000, -1.000000000000000000 ) ) ;
#10629 = EDGE_LOOP ( 'NONE', ( #26560, #11116, #13099, #4469 ) ) ;
#10630 = CARTESIAN_POINT ( 'NONE',  ( 0.000000000000000000, -4.724769925181146135, -4.089810527897805414 ) ) ;
#10631 = CARTESIAN_POINT ( 'NONE',  ( -1.047937531484008700, -4.989690239014953121, -4.522129901861164925 ) ) ;
#10632 = CARTESIAN_POINT ( 'NONE',  ( 69.13676591393821980, -7.435400085125419167, -1.873789664671283051 ) ) ;
#10633 = DIRECTION ( 'NONE',  ( 0.000000000000000000, 0.000000000000000000, 1.000000000000000000 ) ) ;
#10634 = EDGE_CURVE ( 'NONE', #3548, #24916, #1747, .T. ) ;
#10635 = CARTESIAN_POINT ( 'NONE',  ( 7.249760686538667009, 5.151476664237558900, -6.139290821770204687 ) ) ;
#10636 = CARTESIAN_POINT ( 'NONE',  ( -7.362942409646514363, 1.214281993118000652E-15, 3.000000000000000000 ) ) ;
#10637 = DIRECTION ( 'NONE',  ( -1.000000000000000000, 0.000000000000000000, 0.000000000000000000 ) ) ;
#10638 = CARTESIAN_POINT ( 'NONE',  ( 6.524595623740803596, -7.015943501182358766, -5.074779492939359926 ) ) ;
#10639 = EDGE_CURVE ( 'NONE', #17664, #14956, #22554, .T. ) ;
#10640 = CARTESIAN_POINT ( 'NONE',  ( -3.162550801365593856, 2.752080473201636845, -2.228590825266444142 ) ) ;
#10641 = EDGE_LOOP ( 'NONE', ( #9963, #13060, #13964 ) ) ;
#10642 = CARTESIAN_POINT ( 'NONE',  ( -8.450050800000001416, 1.549418761218566143, -2.853674364686379583 ) ) ;
#10643 = CARTESIAN_POINT ( 'NONE',  ( 108.0492188137333471, 18.45222970056496692, 4.641158654489260904 ) ) ;
#10644 = DIRECTION ( 'NONE',  ( 1.000000000000000000, 0.000000000000000000, 0.000000000000000000 ) ) ;
#10645 = CARTESIAN_POINT ( 'NONE',  ( 9.555580689063649658, -12.32072190999856431, 1.500000000000000000 ) ) ;
#10646 = VERTEX_POINT ( 'NONE', #9083 ) ;
#10647 = DIRECTION ( 'NONE',  ( 0.000000000000000000, 0.000000000000000000, 1.000000000000000000 ) ) ;
#10648 = AXIS2_PLACEMENT_3D ( 'NONE', #16803, #19642, #25136 ) ;
#10649 =( BOUNDED_CURVE ( )  B_SPLINE_CURVE ( 2, ( #24367, #24704, #4501, #12160, #16682, #8979, #14489, #19190, #12014, #22358, #29385 ),
 .UNSPECIFIED., .F., .F. ) 
 B_SPLINE_CURVE_WITH_KNOTS ( ( 3, 2, 2, 2, 2, 3 ),
 ( 0.8966116191895003862, 0.9000000000000000222, 0.9250000000000000444, 0.9499999999999999556, 0.9749999999999999778, 0.9966116191895003640 ),
 .UNSPECIFIED. ) 
 CURVE ( )  GEOMETRIC_REPRESENTATION_ITEM ( )  RATIONAL_B_SPLINE_CURVE ( ( 0.9821626249036858880, 0.9896829947469992783, 1.000000000000000000, 0.9238795325112867385, 1.000000000000000000, 0.9238795325112867385, 1.000000000000000000, 0.9238795325112867385, 1.000000000000000000, 0.9341965377642874602, 0.9821626249036858880 ) ) 
 REPRESENTATION_ITEM ( '' )  );
#10650 = VERTEX_POINT ( 'NONE', #29022 ) ;
#10651 = DIRECTION ( 'NONE',  ( 0.4922101374339195035, 0.7179542890850474368, -0.4922101374328513579 ) ) ;
#10652 = PERSON_AND_ORGANIZATION_ROLE ( 'classification_officer' ) ;
#10653 = CARTESIAN_POINT ( 'NONE',  ( 102.4142005201414918, -3.868549851786822646, 4.150065902002959106 ) ) ;
#10654 = EDGE_CURVE ( 'NONE', #19087, #25039, #27897, .T. ) ;
#10655 = CARTESIAN_POINT ( 'NONE',  ( -56.32779077071818818, 0.3678964383417479556, -1.500000000000000000 ) ) ;
#10657 = CARTESIAN_POINT ( 'NONE',  ( 7.064423669210277978, 7.135485519863459913, 5.064320921489716909 ) ) ;
#10656 = CARTESIAN_POINT ( 'NONE',  ( 3.063284526839887167, 0.000000000000000000, 0.000000000000000000 ) ) ;
#10658 = ORIENTED_EDGE ( 'NONE', *, *, #10619, .F. ) ;
#10659 = DIRECTION ( 'NONE',  ( -1.224646799147353207E-16, 1.000000000000000000, 0.000000000000000000 ) ) ;
#10660 = DIRECTION ( 'NONE',  ( 7.023442172597802627E-17, 0.8191520442889853593, 0.5735764363510552633 ) ) ;
#10661 = CARTESIAN_POINT ( 'NONE',  ( 21.42250000136559507, -0.3178988483021076838, -3.024605502323848949 ) ) ;
#10662 = AXIS2_PLACEMENT_3D ( 'NONE', #27671, #4774, #17326 ) ;
#10664 = ORIENTED_EDGE ( 'NONE', *, *, #26540, .F. ) ;
#10663 = CARTESIAN_POINT ( 'NONE',  ( 9.302055952181039089, 0.2457637073014079521, -1.050000000000000044 ) ) ;
#10665 = CARTESIAN_POINT ( 'NONE',  ( -6.012550801365594388, -1.828967928396026510, 3.368539882008728004 ) ) ;
#10666 = AXIS2_PLACEMENT_3D ( 'NONE', #6542, #26946, #4049 ) ;
#10667 = PLANE ( 'NONE',  #23600 ) ;
#10668 = CARTESIAN_POINT ( 'NONE',  ( 102.5016417986325621, -5.123484090859097506, -2.184956770182200358 ) ) ;
#10669 = ORIENTED_EDGE ( 'NONE', *, *, #22134, .F. ) ;
#10670 = ORIENTED_EDGE ( 'NONE', *, *, #16290, .F. ) ;
#10671 = ADVANCED_FACE ( 'NONE', ( #8444 ), #31519, .F. ) ;
#10672 = DIRECTION ( 'NONE',  ( 0.000000000000000000, 0.000000000000000000, 1.000000000000000000 ) ) ;
#10673 = DIRECTION ( 'NONE',  ( 1.000000000000000000, -8.574039729943018344E-17, -0.000000000000000000 ) ) ;
#10674 = EDGE_CURVE ( 'NONE', #26855, #7281, #24937, .T. ) ;
#10675 = CARTESIAN_POINT ( 'NONE',  ( 102.6609843814833027, -1.982062027707616192, 4.522129901861162260 ) ) ;
#10676 = DIRECTION ( 'NONE',  ( 0.000000000000000000, 0.000000000000000000, -1.000000000000000000 ) ) ;
#10677 = CARTESIAN_POINT ( 'NONE',  ( 3.249999999999999556, -0.4999240074895051067, 8.734705317681624948 ) ) ;
#10678 = CARTESIAN_POINT ( 'NONE',  ( 3.499999999999999556, 4.561279057474412646, 4.271385531633187682 ) ) ;
#10679 = CARTESIAN_POINT ( 'NONE',  ( 23.61221640758335027, -8.051464822112823327, 0.07017451552782230650 ) ) ;
#10680 = EDGE_LOOP ( 'NONE', ( #24234, #19478, #31386, #3456, #14260, #4657, #12170 ) ) ;
#10681 = CARTESIAN_POINT ( 'NONE',  ( 5.885541736258995904, -2.519172009311986926, 8.006759975090643522 ) ) ;
#10682 = AXIS2_PLACEMENT_3D ( 'NONE', #17022, #4343, #14523 ) ;
#10683 = AXIS2_PLACEMENT_3D ( 'NONE', #4247, #16612, #16950 ) ;
#10684 = ORIENTED_EDGE ( 'NONE', *, *, #17139, .F. ) ;
#10685 = PERSON_AND_ORGANIZATION ( #6766, #25292 ) ;
#10686 = CARTESIAN_POINT ( 'NONE',  ( 48.01729800609908949, -4.703650321870253670, 4.522129901861162260 ) ) ;
#10687 = ORIENTED_EDGE ( 'NONE', *, *, #16827, .T. ) ;
#10688 = TOROIDAL_SURFACE ( 'NONE', #19798, 8.000000000000000000, 0.5000000000000000000 ) ;
#10689 = CARTESIAN_POINT ( 'NONE',  ( 10.93412304894858167, -12.62793677521797164, -0.9999999999999997780 ) ) ;
#10690 = ORIENTED_EDGE ( 'NONE', *, *, #2729, .F. ) ;
#10691 = DIRECTION ( 'NONE',  ( 0.06927878976713386372, -0.9975973382524639943, 0.000000000000000000 ) ) ;
#10693 = ORIENTED_EDGE ( 'NONE', *, *, #17803, .F. ) ;
#10692 = CARTESIAN_POINT ( 'NONE',  ( 102.3491787549029510, -2.929927866010495041, -4.093303780340187714 ) ) ;
#10694 = VERTEX_POINT ( 'NONE', #16300 ) ;
#10695 = DIRECTION ( 'NONE',  ( 1.000000000000000000, -0.000000000000000000, -0.000000000000000000 ) ) ;
#10696 = CARTESIAN_POINT ( 'NONE',  ( 56.97280603064898941, -277.2763395528616002, 1.508259000770581615 ) ) ;
#10697 = CARTESIAN_POINT ( 'NONE',  ( 11.20269353100556486, -13.34333142745244238, 1.499999999999999778 ) ) ;
#10698 = LINE ( 'NONE', #7537, #5971 ) ;
#10700 = ORIENTED_EDGE ( 'NONE', *, *, #28548, .T. ) ;
#10699 = DIRECTION ( 'NONE',  ( -0.1908089953765453595, 1.324003374828971999E-15, -0.9816271834476638647 ) ) ;
#10701 = CARTESIAN_POINT ( 'NONE',  ( 7.249760686538667009, -1.391664247347281780, 7.892520144992429820 ) ) ;
#10702 = CARTESIAN_POINT ( 'NONE',  ( 17.56297300348760615, 13.04222886887431798, 1.050000000000000044 ) ) ;
#10703 = AXIS2_PLACEMENT_3D ( 'NONE', #12719, #221, #32823 ) ;
#10704 = CARTESIAN_POINT ( 'NONE',  ( -4.125289193777756935, -7.575181221222853090, 1.744514882266629874 ) ) ;
#10705 = CARTESIAN_POINT ( 'NONE',  ( 21.11000000136559152, -3.156283516753370044, -0.9349337715887220401 ) ) ;
#10706 = AXIS2_PLACEMENT_3D ( 'NONE', #28391, #8642, #5809 ) ;
#10707 = DIRECTION ( 'NONE',  ( 0.000000000000000000, 1.000000000000000000, 0.000000000000000000 ) ) ;
#10708 = EDGE_CURVE ( 'NONE', #280, #13240, #21313, .T. ) ;
#10710 = ORIENTED_EDGE ( 'NONE', *, *, #29647, .F. ) ;
#10709 = CARTESIAN_POINT ( 'NONE',  ( 10.57125986779756843, -0.8254815157534942660, -4.681538312723525053 ) ) ;
#10711 = DIRECTION ( 'NONE',  ( -1.000000000000000000, 8.574039729943018344E-17, -0.000000000000000000 ) ) ;
#10712 = ADVANCED_FACE ( 'NONE', ( #13928 ), #16131, .T. ) ;
#10713 = AXIS2_PLACEMENT_3D ( 'NONE', #3580, #18461, #8749 ) ;
#10714 = VECTOR ( 'NONE', #10746, 1000.000000000000227 ) ;
#10715 = DIRECTION ( 'NONE',  ( 1.000000000000000000, 0.000000000000000000, 0.000000000000000000 ) ) ;
#10716 = CARTESIAN_POINT ( 'NONE',  ( 24.86000000273118715, -1.942864903642428587, -1.573300977624592756 ) ) ;
#10717 = DIRECTION ( 'NONE',  ( 0.000000000000000000, 0.000000000000000000, 1.000000000000000000 ) ) ;
#10718 = CARTESIAN_POINT ( 'NONE',  ( -4.512942406915326998, 4.884725290497410777E-15, -2.999999999999999556 ) ) ;
#10719 = DIRECTION ( 'NONE',  ( 0.4999999999999977796, 0.8660254037844398178, 0.000000000000000000 ) ) ;
#10720 = VECTOR ( 'NONE', #5835, 1000.000000000000000 ) ;
#10721 = DIRECTION ( 'NONE',  ( -3.552713678800500929E-15, 0.000000000000000000, 1.000000000000000000 ) ) ;
#10722 = DIRECTION ( 'NONE',  ( -7.472768010111999110E-18, -0.08715574274766814400, 0.9961946980917446570 ) ) ;
#10723 = VERTEX_POINT ( 'NONE', #18820 ) ;
#10724 = ADVANCED_BREP_SHAPE_REPRESENTATION ( '', ( #10515, #2865 ), #32200 ) ;
#10725 = CARTESIAN_POINT ( 'NONE',  ( 25.23500000000000654, 2.486304733690583912, -0.2613212031729839624 ) ) ;
#10726 = AXIS2_PLACEMENT_3D ( 'NONE', #30708, #18300, #17971 ) ;
#10727 = CARTESIAN_POINT ( 'NONE',  ( -0.9801757370192284435, 19.50000000000000000, 6.747923662139668544 ) ) ;
#10728 = VECTOR ( 'NONE', #21238, 1000.000000000000000 ) ;
#10729 = CARTESIAN_POINT ( 'NONE',  ( 0.3277201397524639459, -5.271209332775584677, -1.500000000000000444 ) ) ;
#10731 = CARTESIAN_POINT ( 'NONE',  ( 107.5501414772658961, -18.81481929958330568, 4.827012719627553849 ) ) ;
#10730 = CARTESIAN_POINT ( 'NONE',  ( 108.0493349993913341, 18.45287666815344352, -4.631887712010465563 ) ) ;
#10732 = ORIENTED_EDGE ( 'NONE', *, *, #9210, .T. ) ;
#10733 = AXIS2_PLACEMENT_3D ( 'NONE', #26228, #26416, #3343 ) ;
#10734 = VECTOR ( 'NONE', #13326, 1000.000000000000114 ) ;
#10735 = CARTESIAN_POINT ( 'NONE',  ( -31.67864539881508179, -25.93932300454937945, 1.095404497688271528 ) ) ;
#10736 = CIRCLE ( 'NONE', #32084, 5.010000000000000675 ) ;
#10737 = ORIENTED_EDGE ( 'NONE', *, *, #9189, .F. ) ;
#10738 = CARTESIAN_POINT ( 'NONE',  ( -2.760161469795538558, -0.06813755667566065433, 1.269913365998487365 ) ) ;
#10740 = ORIENTED_EDGE ( 'NONE', *, *, #9189, .T. ) ;
#10739 = CARTESIAN_POINT ( 'NONE',  ( -30.51827900900859802, 4.402097243136377180, 5.049999999999999822 ) ) ;
#10741 = VERTEX_POINT ( 'NONE', #26358 ) ;
#10742 = DIRECTION ( 'NONE',  ( 8.574039729943018344E-17, 1.000000000000000000, 0.000000000000000000 ) ) ;
#10744 = VECTOR ( 'NONE', #1081, 1000.000000000000000 ) ;
#10743 = CARTESIAN_POINT ( 'NONE',  ( 101.6022419886208610, -1.170867242066747416, 0.07017451552782490165 ) ) ;
#10745 = EDGE_CURVE ( 'NONE', #12480, #1608, #4948, .T. ) ;
#10747 = ORIENTED_EDGE ( 'NONE', *, *, #22622, .F. ) ;
#10746 = DIRECTION ( 'NONE',  ( 0.9896144216807899463, -8.678901113238559347E-19, 0.1437473352845035635 ) ) ;
#10748 = VERTEX_POINT ( 'NONE', #21803 ) ;
#10749 = DIRECTION ( 'NONE',  ( 0.000000000000000000, -0.9059606027152153906, 0.4233620038783403872 ) ) ;
#10750 = LINE ( 'NONE', #5419, #29985 ) ;
#10751 = CARTESIAN_POINT ( 'NONE',  ( 24.24156412053827836, -17.70199322286653043, -1.500000000000000000 ) ) ;
#10752 = LINE ( 'NONE', #13408, #21925 ) ;
#10753 = CARTESIAN_POINT ( 'NONE',  ( 107.9552175441146176, -17.42450589234269387, 3.586585920852337406 ) ) ;
#10754 = AXIS2_PLACEMENT_3D ( 'NONE', #7239, #1913, #2060 ) ;
#10755 = ADVANCED_FACE ( 'NONE', ( #3464 ), #8784, .T. ) ;
#10756 = DIRECTION ( 'NONE',  ( -7.770718973608981122E-17, -0.9063077870366509359, 0.4226182617406975539 ) ) ;
#10757 = CARTESIAN_POINT ( 'NONE',  ( 85.05927807847463384, -5.579234875942719718, 3.390607678642486800 ) ) ;
#10758 = AXIS2_PLACEMENT_3D ( 'NONE', #32750, #32413, #29572 ) ;
#10759 = AXIS2_PLACEMENT_3D ( 'NONE', #7109, #22665, #30515 ) ;
#10760 = CARTESIAN_POINT ( 'NONE',  ( -0.2168228499942651821, -15.24168959956947234, 0.9788672205877712029 ) ) ;
#10761 = DIRECTION ( 'NONE',  ( 0.000000000000000000, 0.000000000000000000, 1.000000000000000000 ) ) ;
#10762 = ORIENTED_EDGE ( 'NONE', *, *, #12215, .F. ) ;
#10763 = FACE_OUTER_BOUND ( 'NONE', #11187, .T. ) ;
#10764 = AXIS2_PLACEMENT_3D ( 'NONE', #17796, #15611, #5101 ) ;
#10765 = EDGE_CURVE ( 'NONE', #3987, #18549, #11458, .T. ) ;
#10766 = CARTESIAN_POINT ( 'NONE',  ( 23.90742340929273624, -3.204431202270332513, 2.713652344655542503 ) ) ;
#10767 = CARTESIAN_POINT ( 'NONE',  ( 13.49495119401204413, 21.89891421162703011, -1.242381988985816532 ) ) ;
#10768 = ORIENTED_EDGE ( 'NONE', *, *, #22273, .F. ) ;
#10769 = CARTESIAN_POINT ( 'NONE',  ( 22.11000000136559507, -2.892927487894331406, 1.570731468192932301 ) ) ;
#10770 = VECTOR ( 'NONE', #6710, 999.9999999999998863 ) ;
#10772 = B_SPLINE_CURVE_WITH_KNOTS ( 'NONE', 3,
 ( #23615, #13398, #28788, #18945, #1220, #20955 ),
 .UNSPECIFIED., .F., .F.,
 ( 4, 2, 4 ),
 ( 0.009536920346932657028, 0.5047684601734664378, 1.000000000000000000 ),
 .UNSPECIFIED. ) ;
#10771 = VECTOR ( 'NONE', #824, 1000.000000000000000 ) ;
#10773 = CARTESIAN_POINT ( 'NONE',  ( -12.44989959798873791, 0.5000000000000000000, -12.99999999999999645 ) ) ;
#10774 = EDGE_CURVE ( 'NONE', #21855, #30672, #8927, .T. ) ;
#10775 = CARTESIAN_POINT ( 'NONE',  ( 19.69555400981637661, -21.64588847999016252, -1.456500879219860600 ) ) ;
#10776 = ORIENTED_EDGE ( 'NONE', *, *, #15880, .F. ) ;
#10777 = CARTESIAN_POINT ( 'NONE',  ( 23.95058674323790271, -2.449331254364353949, -0.07017451552781628354 ) ) ;
#10778 = EDGE_LOOP ( 'NONE', ( #24100, #12559, #32141, #2413, #15378 ) ) ;
#10779 = LINE ( 'NONE', #28335, #9186 ) ;
#10780 = EDGE_CURVE ( 'NONE', #1359, #10135, #7612, .T. ) ;
#10781 = B_SPLINE_SURFACE_WITH_KNOTS ( 'NONE', 3, 1, ( 
 ( #6228, #14079 ),
 ( #16412, #13890 ),
 ( #24281, #17262 ),
 ( #24936, #27277 ) ),
 .UNSPECIFIED., .F., .F., .F.,
 ( 4, 4 ),
 ( 2, 2 ),
 ( 0.001101513941755155341, 1.000000000000000000 ),
 ( 0.000000000000000000, 1.000000000000000000 ),
 .UNSPECIFIED. ) ;
#10782 = COORDINATED_UNIVERSAL_TIME_OFFSET ( 0, 0, .AHEAD. ) ;
#10784 = ORIENTED_EDGE ( 'NONE', *, *, #9113, .F. ) ;
#10783 = CARTESIAN_POINT ( 'NONE',  ( 9.331062908042635939, 15.00000000000000178, 4.629213727441584325 ) ) ;
#10785 = VERTEX_POINT ( 'NONE', #32367 ) ;
#10786 = CARTESIAN_POINT ( 'NONE',  ( 24.86000000136559507, -0.9349337715887247047, 3.156283516753367824 ) ) ;
#10787 = CIRCLE ( 'NONE', #8147, 2.999999999999998668 ) ;
#10788 = AXIS2_PLACEMENT_3D ( 'NONE', #14672, #21411, #27046 ) ;
#10789 = ORIENTED_EDGE ( 'NONE', *, *, #32437, .F. ) ;
#10790 = CARTESIAN_POINT ( 'NONE',  ( -7.650050800000001594, 1.549418761218566143, -2.853674364686379583 ) ) ;
#10792 = ORIENTED_EDGE ( 'NONE', *, *, #30254, .F. ) ;
#10791 = CARTESIAN_POINT ( 'NONE',  ( 68.92885037294648498, -3.291915072450345647, -0.8105619191593885775 ) ) ;
#10793 = AXIS2_PLACEMENT_3D ( 'NONE', #20725, #28404, #5520 ) ;
#10794 = CARTESIAN_POINT ( 'NONE',  ( 18.51491971917342028, -8.599446730134173933, 0.07017451552781803215 ) ) ;
#10795 = FACE_OUTER_BOUND ( 'NONE', #28974, .T. ) ;
#10796 = ADVANCED_FACE ( 'NONE', ( #10042 ), #30808, .F. ) ;
#10797 = FACE_OUTER_BOUND ( 'NONE', #6312, .T. ) ;
#10798 = EDGE_CURVE ( 'NONE', #4093, #13793, #4426, .T. ) ;
#10799 = CARTESIAN_POINT ( 'NONE',  ( -23.35000000000000142, -10.96966150227469505, -11.50000000000000000 ) ) ;
#10800 = ORIENTED_EDGE ( 'NONE', *, *, #28298, .F. ) ;
#10801 = PLANE ( 'NONE',  #4308 ) ;
#10802 = DIRECTION ( 'NONE',  ( -1.000000000000000000, 0.000000000000000000, 0.000000000000000000 ) ) ;
#10803 = CARTESIAN_POINT ( 'NONE',  ( 69.14445055419099617, -7.589252662747979272, -1.529340293471085355 ) ) ;
#10804 = CARTESIAN_POINT ( 'NONE',  ( 19.03654924710324892, -2.768675503676413019, -2.713652344655541615 ) ) ;
#10805 = CARTESIAN_POINT ( 'NONE',  ( 23.19698579062264443, -21.93770718891966709, 1.040523306341560428 ) ) ;
#10806 = VECTOR ( 'NONE', #10207, 1000.000000000000000 ) ;
#10807 = DIRECTION ( 'NONE',  ( -1.000000000000000000, 0.000000000000000000, 0.000000000000000000 ) ) ;
#10808 = DIRECTION ( 'NONE',  ( 0.000000000000000000, 0.000000000000000000, 1.000000000000000000 ) ) ;
#10809 = CARTESIAN_POINT ( 'NONE',  ( 21.36776303755519635, -21.72386242187942429, 1.606475753955313612 ) ) ;
#10810 = AXIS2_PLACEMENT_3D ( 'NONE', #3074, #30478, #10564 ) ;
#10811 = VECTOR ( 'NONE', #12727, 1000.000000000000114 ) ;
#10812 = CARTESIAN_POINT ( 'NONE',  ( -4.662550801365592967, 3.521866450007987037, 0.3701630799359328372 ) ) ;
#10813 = ORIENTED_EDGE ( 'NONE', *, *, #5362, .F. ) ;
#10814 = AXIS2_PLACEMENT_3D ( 'NONE', #12850, #28239, #10676 ) ;
#10816 = EDGE_CURVE ( 'NONE', #12536, #24760, #11884, .T. ) ;
#10815 = AXIS2_PLACEMENT_3D ( 'NONE', #14245, #28993, #13903 ) ;
#10817 = CARTESIAN_POINT ( 'NONE',  ( -3.004531657079156926, -1.883076972206379818, -2.325406398514292761 ) ) ;
#10818 = AXIS2_PLACEMENT_3D ( 'NONE', #2550, #20435, #20604 ) ;
#10819 = CARTESIAN_POINT ( 'NONE',  ( -7.000050800000000351, 0.000000000000000000, 0.000000000000000000 ) ) ;
#10820 = DIRECTION ( 'NONE',  ( 0.000000000000000000, 0.000000000000000000, 1.000000000000000000 ) ) ;
#10821 = CARTESIAN_POINT ( 'NONE',  ( 10.11068945975240396, -12.10067465535042963, 1.000000000000000000 ) ) ;
#10822 = AXIS2_PLACEMENT_3D ( 'NONE', #10527, #20741, #7210 ) ;
#10823 = ORIENTED_EDGE ( 'NONE', *, *, #21682, .F. ) ;
#10824 = DIRECTION ( 'NONE',  ( 0.000000000000000000, -0.9945218953682744001, 0.1045284632676437286 ) ) ;
#10825 = AXIS2_PLACEMENT_3D ( 'NONE', #17375, #6992, #27409 ) ;
#10826 = ORIENTED_EDGE ( 'NONE', *, *, #28752, .T. ) ;
#10827 = CARTESIAN_POINT ( 'NONE',  ( 1.205515411592139596, -3.374104910866653650, 1.499999999999999334 ) ) ;
#10828 = CALENDAR_DATE ( 2026, 6, 10 ) ;
#10829 = CARTESIAN_POINT ( 'NONE',  ( 54.97514302769123162, -6.431362512712788693, 4.093303786126267774 ) ) ;
#10830 = EDGE_CURVE ( 'NONE', #14757, #24556, #12562, .T. ) ;
#10831 = CONICAL_SURFACE ( 'NONE', #28970, 303.0536494382092769, 0.4915790642873723582 ) ;
#10832 = LINE ( 'NONE', #11000, #6954 ) ;
#10833 = VECTOR ( 'NONE', #29874, 1000.000000000000000 ) ;
#10834 = DIRECTION ( 'NONE',  ( -1.000000000000000000, 1.387778780781444413E-14, 0.000000000000000000 ) ) ;
#10835 = CIRCLE ( 'NONE', #27928, 10.94895958125474245 ) ;
#10836 = ORIENTED_EDGE ( 'NONE', *, *, #24028, .T. ) ;
#10837 = EDGE_CURVE ( 'NONE', #27172, #974, #30297, .T. ) ;
#10838 = CARTESIAN_POINT ( 'NONE',  ( 5.612718383992088889, -8.054241895195639600, 1.622626842546736503 ) ) ;
#10839 = EDGE_CURVE ( 'NONE', #14366, #26855, #20106, .T. ) ;
#10840 = CARTESIAN_POINT ( 'NONE',  ( 0.6791197464446645515, 9.138998021039178354, -0.5477823182331189589 ) ) ;
#10841 = VECTOR ( 'NONE', #19380, 1000.000000000000000 ) ;
#10842 = DIRECTION ( 'NONE',  ( -1.000000000000000000, 0.000000000000000000, 0.000000000000000000 ) ) ;
#10843 = VECTOR ( 'NONE', #2876, 1000.000000000000000 ) ;
#10845 = ORIENTED_EDGE ( 'NONE', *, *, #10639, .T. ) ;
#10844 = FACE_OUTER_BOUND ( 'NONE', #5128, .T. ) ;
#10846 = CARTESIAN_POINT ( 'NONE',  ( -2.912550801365593411, 1.088641768524161613, 3.675193018007247403 ) ) ;
#10847 = VECTOR ( 'NONE', #26881, 1000.000000000000000 ) ;
#10848 = DIRECTION ( 'NONE',  ( 1.000000000000000000, -0.000000000000000000, 6.943123467126514267E-15 ) ) ;
#10849 = CARTESIAN_POINT ( 'NONE',  ( 41.35430931302077795, -7.517178856329168823, -2.787783064041839953 ) ) ;
#10850 = VECTOR ( 'NONE', #6784, 1000.000000000000114 ) ;
#10851 = VERTEX_POINT ( 'NONE', #15553 ) ;
#10852 = EDGE_LOOP ( 'NONE', ( #19133, #10497, #10961, #25665 ) ) ;
#10853 = CARTESIAN_POINT ( 'NONE',  ( 0.000000000000000000, 5.227991826304090317, 9.620177616658001085 ) ) ;
#10854 = LINE ( 'NONE', #8489, #14605 ) ;
#10855 = FACE_OUTER_BOUND ( 'NONE', #22694, .T. ) ;
#10856 = EDGE_CURVE ( 'NONE', #635, #8281, #16144, .T. ) ;
#10857 = CARTESIAN_POINT ( 'NONE',  ( -2.617344628312510135, 0.000000000000000000, -1.468739241856748867 ) ) ;
#10858 = PRODUCT_RELATED_PRODUCT_CATEGORY ( 'detail', '', ( #12431 ) ) ;
#10859 = CIRCLE ( 'NONE', #6062, 2.999999999999999112 ) ;
#10860 = CARTESIAN_POINT ( 'NONE',  ( 10.00000000000000000, 4.753758587302147731, 3.462581523170085693E-33 ) ) ;
#10861 = VECTOR ( 'NONE', #28707, 1000.000000000000114 ) ;
#10862 = CARTESIAN_POINT ( 'NONE',  ( 107.9718772962921776, -17.66440217927672762, -4.377269687808228227 ) ) ;
#10863 = DIRECTION ( 'NONE',  ( -0.000000000000000000, 0.000000000000000000, 1.000000000000000000 ) ) ;
#10864 = VERTEX_POINT ( 'NONE', #22156 ) ;
#10865 = CARTESIAN_POINT ( 'NONE',  ( -53.72801162551947840, 5.497307881342318403, 1.430198536305348656 ) ) ;
#10866 = AXIS2_PLACEMENT_3D ( 'NONE', #702, #19069, #4177 ) ;
#10867 = B_SPLINE_CURVE_WITH_KNOTS ( 'NONE', 3,
 ( #22768, #15385, #30456, #8220, #5057, #18420, #10043, #25773, #5556, #27950 ),
 .UNSPECIFIED., .F., .F.,
 ( 4, 3, 3, 4 ),
 ( 8.673617379884035472E-19, 0.001000000000064768307, 0.002000000000131801729, 0.003364209820980246842 ),
 .UNSPECIFIED. ) ;
#10868 = ORIENTED_EDGE ( 'NONE', *, *, #16741, .T. ) ;
#10869 = APPROVAL_ROLE ( '' ) ;
#10871 = PLANE ( 'NONE',  #6990 ) ;
#10870 = CC_DESIGN_APPROVAL ( #26006, ( #7128 ) ) ;
#10872 = ORIENTED_EDGE ( 'NONE', *, *, #6291, .F. ) ;
#10873 = EDGE_CURVE ( 'NONE', #29889, #32584, #2701, .T. ) ;
#10874 = B_SPLINE_CURVE_WITH_KNOTS ( 'NONE', 3,
 ( #28502, #25831, #5605, #20969, #13409, #5751, #3248, #23628 ),
 .UNSPECIFIED., .F., .F.,
 ( 4, 2, 2, 4 ),
 ( 2.494123547463239299E-07, 0.001262099805913989873, 0.001893025002693609444, 0.002523950199473228798 ),
 .UNSPECIFIED. ) ;
#10875 = CARTESIAN_POINT ( 'NONE',  ( 35.00000000000000000, 0.000000000000000000, -2.999999999999995559 ) ) ;
#10876 = ORIENTED_EDGE ( 'NONE', *, *, #29391, .T. ) ;
#10877 = CARTESIAN_POINT ( 'NONE',  ( 4.075891499408641642E-16, 4.753758587302147731, 0.000000000000000000 ) ) ;
#10878 = B_SPLINE_CURVE_WITH_KNOTS ( 'NONE', 3,
 ( #25524, #4640, #27544, #30068, #30383, #12494, #22525, #17495 ),
 .UNSPECIFIED., .F., .F.,
 ( 4, 2, 2, 4 ),
 ( 5.099451029794817991E-07, 0.001229189590460703658, 0.001843529413139567913, 0.002457869235818432169 ),
 .UNSPECIFIED. ) ;
#10880 = VERTEX_POINT ( 'NONE', #11768 ) ;
#10879 = CARTESIAN_POINT ( 'NONE',  ( 102.3561127732198770, -3.030023377210125712, -4.185347658349727773 ) ) ;
#10881 = ORIENTED_EDGE ( 'NONE', *, *, #25250, .T. ) ;
#10882 = CARTESIAN_POINT ( 'NONE',  ( 13.13178786249840435, -17.31629153505178920, -4.522129901861164925 ) ) ;
#10883 = CARTESIAN_POINT ( 'NONE',  ( -3.762550801365593500, 2.228590825266444142, 2.752080473201636845 ) ) ;
#10884 = CARTESIAN_POINT ( 'NONE',  ( 25.79749999999999943, 0.7685399846772009713, -2.594547506269381909 ) ) ;
#10885 = CARTESIAN_POINT ( 'NONE',  ( 0.9067410411906208223, -4.287332675150268280, -1.499999999999999556 ) ) ;
#10887 = ORIENTED_EDGE ( 'NONE', *, *, #13334, .T. ) ;
#10886 = DIRECTION ( 'NONE',  ( -1.211557572730276143E-16, -3.469446951953611428E-15, -1.000000000000000000 ) ) ;
#10888 = AXIS2_PLACEMENT_3D ( 'NONE', #20925, #28456, #17930 ) ;
#10889 = DIRECTION ( 'NONE',  ( 1.000000000000000000, -1.447395388606377867E-16, 3.132748819842649948E-17 ) ) ;
#10890 = CARTESIAN_POINT ( 'NONE',  ( 12.22374906563888963, 4.895420474595863602, 1.499999999999170441 ) ) ;
#10891 =( BOUNDED_CURVE ( )  B_SPLINE_CURVE ( 3, ( #25879, #3138, #12650, #26034 ),
 .UNSPECIFIED., .F., .F. ) 
 B_SPLINE_CURVE_WITH_KNOTS ( ( 4, 4 ),
 ( 1.570796326794896558, 1.762782544514152949 ),
 .UNSPECIFIED. ) 
 CURVE ( )  GEOMETRIC_REPRESENTATION_ITEM ( )  RATIONAL_B_SPLINE_CURVE ( ( 1.000000000000000000, 0.9969307989114561952, 0.9969307989114561952, 1.000000000000000000 ) ) 
 REPRESENTATION_ITEM ( '' )  );
#10892 = CARTESIAN_POINT ( 'NONE',  ( 0.000000000000000000, -5.227991826304158707, 9.620177616657965558 ) ) ;
#10893 = CARTESIAN_POINT ( 'NONE',  ( -15.12340757463330654, -27.93932300454937590, -1.500000000000000000 ) ) ;
#10894 = CIRCLE ( 'NONE', #22113, 6.248999999999999666 ) ;
#10895 = DIRECTION ( 'NONE',  ( 1.000000000000000000, -0.000000000000000000, -0.000000000000000000 ) ) ;
#10897 = ORIENTED_EDGE ( 'NONE', *, *, #24060, .T. ) ;
#10896 = DIRECTION ( 'NONE',  ( -4.917867153433062508E-17, -0.5735764363510531538, 0.8191520442889869136 ) ) ;
#10898 = CARTESIAN_POINT ( 'NONE',  ( 7.249760686538667009, -6.940565734314570356, -4.007137495034885255 ) ) ;
#10899 = CARTESIAN_POINT ( 'NONE',  ( 107.3476950949991391, -15.88628029827230925, 1.500000000000000000 ) ) ;
#10900 = CARTESIAN_POINT ( 'NONE',  ( 24.54750000273118715, -0.7685399846772070775, 2.594547506269381465 ) ) ;
#10901 = CC_DESIGN_APPROVAL ( #30093, ( #26379 ) ) ;
#10902 = EDGE_CURVE ( 'NONE', #10851, #8114, #21970, .T. ) ;
#10903 = CARTESIAN_POINT ( 'NONE',  ( -19.48091229030179150, 5.440830098942543103, 2.106297401565688787 ) ) ;
#10904 = CARTESIAN_POINT ( 'NONE',  ( 47.40009415622113664, 24.02318594975524491, 5.412820279296879811 ) ) ;
#10905 = DIRECTION ( 'NONE',  ( -1.000000000000000000, 8.574039729943018344E-17, -0.000000000000000000 ) ) ;
#10906 = CARTESIAN_POINT ( 'NONE',  ( 10.00000000000000000, -4.616489984850546513, 1.946309384392575392 ) ) ;
#10907 = CARTESIAN_POINT ( 'NONE',  ( 5.377543748152548986, -6.139290821770219786, -5.151476664237539360 ) ) ;
#10908 = EDGE_LOOP ( 'NONE', ( #10133, #5047, #20326, #17471 ) ) ;
#10909 = AXIS2_PLACEMENT_3D ( 'NONE', #9977, #4796, #17657 ) ;
#10910 = LINE ( 'NONE', #21262, #27868 ) ;
#10911 = DIRECTION ( 'NONE',  ( 1.000000000000000000, 0.000000000000000000, 0.000000000000000000 ) ) ;
#10912 = CARTESIAN_POINT ( 'NONE',  ( 7.064423539573518873, -8.721381771257245674, 0.7071067811875828557 ) ) ;
#10914 = CARTESIAN_POINT ( 'NONE',  ( 107.9851147162994351, -17.85501773432275741, 4.472621839076901473 ) ) ;
#10913 = CARTESIAN_POINT ( 'NONE',  ( 10.56183597391177464, -5.003758587302149508, -0.2500000000000008882 ) ) ;
#10915 = ADVANCED_FACE ( 'NONE', ( #20253 ), #19490, .T. ) ;
#10916 = ORIENTED_EDGE ( 'NONE', *, *, #3420, .T. ) ;
#10917 = EDGE_CURVE ( 'NONE', #18770, #18479, #32197, .T. ) ;
#10918 = DIRECTION ( 'NONE',  ( 0.6195800045172923376, -0.7849335118354624496, 0.000000000000000000 ) ) ;
#10919 = ORIENTED_EDGE ( 'NONE', *, *, #26232, .F. ) ;
#10920 = PLANE ( 'NONE',  #1188 ) ;
#10921 = EDGE_CURVE ( 'NONE', #13878, #19582, #27949, .T. ) ;
#10923 = ORIENTED_EDGE ( 'NONE', *, *, #19820, .F. ) ;
#10922 = CARTESIAN_POINT ( 'NONE',  ( 102.3439814245641344, -2.854902261435320110, -3.993434327320336319 ) ) ;
#10924 = ORIENTED_EDGE ( 'NONE', *, *, #27238, .T. ) ;
#10925 = LINE ( 'NONE', #11229, #28936 ) ;
#10926 = LOCAL_TIME ( 16, 7, 10.00000000000000000, #591 ) ;
#10927 = CARTESIAN_POINT ( 'NONE',  ( 7.249760686538667009, 7.892520144992435149, 1.391664247347255134 ) ) ;
#10929 = ORIENTED_EDGE ( 'NONE', *, *, #32794, .T. ) ;
#10928 = CARTESIAN_POINT ( 'NONE',  ( 17.32050807568873552, 10.00000000000002309, 1.508259000770581615 ) ) ;
#10930 = VERTEX_POINT ( 'NONE', #9268 ) ;
#10931 = CARTESIAN_POINT ( 'NONE',  ( 107.5147077154356481, 18.30459826903478771, 4.414771370926589000 ) ) ;
#10932 = CARTESIAN_POINT ( 'NONE',  ( 18.69993402965692653, -6.531358056919786215, 2.942092882392380648 ) ) ;
#10933 = CARTESIAN_POINT ( 'NONE',  ( 23.15368348421675293, -16.86203458153637058, -1.000000000000000444 ) ) ;
#10934 = CARTESIAN_POINT ( 'NONE',  ( -2.476225935960405966, -0.3178988483021057410, 3.024605502323848949 ) ) ;
#10935 = CARTESIAN_POINT ( 'NONE',  ( 101.6022419886208610, -1.170867242066747416, 0.07017451552782490165 ) ) ;
#10936 = CIRCLE ( 'NONE', #12007, 7.981930256614262476 ) ;
#10937 = CARTESIAN_POINT ( 'NONE',  ( -8.000050800000000351, -1.836970198721030181E-16, -3.000000000000000444 ) ) ;
#10938 = CARTESIAN_POINT ( 'NONE',  ( 9.130194559407742716, -14.25877845138838751, 1.499999999999999778 ) ) ;
#10939 = CARTESIAN_POINT ( 'NONE',  ( 47.94319819119432680, -7.452467522312293369, 2.787782382152882654 ) ) ;
#10940 = B_SPLINE_CURVE_WITH_KNOTS ( 'NONE', 3,
 ( #1637, #12155, #32258, #22353, #32566, #9637, #14818, #2130, #12311, #32749, #22527, #27694, #4798, #14976, #18158, #615, #12797, #2634, #7817, #23012, #18348, #21025, #30895, #18504, #5791, #33055, #28049, #10482, #454, #20536 ),
 .UNSPECIFIED., .F., .F.,
 ( 4, 2, 2, 2, 2, 2, 2, 2, 2, 2, 2, 2, 2, 2, 4 ),
 ( -0.008140911791333830735, -0.007115276677915103633, -0.006602459121205740515, -0.006089641564496376530, -0.005576824007787013412, -0.005064006451077650295, -0.004038371337658924060, -0.003525553780949560942, -0.003012736224240198692, -0.002499918667530834707, -0.001987101110821470722, -0.001474283554112107604, -0.0009614659974027444864, -0.0004486484406933805014, 6.416911601598088155E-05 ),
 .UNSPECIFIED. ) ;
#10941 = CARTESIAN_POINT ( 'NONE',  ( 110.4915906369627123, -18.78144465615449832, 4.522129901861158707 ) ) ;
#10942 = CARTESIAN_POINT ( 'NONE',  ( 3.406359441062990268, 0.6647459039674525894, 0.7949826693599013616 ) ) ;
#10943 = EDGE_LOOP ( 'NONE', ( #23843, #13435, #17830, #30090 ) ) ;
#10944 = CARTESIAN_POINT ( 'NONE',  ( 5.489343958331426521, -2.874233210898315072, -7.593062460271022829 ) ) ;
#10945 = B_SPLINE_CURVE_WITH_KNOTS ( 'NONE', 3,
 ( #25284, #28269, #30661, #15393, #376, #12886 ),
 .UNSPECIFIED., .F., .F.,
 ( 4, 2, 4 ),
 ( 0.000000000000000000, 0.001111101129502802768, 0.002222202259005605536 ),
 .UNSPECIFIED. ) ;
#10946 = CARTESIAN_POINT ( 'NONE',  ( 107.9195515681646214, 17.73019131298662643, 3.374709941095086041 ) ) ;
#10947 = DIRECTION ( 'NONE',  ( -0.000000000000000000, -1.000000000000000000, -0.000000000000000000 ) ) ;
#10948 = VERTEX_POINT ( 'NONE', #4874 ) ;
#10949 = CARTESIAN_POINT ( 'NONE',  ( 23.36000000136559507, -1.570731468192933633, -2.892927487894330074 ) ) ;
#10950 = EDGE_CURVE ( 'NONE', #8263, #6649, #15055, .T. ) ;
#10951 = CARTESIAN_POINT ( 'NONE',  ( 25.46140505637537643, -2.308950792538006613, -1.460408169760519792 ) ) ;
#10952 = CARTESIAN_POINT ( 'NONE',  ( 109.6329156864505165, 19.01855260168436246, -4.612695725900422872 ) ) ;
#10953 = VERTEX_POINT ( 'NONE', #25436 ) ;
#10954 = CARTESIAN_POINT ( 'NONE',  ( 4.959835597591649048, -12.47346298686548849, -1.499999999999999334 ) ) ;
#10955 =( NAMED_UNIT ( * ) SI_UNIT ( $, .STERADIAN. ) SOLID_ANGLE_UNIT ( ) );
#10956 = EDGE_LOOP ( 'NONE', ( #5194, #18135, #28606, #5568, #1748, #24892, #16121, #3528 ) ) ;
#10957 = ORIENTED_EDGE ( 'NONE', *, *, #13974, .F. ) ;
#10958 = CARTESIAN_POINT ( 'NONE',  ( 17.41559371906258136, 18.02474698348859405, 1.508259000770581615 ) ) ;
#10959 = COORDINATED_UNIVERSAL_TIME_OFFSET ( 0, 0, .AHEAD. ) ;
#10961 = ORIENTED_EDGE ( 'NONE', *, *, #3047, .F. ) ;
#10960 = CARTESIAN_POINT ( 'NONE',  ( 23.04750000000000654, 2.594547506269380133, 0.7685399846772031918 ) ) ;
#10962 = ORIENTED_EDGE ( 'NONE', *, *, #22893, .T. ) ;
#10963 = CARTESIAN_POINT ( 'NONE',  ( 25.48500000136559507, 2.892927487894327410, -1.570731468192931635 ) ) ;
#10964 = ORIENTED_EDGE ( 'NONE', *, *, #21300, .F. ) ;
#10965 = CARTESIAN_POINT ( 'NONE',  ( -7.450050800000001416, 2.853674364686379583, 1.549418761218565921 ) ) ;
#10967 = VERTEX_POINT ( 'NONE', #12714 ) ;
#10966 = DIRECTION ( 'NONE',  ( 0.000000000000000000, -0.08715574274765797158, -0.9961946980917455452 ) ) ;
#10968 = CARTESIAN_POINT ( 'NONE',  ( 21.32535692059155963, -21.82495604402122069, 1.318256435726650633 ) ) ;
#10969 = CARTESIAN_POINT ( 'NONE',  ( -53.35155202832373078, 4.402097243136370963, 5.049999999999999822 ) ) ;
#10970 = DIRECTION ( 'NONE',  ( 1.000000000000000000, -8.574039729943018344E-17, -0.000000000000000000 ) ) ;
#10971 = CARTESIAN_POINT ( 'NONE',  ( 0.6728000687415590653, 8.860258565202267178, -2.287261066729833647 ) ) ;
#10972 = DIRECTION ( 'NONE',  ( -1.000000000000000000, -0.000000000000000000, -0.000000000000000000 ) ) ;
#10973 = B_SPLINE_CURVE_WITH_KNOTS ( 'NONE', 3,
 ( #20002, #25150, #2597, #12947, #2270, #15123, #7605, #7272 ),
 .UNSPECIFIED., .F., .F.,
 ( 4, 2, 2, 4 ),
 ( 2.304311362624057754E-07, 0.001064504214901549435, 0.001596641106784193239, 0.002128777998666837260 ),
 .UNSPECIFIED. ) ;
#10974 = EDGE_LOOP ( 'NONE', ( #18628, #10747, #23960, #17992 ) ) ;
#10975 = DIRECTION ( 'NONE',  ( 0.000000000000000000, 0.000000000000000000, -1.000000000000000000 ) ) ;
#10976 = CARTESIAN_POINT ( 'NONE',  ( -2.673784050203184215, -0.4252642838279113713, -1.725835265963347798 ) ) ;
#10977 = CARTESIAN_POINT ( 'NONE',  ( 47.95525692263769457, -8.175714017047097215, -1.529339665925934177 ) ) ;
#10978 = FACE_OUTER_BOUND ( 'NONE', #14552, .T. ) ;
#10979 = EDGE_CURVE ( 'NONE', #25776, #1551, #569, .T. ) ;
#10980 = DIRECTION ( 'NONE',  ( 1.000000000000000000, 0.000000000000000000, 0.000000000000000000 ) ) ;
#10981 = CYLINDRICAL_SURFACE ( 'NONE', #27847, 4.000000000000001776 ) ;
#10982 = CARTESIAN_POINT ( 'NONE',  ( 26.44001828968095680, 18.17676778675652471, 2.806473568333413660 ) ) ;
#10983 = EDGE_CURVE ( 'NONE', #30369, #26986, #18231, .T. ) ;
#10984 = CARTESIAN_POINT ( 'NONE',  ( -27.13750370378988919, 4.491141813158496809, 1.500000000000000000 ) ) ;
#10985 = CARTESIAN_POINT ( 'NONE',  ( -4.862550801365594033, 0.3701630799359330593, -3.521866450007987037 ) ) ;
#10986 = EDGE_LOOP ( 'NONE', ( #20637, #32226, #4384, #2712, #25978 ) ) ;
#10987 = CARTESIAN_POINT ( 'NONE',  ( -6.150050800000001594, -0.9222479816126459840, -3.113457007523259268 ) ) ;
#10988 = CARTESIAN_POINT ( 'NONE',  ( 107.6901504273134975, 19.30156402555556028, 4.744684166805590131 ) ) ;
#10989 = EDGE_CURVE ( 'NONE', #24814, #17909, #23108, .T. ) ;
#10990 = CARTESIAN_POINT ( 'NONE',  ( 20.74999999999999645, 5.999999999999999112, 0.000000000000000000 ) ) ;
#10991 = CARTESIAN_POINT ( 'NONE',  ( 8.486535498732452609, -10.66169397748241998, 1.000000000000000000 ) ) ;
#10992 = ORIENTED_EDGE ( 'NONE', *, *, #10873, .T. ) ;
#10993 = CARTESIAN_POINT ( 'NONE',  ( 40.87146290595926956, -4.622005974792367411, -2.184956282064931088 ) ) ;
#10994 = EDGE_CURVE ( 'NONE', #16940, #9839, #8032, .T. ) ;
#10995 = VERTEX_POINT ( 'NONE', #863 ) ;
#10996 = CARTESIAN_POINT ( 'NONE',  ( 2.281627749324421917, -0.2935656086769610207, 1.757435426329174044 ) ) ;
#10997 = APPROVAL_DATE_TIME ( #3155, #7375 ) ;
#10998 = CARTESIAN_POINT ( 'NONE',  ( 28.68200330691262323, -6.065191176973169895, 4.312042181588143563 ) ) ;
#10999 = EDGE_CURVE ( 'NONE', #5581, #19600, #13696, .T. ) ;
#11000 = CARTESIAN_POINT ( 'NONE',  ( 3.499999999999999556, -0.1221666339523235223, -6.247805719894684806 ) ) ;
#11001 = CARTESIAN_POINT ( 'NONE',  ( -12.44989959798873791, 6.043040383381309791E-17, -2.999999999999995559 ) ) ;
#11002 = VERTEX_POINT ( 'NONE', #8219 ) ;
#11003 = CARTESIAN_POINT ( 'NONE',  ( 0.000000000000000000, 8.265874651078018331, 1.981241088980808751 ) ) ;
#11004 = CYLINDRICAL_SURFACE ( 'NONE', #26771, 6.248999999999999666 ) ;
#11005 = DIRECTION ( 'NONE',  ( 0.000000000000000000, 0.000000000000000000, -1.000000000000000000 ) ) ;
#11006 = EDGE_CURVE ( 'NONE', #16325, #12581, #3051, .T. ) ;
#11008 = VERTEX_POINT ( 'NONE', #5703 ) ;
#11007 = CARTESIAN_POINT ( 'NONE',  ( -23.35000000000000142, -10.96966150227469505, -11.00000000000000000 ) ) ;
#11009 = CARTESIAN_POINT ( 'NONE',  ( -3.362550801365593589, -2.228590825266444586, -2.752080473201636401 ) ) ;
#11010 = PLANE ( 'NONE',  #21410 ) ;
#11011 = DIRECTION ( 'NONE',  ( 1.000000000000000000, 0.000000000000000000, -0.000000000000000000 ) ) ;
#11012 = ORIENTED_EDGE ( 'NONE', *, *, #14602, .F. ) ;
#11013 = ORIENTED_EDGE ( 'NONE', *, *, #28395, .T. ) ;
#11014 = DIRECTION ( 'NONE',  ( -1.000000000000000000, 0.000000000000000000, 0.000000000000000000 ) ) ;
#11015 = CARTESIAN_POINT ( 'NONE',  ( 20.74999999999999645, -1.779113243963176091E-15, 0.000000000000000000 ) ) ;
#11016 = DIRECTION ( 'NONE',  ( 0.000000000000000000, -1.000000000000000000, 0.000000000000000000 ) ) ;
#11017 = CARTESIAN_POINT ( 'NONE',  ( -1.425727661597485874, -5.130997865967673377, 5.485967528433933538 ) ) ;
#11018 = ORIENTED_EDGE ( 'NONE', *, *, #5217, .T. ) ;
#11019 = FACE_OUTER_BOUND ( 'NONE', #4592, .T. ) ;
#11020 = CARTESIAN_POINT ( 'NONE',  ( 17.33093461831550286, -21.43932300456650353, -1.499999999999999112 ) ) ;
#11021 = CARTESIAN_POINT ( 'NONE',  ( -58.99735576046915497, -4.718558500561493396, 5.402788590778398792 ) ) ;
#11022 = CARTESIAN_POINT ( 'NONE',  ( -3.187550801365593767, 3.521866450007987037, 0.3701630799359328372 ) ) ;
#11023 = EDGE_CURVE ( 'NONE', #140, #13341, #30481, .T. ) ;
#11024 = CARTESIAN_POINT ( 'NONE',  ( 9.331062908042635939, 15.00000000000000178, 4.629213727441584325 ) ) ;
#11025 = CARTESIAN_POINT ( 'NONE',  ( 29.18511942701327300, -8.255514837368274073, 0.8105614686238012956 ) ) ;
#11026 = EDGE_LOOP ( 'NONE', ( #14877, #208, #1895, #14250 ) ) ;
#11027 = FACE_OUTER_BOUND ( 'NONE', #1075, .T. ) ;
#11028 = ADVANCED_FACE ( 'NONE', ( #13205 ), #21533, .T. ) ;
#11029 = ORIENTED_EDGE ( 'NONE', *, *, #9068, .T. ) ;
#11030 = APPROVAL_DATE_TIME ( #26080, #16568 ) ;
#11031 = CARTESIAN_POINT ( 'NONE',  ( 18.75828436637440433, -5.879118399754064583, 3.993434335971381532 ) ) ;
#11032 = EDGE_CURVE ( 'NONE', #13341, #28440, #9326, .T. ) ;
#11033 = DIRECTION ( 'NONE',  ( 0.000000000000000000, 0.000000000000000000, 1.000000000000000000 ) ) ;
#11034 = ORIENTED_EDGE ( 'NONE', *, *, #2772, .F. ) ;
#11035 = CARTESIAN_POINT ( 'NONE',  ( -2.986472588763606328, 8.217301096052205839E-30, -1.110524573187248620 ) ) ;
#11036 = EDGE_LOOP ( 'NONE', ( #243, #23613 ) ) ;
#11037 = ORIENTED_EDGE ( 'NONE', *, *, #16432, .F. ) ;
#11038 = CARTESIAN_POINT ( 'NONE',  ( 2.037945749704362236E-16, 2.376879293651122271, -4.116875700062057497 ) ) ;
#11039 = CARTESIAN_POINT ( 'NONE',  ( -3.962550801365593234, 2.752080473201636845, -2.228590825266444142 ) ) ;
#11040 = CARTESIAN_POINT ( 'NONE',  ( 6.751043368244950216, -5.560327249377744252, 1.500000000000000222 ) ) ;
#11041 = EDGE_CURVE ( 'NONE', #21569, #7000, #3768, .T. ) ;
#11042 = CARTESIAN_POINT ( 'NONE',  ( 0.5362739657699832074, -4.520875221154571300, -1.499999999999964917 ) ) ;
#11043 = CC_DESIGN_DATE_AND_TIME_ASSIGNMENT ( #16474, #26681, ( #32113 ) ) ;
#11045 = ORIENTED_EDGE ( 'NONE', *, *, #20557, .T. ) ;
#11044 = CARTESIAN_POINT ( 'NONE',  ( 14.84037634778394299, 10.17686136595211366, -1.499999999999999778 ) ) ;
#11046 = CARTESIAN_POINT ( 'NONE',  ( -5.087550801365593678, -2.228590825266444586, -2.752080473201636401 ) ) ;
#11047 = CARTESIAN_POINT ( 'NONE',  ( 10.51841884079962064, 2.077444665211660713, 1.050000000000000044 ) ) ;
#11048 = CARTESIAN_POINT ( 'NONE',  ( 5.612974044843315191, 1.622927203279449282, -8.054452210044747318 ) ) ;
#11049 = DIRECTION ( 'NONE',  ( -0.9993908270190956511, 0.03489949670250350189, -8.673617379884042375E-16 ) ) ;
#11051 = ORIENTED_EDGE ( 'NONE', *, *, #13508, .F. ) ;
#11050 = DIRECTION ( 'NONE',  ( -1.000000000000000000, -0.000000000000000000, 0.000000000000000000 ) ) ;
#11052 = CARTESIAN_POINT ( 'NONE',  ( -28.89553135701950737, 6.931071537538192828, 2.065847295955301366 ) ) ;
#11053 = CARTESIAN_POINT ( 'NONE',  ( 21.11000000273118715, 1.573300977624590313, -1.942864903642426144 ) ) ;
#11054 = CARTESIAN_POINT ( 'NONE',  ( 5.612974044843316079, -1.229732182294847487, -8.123783100924562461 ) ) ;
#11055 = CARTESIAN_POINT ( 'NONE',  ( 4.749760686538667009, -7.530955069117533540, 2.741043480754901118 ) ) ;
#11056 = CARTESIAN_POINT ( 'NONE',  ( -2.753702574462014052, -0.2727682784858890819, -1.454428814729283870 ) ) ;
#11057 = DIRECTION ( 'NONE',  ( -8.541412920197225978E-17, -0.9961946980917466554, 0.08715574274764535667 ) ) ;
#11058 = EDGE_CURVE ( 'NONE', #10525, #7245, #2171, .T. ) ;
#11059 = CARTESIAN_POINT ( 'NONE',  ( 10.57125986779756843, 4.884328206559851004, -1.115095498423258391 ) ) ;
#11060 = CARTESIAN_POINT ( 'NONE',  ( -4.637550801365592612, 1.088641768524161613, 3.675193018007247403 ) ) ;
#11061 = ORIENTED_EDGE ( 'NONE', *, *, #13580, .T. ) ;
#11062 = CARTESIAN_POINT ( 'NONE',  ( 20.08514749461460269, -21.49093168682494692, 1.640482353826733242 ) ) ;
#11063 = CARTESIAN_POINT ( 'NONE',  ( 0.000000000000000000, 0.000000000000000000, 0.000000000000000000 ) ) ;
#11064 = CARTESIAN_POINT ( 'NONE',  ( 47.75999538435752356, -8.435302152669851949, -0.07017451552783426916 ) ) ;
#11066 = CARTESIAN_POINT ( 'NONE',  ( 107.9806159500837452, -17.79023661996872718, 4.339996101326005551 ) ) ;
#11065 = CARTESIAN_POINT ( 'NONE',  ( 108.0191616676854665, 18.28485965138728986, -4.516253933250887975 ) ) ;
#11067 = ORIENTED_EDGE ( 'NONE', *, *, #7297, .T. ) ;
#11068 = CARTESIAN_POINT ( 'NONE',  ( 2.274274201625318348, -5.222868219166783454, -9.680994141368850947 ) ) ;
#11069 = ORIENTED_EDGE ( 'NONE', *, *, #19550, .F. ) ;
#11070 =( BOUNDED_SURFACE ( )  B_SPLINE_SURFACE ( 3, 2, ( 
 ( #31315, #26290, #13870 ),
 ( #23601, #5870, #3401 ),
 ( #23921, #31636, #6209 ),
 ( #19083, #23771, #885 ),
 ( #11062, #31461, #8540 ),
 ( #16392, #24077, #29270 ),
 ( #26604, #1207, #6357 ),
 ( #16552, #3882, #14057 ),
 ( #6707, #24764, #1695 ),
 ( #32464, #14872, #27093 ) ),
 .UNSPECIFIED., .F., .F., .F. ) 
 B_SPLINE_SURFACE_WITH_KNOTS ( ( 4, 2, 2, 2, 4 ),
 ( 3, 3 ),
 ( 0.01791456443260443579, 0.01997296323900674131, 0.02100216264220789580, 0.02151676234380847305, 0.02203136204540905030 ),
 ( 0.000000000000000000, 1.000000000000000000 ),
 .UNSPECIFIED. ) 
 GEOMETRIC_REPRESENTATION_ITEM ( )  RATIONAL_B_SPLINE_SURFACE ( (
 ( 1.000000000000000000, 0.8490876263417815872, 1.000000000000000000),
 ( 1.000000000000000000, 0.8789005871655674040, 1.000000000000000000),
 ( 1.000000000000000000, 0.9052476245296197099, 1.000000000000000000),
 ( 1.000000000000000000, 0.9409176603636237868, 1.000000000000000000),
 ( 1.000000000000000000, 0.9521522767065306869, 1.000000000000000000),
 ( 1.000000000000000000, 0.9681060328969361972, 1.000000000000000000),
 ( 1.000000000000000000, 0.9732806895434287231, 1.000000000000000000),
 ( 1.000000000000000000, 0.9832765258106581641, 1.000000000000000000),
 ( 1.000000000000000000, 0.9881226520953384496, 1.000000000000000000),
 ( 1.000000000000000000, 0.9925898118721221408, 1.000000000000000000) ) ) 
 REPRESENTATION_ITEM ( '' )  SURFACE ( )  );
#11071 = DIRECTION ( 'NONE',  ( -1.000000000000000000, 0.000000000000000000, 0.000000000000000000 ) ) ;
#11073 = ORIENTED_EDGE ( 'NONE', *, *, #10592, .F. ) ;
#11072 = CARTESIAN_POINT ( 'NONE',  ( 108.2141205071562098, 20.71718940879397763, -1.479437267284251067 ) ) ;
#11074 = ORIENTED_EDGE ( 'NONE', *, *, #20734, .F. ) ;
#11075 = CARTESIAN_POINT ( 'NONE',  ( 29.21519671786122885, -8.552672223070194590, -2.713652344655543391 ) ) ;
#11076 = ADVANCED_FACE ( 'NONE', ( #5513 ), #32209, .T. ) ;
#11077 = CARTESIAN_POINT ( 'NONE',  ( 23.04481819307383716, -21.91824019632983678, -1.499999999999999556 ) ) ;
#11079 = VERTEX_POINT ( 'NONE', #18527 ) ;
#11078 = CARTESIAN_POINT ( 'NONE',  ( 108.0068349480237515, 18.21621961241920573, 4.414771370926588112 ) ) ;
#11080 = CARTESIAN_POINT ( 'NONE',  ( 15.00732532914695305, 9.584243417931569198, -1.050000000000000044 ) ) ;
#11081 = CARTESIAN_POINT ( 'NONE',  ( -2.558315521542159132, 0.4094970184090410137, -1.491740999229417941 ) ) ;
#11082 = DIRECTION ( 'NONE',  ( -1.000000000000000000, 0.000000000000000000, 0.000000000000000000 ) ) ;
#11083 = CARTESIAN_POINT ( 'NONE',  ( 8.901201215455881055, 15.00000000000000000, -5.396302277755718357 ) ) ;
#11084 = CARTESIAN_POINT ( 'NONE',  ( 107.9299262097015202, -17.06031696848630119, -2.839861482690292149 ) ) ;
#11085 = CARTESIAN_POINT ( 'NONE',  ( 8.911384905465473238, 0.2172754300402908179, -1.412391582771881371 ) ) ;
#11086 = B_SPLINE_CURVE_WITH_KNOTS ( 'NONE', 3,
 ( #27034, #29873, #26690, #13977, #21841, #19524 ),
 .UNSPECIFIED., .F., .F.,
 ( 4, 2, 4 ),
 ( 0.000000000000000000, 0.0003933473255787851234, 0.0007866946511575702468 ),
 .UNSPECIFIED. ) ;
#11087 = DIRECTION ( 'NONE',  ( 0.000000000000000000, -0.9056868434500645604, 0.4239473335232317175 ) ) ;
#11088 = CARTESIAN_POINT ( 'NONE',  ( 10.00000000000000000, 4.893557421779793832E-14, -4.753758587302147731 ) ) ;
#11089 = EDGE_CURVE ( 'NONE', #20196, #10337, #12427, .T. ) ;
#11090 = CARTESIAN_POINT ( 'NONE',  ( -3.370691070153704949, -1.614088942876946264, 1.500000000000000000 ) ) ;
#11091 = CARTESIAN_POINT ( 'NONE',  ( 2.535833972131079417, -0.1672301947041110182, 1.432210082195920720 ) ) ;
#11092 = ORIENTED_EDGE ( 'NONE', *, *, #31638, .T. ) ;
#11093 = DIRECTION ( 'NONE',  ( 1.000000000000000000, -6.938893903907222067E-15, 0.000000000000000000 ) ) ;
#11094 = ADVANCED_FACE ( 'NONE', ( #479 ), #8479, .T. ) ;
#11095 = DIRECTION ( 'NONE',  ( -1.000000000000000000, 0.000000000000000000, 0.000000000000000000 ) ) ;
#11096 = CARTESIAN_POINT ( 'NONE',  ( 2.864530875629069051, 9.539603485476133571, 0.6595692664037854369 ) ) ;
#11097 = ORIENTED_EDGE ( 'NONE', *, *, #10774, .T. ) ;
#11098 = CARTESIAN_POINT ( 'NONE',  ( 24.29750000136559507, -2.363507492473152283, -1.913930629741525280 ) ) ;
#11099 = FACE_OUTER_BOUND ( 'NONE', #206, .T. ) ;
#11100 = CARTESIAN_POINT ( 'NONE',  ( 25.56776753627341137, -17.11417227705152655, 1.000000000000000000 ) ) ;
#11101 = ORIENTED_EDGE ( 'NONE', *, *, #12601, .F. ) ;
#11102 = CARTESIAN_POINT ( 'NONE',  ( 5.377543748152550762, 6.139290821770327256, -5.151476664237414127 ) ) ;
#11103 = SHAPE_REPRESENTATION_RELATIONSHIP ( 'NONE' , 'NONE' ,  #27351, #9968 ) ;
#11104 = ORIENTED_EDGE ( 'NONE', *, *, #3986, .T. ) ;
#11105 = VERTEX_POINT ( 'NONE', #25907 ) ;
#11106 = CARTESIAN_POINT ( 'NONE',  ( 24.36752972617610524, -17.44836528598952796, -1.442218785864573416 ) ) ;
#11107 = CONTEXT_DEPENDENT_SHAPE_REPRESENTATION ( #9038, #20473 ) ;
#11109 = VERTEX_POINT ( 'NONE', #18677 ) ;
#11108 = FACE_OUTER_BOUND ( 'NONE', #4838, .T. ) ;
#11110 = B_SPLINE_CURVE_WITH_KNOTS ( 'NONE', 3,
 ( #6361, #22103, #21754, #11900, #8726, #19086, #31961, #13873, #26463, #16745, #24574, #14218 ),
 .UNSPECIFIED., .F., .F.,
 ( 4, 2, 2, 2, 2, 4 ),
 ( 4.661736504953698139E-16, 0.001666179614552203668, 0.002499269421828077386, 0.002915814325466020100, 0.003124086777284991890, 0.003332359229103963247 ),
 .UNSPECIFIED. ) ;
#11111 = ORIENTED_EDGE ( 'NONE', *, *, #16629, .T. ) ;
#11112 = CARTESIAN_POINT ( 'NONE',  ( 1.265925305626668392E-16, 1.476463073999636277, 4.787500056513372293 ) ) ;
#11113 = ORIENTED_EDGE ( 'NONE', *, *, #1396, .T. ) ;
#11114 = CARTESIAN_POINT ( 'NONE',  ( 0.1574692253521047247, 2.132217800984971934, -10.40622129948815910 ) ) ;
#11116 = ORIENTED_EDGE ( 'NONE', *, *, #30216, .T. ) ;
#11115 = CARTESIAN_POINT ( 'NONE',  ( 47.88515715257229033, -3.977125052580343656, -1.169950612145078450 ) ) ;
#11117 = DIRECTION ( 'NONE',  ( -1.000000000000000000, 0.000000000000000000, 0.000000000000000000 ) ) ;
#11118 = DIRECTION ( 'NONE',  ( -0.000000000000000000, -1.000000000000000000, -0.000000000000000000 ) ) ;
#11119 = CARTESIAN_POINT ( 'NONE',  ( 2.970200481228956413, 4.917777846811763887, -7.729547851462088559 ) ) ;
#11120 = CARTESIAN_POINT ( 'NONE',  ( 108.0585218215646677, -18.91206178857411402, 4.613303170613168191 ) ) ;
#11121 = CARTESIAN_POINT ( 'NONE',  ( -3.900050800000000706, -2.983565686104819648, -0.3135853898029605791 ) ) ;
#11122 = CARTESIAN_POINT ( 'NONE',  ( 41.92799935455844462, -21.01937708447562159, -4.522129901861164925 ) ) ;
#11123 = CARTESIAN_POINT ( 'NONE',  ( 85.13967574987859166, -6.881122605236785539, -0.8105612905604291374 ) ) ;
#11124 = DIRECTION ( 'NONE',  ( -7.023442172597837140E-17, -0.8191520442889893561, -0.5735764363510496011 ) ) ;
#11125 = EDGE_CURVE ( 'NONE', #12969, #13197, #9222, .T. ) ;
#11126 = EDGE_CURVE ( 'NONE', #15594, #7501, #18868, .T. ) ;
#11127 = DIRECTION ( 'NONE',  ( -0.000000000000000000, -0.3746065934159164001, 0.9271838545667856479 ) ) ;
#11128 = CYLINDRICAL_SURFACE ( 'NONE', #17704, 8.749000000000002331 ) ;
#11129 = CARTESIAN_POINT ( 'NONE',  ( 0.7212198416532932255, -6.922088825881659524, -5.676697589997751869 ) ) ;
#11130 = DIRECTION ( 'NONE',  ( 1.000000000000000000, -0.000000000000000000, -0.000000000000000000 ) ) ;
#11131 = CARTESIAN_POINT ( 'NONE',  ( -32.85000000000000142, -10.96966150227469328, -1.499999999999999556 ) ) ;
#11132 = CARTESIAN_POINT ( 'NONE',  ( -2.212550801365593234, 3.368539882008727115, 1.828967928396026954 ) ) ;
#11133 = VERTEX_POINT ( 'NONE', #29068 ) ;
#11134 = CARTESIAN_POINT ( 'NONE',  ( -7.750050800000000351, -0.9222479816126459840, -3.113457007523259268 ) ) ;
#11135 = DIRECTION ( 'NONE',  ( 1.000000000000000000, -0.000000000000000000, -0.000000000000000000 ) ) ;
#11136 = DIRECTION ( 'NONE',  ( 1.000000000000000000, 0.000000000000000000, 0.000000000000000000 ) ) ;
#11137 = CARTESIAN_POINT ( 'NONE',  ( -41.24084109483541027, -14.66809682074130627, 5.561913827905596186 ) ) ;
#11138 = ORIENTED_EDGE ( 'NONE', *, *, #28600, .F. ) ;
#11139 = LINE ( 'NONE', #26389, #23634 ) ;
#11140 = ADVANCED_BREP_SHAPE_REPRESENTATION ( '', ( #21237, #2865 ), #13509 ) ;
#11141 = VERTEX_POINT ( 'NONE', #29722 ) ;
#11142 = CARTESIAN_POINT ( 'NONE',  ( 1.058168406056548605, -9.473510274387203722, 1.499999999999999778 ) ) ;
#11143 = DATE_AND_TIME ( #18855, #7681 ) ;
#11144 = CARTESIAN_POINT ( 'NONE',  ( 40.87951250943078918, -6.073635182929082887, 4.275175681039489639 ) ) ;
#11145 = EDGE_CURVE ( 'NONE', #17732, #23082, #27035, .T. ) ;
#11146 = CARTESIAN_POINT ( 'NONE',  ( -56.32245079178366609, 0.2385709902195854437, -1.445874915207051581 ) ) ;
#11147 = CARTESIAN_POINT ( 'NONE',  ( 24.34295195635817777, -17.38504247893911270, -1.375705049358364684 ) ) ;
#11148 = ORIENTED_EDGE ( 'NONE', *, *, #12575, .F. ) ;
#11149 = FACE_OUTER_BOUND ( 'NONE', #24082, .T. ) ;
#11150 = CARTESIAN_POINT ( 'NONE',  ( -31.18783180709124636, -21.43932300455417916, 1.500000000000000000 ) ) ;
#11151 = CARTESIAN_POINT ( 'NONE',  ( 109.3153218317886513, 19.84491634189289400, 3.222654707407430319 ) ) ;
#11152 = EDGE_CURVE ( 'NONE', #22574, #9919, #23133, .T. ) ;
#11154 = ORIENTED_EDGE ( 'NONE', *, *, #10921, .F. ) ;
#11153 = CARTESIAN_POINT ( 'NONE',  ( -4.013969549054180728E-16, -4.681538312723511730, -0.8254815157535732029 ) ) ;
#11155 = CARTESIAN_POINT ( 'NONE',  ( -3.612550801365593589, -1.828967928396026510, 3.368539882008728004 ) ) ;
#11156 = CARTESIAN_POINT ( 'NONE',  ( 108.1156589233279419, 18.82219444680297116, 4.414476567109417715 ) ) ;
#11157 = CARTESIAN_POINT ( 'NONE',  ( 18.75828436641558028, -5.879118399717574661, -3.993434336035625254 ) ) ;
#11158 = ORIENTED_EDGE ( 'NONE', *, *, #5307, .T. ) ;
#11159 = ORIENTED_EDGE ( 'NONE', *, *, #5741, .F. ) ;
#11160 = EDGE_CURVE ( 'NONE', #22902, #6888, #15738, .T. ) ;
#11161 = DIRECTION ( 'NONE',  ( 0.000000000000000000, 0.000000000000000000, -1.000000000000000000 ) ) ;
#11162 = CARTESIAN_POINT ( 'NONE',  ( 0.5640492184727913250, -3.576105523038064504, 8.844377740319870895 ) ) ;
#11163 = PLANE ( 'NONE',  #25288 ) ;
#11164 = CARTESIAN_POINT ( 'NONE',  ( 13.65718777917708415, -19.09288791508985028, 4.522129901861159595 ) ) ;
#11165 = EDGE_CURVE ( 'NONE', #14980, #26351, #11495, .T. ) ;
#11166 = CARTESIAN_POINT ( 'NONE',  ( 25.43628654896618357, -17.54453578616538323, 1.025168090788791009 ) ) ;
#11167 = ORIENTED_EDGE ( 'NONE', *, *, #7888, .T. ) ;
#11168 = CARTESIAN_POINT ( 'NONE',  ( -8.454531657079160212, 1.545410377633947174, -2.846291840500173365 ) ) ;
#11169 = AXIS2_PLACEMENT_3D ( 'NONE', #939, #8602, #18640 ) ;
#11170 = CARTESIAN_POINT ( 'NONE',  ( -57.83188187760648447, -3.114258703770785619, 5.486698823786428925 ) ) ;
#11171 = EDGE_CURVE ( 'NONE', #16287, #27971, #1321, .T. ) ;
#11172 = CARTESIAN_POINT ( 'NONE',  ( -4.487550801365593145, -2.752080473201636845, 2.228590825266444586 ) ) ;
#11173 = DIRECTION ( 'NONE',  ( -0.000000000000000000, -0.000000000000000000, -1.000000000000000000 ) ) ;
#11174 = DIRECTION ( 'NONE',  ( 0.000000000000000000, 0.1045284632676536235, 0.9945218953682734009 ) ) ;
#11175 = VERTEX_POINT ( 'NONE', #24009 ) ;
#11176 = CYLINDRICAL_SURFACE ( 'NONE', #9206, 2.999999999999999112 ) ;
#11177 = ORIENTED_EDGE ( 'NONE', *, *, #6, .T. ) ;
#11178 = CALENDAR_DATE ( 2026, 6, 10 ) ;
#11179 = EDGE_CURVE ( 'NONE', #18045, #29668, #30094, .T. ) ;
#11180 = CARTESIAN_POINT ( 'NONE',  ( 18.75839033845637971, -5.877933844985113510, 3.995336671754854407 ) ) ;
#11181 = CARTESIAN_POINT ( 'NONE',  ( 13.72001175370881221, -13.92748696968235578, -1.000000000000000000 ) ) ;
#11182 = AXIS2_PLACEMENT_3D ( 'NONE', #29012, #1078, #31508 ) ;
#11183 = ORIENTED_EDGE ( 'NONE', *, *, #171, .T. ) ;
#11184 = CARTESIAN_POINT ( 'NONE',  ( 0.000000000000000000, 8.264486777890107660, -4.472189673936814991 ) ) ;
#11185 = EDGE_CURVE ( 'NONE', #28142, #3782, #13697, .T. ) ;
#11186 = ORIENTED_EDGE ( 'NONE', *, *, #31875, .T. ) ;
#11187 = EDGE_LOOP ( 'NONE', ( #3093, #6461, #17062 ) ) ;
#11188 = DIRECTION ( 'NONE',  ( 0.000000000000000000, 0.000000000000000000, -1.000000000000000000 ) ) ;
#11189 = CARTESIAN_POINT ( 'NONE',  ( -3.012550801365593500, 3.368539882008727115, 1.828967928396027176 ) ) ;
#11190 = CARTESIAN_POINT ( 'NONE',  ( 13.10266514559113205, -14.23637329403208263, 1.500000000000000000 ) ) ;
#11191 = CARTESIAN_POINT ( 'NONE',  ( 1.997925886398103978, -1.624855788928872391, -1.500000000000000000 ) ) ;
#11192 = TOROIDAL_SURFACE ( 'NONE', #4256, 301.4345239564033250, 5.000000000000000888 ) ;
#11194 = ORIENTED_EDGE ( 'NONE', *, *, #26632, .F. ) ;
#11193 = LINE ( 'NONE', #23752, #18182 ) ;
#11195 = CARTESIAN_POINT ( 'NONE',  ( -7.287550801365593856, 2.752080473201636845, -2.228590825266444142 ) ) ;
#11196 = CARTESIAN_POINT ( 'NONE',  ( 13.32340444539593349, 6.787188996065617985, 1.500000000000829781 ) ) ;
#11197 = CARTESIAN_POINT ( 'NONE',  ( 34.48223484310472031, 0.5000000000000000000, -2.552009564962229859 ) ) ;
#11199 = EDGE_CURVE ( 'NONE', #14830, #15097, #14473, .T. ) ;
#11198 = CARTESIAN_POINT ( 'NONE',  ( 21.48500000136559507, 2.892927487894327410, -1.570731468192931635 ) ) ;
#11201 = ORIENTED_EDGE ( 'NONE', *, *, #12704, .T. ) ;
#11200 = LINE ( 'NONE', #18573, #20863 ) ;
#11202 = EDGE_CURVE ( 'NONE', #11273, #20542, #1135, .T. ) ;
#11203 = CARTESIAN_POINT ( 'NONE',  ( -23.54713438638086842, 3.998227953278294944, 2.146185852361370383 ) ) ;
#11204 = CARTESIAN_POINT ( 'NONE',  ( 21.04750000273118715, 0.7685399846772009713, -2.594547506269381909 ) ) ;
#11205 = EDGE_CURVE ( 'NONE', #6245, #15051, #26875, .T. ) ;
#11206 = CARTESIAN_POINT ( 'NONE',  ( -17.81720712383456728, 7.575660699117379160, 1.500000000000110578 ) ) ;
#11207 = CIRCLE ( 'NONE', #6402, 2.999999999999999556 ) ;
#11208 = CARTESIAN_POINT ( 'NONE',  ( 18.73307111251037327, -6.160951975821718385, -3.539148371795089787 ) ) ;
#11209 = CARTESIAN_POINT ( 'NONE',  ( 0.000000000000000000, 0.000000000000000000, -1.500000000000000000 ) ) ;
#11210 = CARTESIAN_POINT ( 'NONE',  ( 3.499999999999999556, 4.561279057474412646, 4.271385531633187682 ) ) ;
#11211 = AXIS2_PLACEMENT_3D ( 'NONE', #30842, #2247, #12745 ) ;
#11212 = B_SPLINE_CURVE_WITH_KNOTS ( 'NONE', 3,
 ( #11926, #29970, #7236, #19609, #32650, #27776, #14389, #4888, #9729, #17073 ),
 .UNSPECIFIED., .F., .F.,
 ( 4, 2, 2, 2, 4 ),
 ( 1.968338519013083730E-07, 0.0005467927057105487470, 0.001093388577569196071, 0.001639984449427843395, 0.002186580321286489634 ),
 .UNSPECIFIED. ) ;
#11213 = PLANE ( 'NONE',  #8169 ) ;
#11214 = CARTESIAN_POINT ( 'NONE',  ( -4.837550801365592790, 3.675193018007247403, -1.088641768524161391 ) ) ;
#11215 = ORIENTED_EDGE ( 'NONE', *, *, #5221, .T. ) ;
#11216 = EDGE_CURVE ( 'NONE', #16936, #18451, #3807, .T. ) ;
#11217 = AXIS2_PLACEMENT_3D ( 'NONE', #1939, #20489, #12605 ) ;
#11218 = FACE_OUTER_BOUND ( 'NONE', #30989, .T. ) ;
#11219 = CARTESIAN_POINT ( 'NONE',  ( 5.885541615502094537, 8.193643496140877502, -1.821712961073262527 ) ) ;
#11221 = CARTESIAN_POINT ( 'NONE',  ( 4.749760686538667009, 6.940565734314597002, 4.007137495034836405 ) ) ;
#11220 = DIRECTION ( 'NONE',  ( 8.574039729943018344E-17, 1.000000000000000000, 0.000000000000000000 ) ) ;
#11222 = ORIENTED_EDGE ( 'NONE', *, *, #5279, .T. ) ;
#11223 = DIRECTION ( 'NONE',  ( 1.000000000000000000, 0.000000000000000000, 0.000000000000000000 ) ) ;
#11224 = ORIENTED_EDGE ( 'NONE', *, *, #12017, .F. ) ;
#11225 = CARTESIAN_POINT ( 'NONE',  ( -10.00000000000000000, 0.000000000000000000, 0.000000000000000000 ) ) ;
#11227 = ORIENTED_EDGE ( 'NONE', *, *, #17335, .F. ) ;
#11226 = CARTESIAN_POINT ( 'NONE',  ( 107.9622325421415212, 20.81773585569407459, -1.491740999229417941 ) ) ;
#11228 = ORIENTED_EDGE ( 'NONE', *, *, #2151, .T. ) ;
#11229 = CARTESIAN_POINT ( 'NONE',  ( 10.00000000000000000, 4.467071865485493731, -1.625881193364653088 ) ) ;
#11230 = VECTOR ( 'NONE', #6829, 1000.000000000000114 ) ;
#11231 = EDGE_CURVE ( 'NONE', #1551, #6094, #26041, .T. ) ;
#11232 = AXIS2_PLACEMENT_3D ( 'NONE', #9679, #12535, #32606 ) ;
#11233 = CARTESIAN_POINT ( 'NONE',  ( -18.35000000000000142, -10.96966150227469505, 4.000000000000000000 ) ) ;
#11235 = ORIENTED_EDGE ( 'NONE', *, *, #20631, .F. ) ;
#11234 = CARTESIAN_POINT ( 'NONE',  ( 107.8941086082324432, 17.58851487277170023, 3.071072500904354463 ) ) ;
#11236 = DIRECTION ( 'NONE',  ( -3.028893931825485746E-17, -8.673617379884035472E-16, -1.000000000000000000 ) ) ;
#11237 = CIRCLE ( 'NONE', #24036, 0.4500000000000025646 ) ;
#11238 = DIRECTION ( 'NONE',  ( 0.000000000000000000, 1.000000000000000000, 0.000000000000000000 ) ) ;
#11239 = CARTESIAN_POINT ( 'NONE',  ( 3.499999999999999556, 4.058600654062849422, 7.468451026206211374 ) ) ;
#11240 = EDGE_CURVE ( 'NONE', #5778, #7501, #11386, .T. ) ;
#11242 = CARTESIAN_POINT ( 'NONE',  ( 7.650166299106958334, -9.403575859901817324, -1.000000000000000000 ) ) ;
#11241 = VECTOR ( 'NONE', #4631, 1000.000000000000000 ) ;
#11243 = CARTESIAN_POINT ( 'NONE',  ( 107.9811197705840016, -17.79749150983783323, -4.359573227107783389 ) ) ;
#11244 = EDGE_CURVE ( 'NONE', #24728, #29938, #7640, .T. ) ;
#11245 = CYLINDRICAL_SURFACE ( 'NONE', #16724, 5.010000000000000675 ) ;
#11246 = AXIS2_PLACEMENT_3D ( 'NONE', #31903, #6464, #6651 ) ;
#11247 = CARTESIAN_POINT ( 'NONE',  ( 2.864531019710239601, 3.575186956654106574, -8.868883597856958900 ) ) ;
#11248 = CARTESIAN_POINT ( 'NONE',  ( 69.07074218556155643, -6.116471746203279380, 3.993434826126005088 ) ) ;
#11249 = CARTESIAN_POINT ( 'NONE',  ( -3.300050800000000173, -0.3135853898029607456, 2.983565686104819648 ) ) ;
#11250 = CARTESIAN_POINT ( 'NONE',  ( 0.000000000000000000, -4.709950686174546597, -9.884132761439110126 ) ) ;
#11251 = ORIENTED_EDGE ( 'NONE', *, *, #32353, .F. ) ;
#11252 = CARTESIAN_POINT ( 'NONE',  ( 0.6791197464446651066, 0.5477823182330875396, 9.138998021039181907 ) ) ;
#11253 = AXIS2_PLACEMENT_3D ( 'NONE', #4834, #25560, #30777 ) ;
#11254 = AXIS2_PLACEMENT_3D ( 'NONE', #33041, #26020, #3280 ) ;
#11255 = CARTESIAN_POINT ( 'NONE',  ( 10.55147673363119232, 2.376879293651063652, 4.116875700062091248 ) ) ;
#11256 = CARTESIAN_POINT ( 'NONE',  ( 25.75999999999999801, -2.208672634433321348E-15, 0.000000000000000000 ) ) ;
#11257 = VERTEX_POINT ( 'NONE', #9972 ) ;
#11259 = EDGE_CURVE ( 'NONE', #4825, #21913, #33048, .T. ) ;
#11258 = VECTOR ( 'NONE', #26410, 1000.000000000000000 ) ;
#11260 = CC_DESIGN_DATE_AND_TIME_ASSIGNMENT ( #3673, #8355, ( #23132 ) ) ;
#11261 = AXIS2_PLACEMENT_3D ( 'NONE', #2159, #30263, #25554 ) ;
#11262 =( BOUNDED_CURVE ( )  B_SPLINE_CURVE ( 2, ( #8999, #19400, #32285, #19215, #27414, #27066, #14517, #11528, #21724, #21879, #9346 ),
 .UNSPECIFIED., .F., .F. ) 
 B_SPLINE_CURVE_WITH_KNOTS ( ( 3, 2, 2, 2, 2, 3 ),
 ( 0.2966116191895003529, 0.2999999999999999889, 0.3250000000000000111, 0.3499999999999999778, 0.3750000000000000000, 0.3966116191895003862 ),
 .UNSPECIFIED. ) 
 CURVE ( )  GEOMETRIC_REPRESENTATION_ITEM ( )  RATIONAL_B_SPLINE_CURVE ( ( 0.9821626249036858880, 0.9896829947469992783, 1.000000000000000000, 0.9238795325112867385, 1.000000000000000000, 0.9238795325112867385, 1.000000000000000000, 0.9238795325112867385, 1.000000000000000000, 0.9341965377642874602, 0.9821626249036858880 ) ) 
 REPRESENTATION_ITEM ( '' )  );
#11263 = DIRECTION ( 'NONE',  ( 1.000000000000000000, -0.000000000000000000, -0.000000000000000000 ) ) ;
#11264 = CARTESIAN_POINT ( 'NONE',  ( 16.10106094948405797, 19.71584668020019038, -5.396302277755718357 ) ) ;
#11265 = ORIENTED_EDGE ( 'NONE', *, *, #11610, .F. ) ;
#11266 = CARTESIAN_POINT ( 'NONE',  ( 7.064632951172269415, 7.135485519862065473, -5.064320921489749772 ) ) ;
#11267 =( NAMED_UNIT ( * ) SI_UNIT ( $, .STERADIAN. ) SOLID_ANGLE_UNIT ( ) );
#11268 = ORIENTED_EDGE ( 'NONE', *, *, #431, .T. ) ;
#11269 = VERTEX_POINT ( 'NONE', #30228 ) ;
#11270 = CARTESIAN_POINT ( 'NONE',  ( 6.038145077921539539, 3.316258947000968238, -7.799182446117161049 ) ) ;
#11271 = CALENDAR_DATE ( 2026, 6, 10 ) ;
#11273 = VERTEX_POINT ( 'NONE', #10121 ) ;
#11272 = CARTESIAN_POINT ( 'NONE',  ( 23.24290772321994325, 0.1310194482076003919, 2.499999999999998668 ) ) ;
#11274 = ORIENTED_EDGE ( 'NONE', *, *, #8283, .T. ) ;
#11275 = DIRECTION ( 'NONE',  ( 0.000000000000000000, -1.000000000000000000, 0.000000000000000000 ) ) ;
#11276 = EDGE_CURVE ( 'NONE', #29777, #12969, #25182, .T. ) ;
#11277 = B_SPLINE_CURVE_WITH_KNOTS ( 'NONE', 3,
 ( #32202, #29686, #29179, #13933, #6765, #11119, #16305, #21656 ),
 .UNSPECIFIED., .F., .F.,
 ( 4, 2, 2, 4 ),
 ( 2.152606690539618764E-07, 0.001262065476468824396, 0.001892990584368709666, 0.002523915692268595152 ),
 .UNSPECIFIED. ) ;
#11278 = ORIENTED_EDGE ( 'NONE', *, *, #24510, .F. ) ;
#11279 = CARTESIAN_POINT ( 'NONE',  ( 107.5617723795404999, -18.98359893170737323, 4.522129901861158707 ) ) ;
#11280 = DIRECTION ( 'NONE',  ( -3.623545766764295357E-17, -0.4226182617407088782, 0.9063077870366454958 ) ) ;
#11282 = ORIENTED_EDGE ( 'NONE', *, *, #18151, .F. ) ;
#11281 = CARTESIAN_POINT ( 'NONE',  ( 41.34386496146564838, -3.886814715717100022, -0.07017451552238240797 ) ) ;
#11283 = DIRECTION ( 'NONE',  ( 1.000000000000000000, 0.000000000000000000, 0.000000000000000000 ) ) ;
#11284 = CARTESIAN_POINT ( 'NONE',  ( 6.530491241813343173, -0.6236753264481147419, 8.637950316517743587 ) ) ;
#11285 = EDGE_CURVE ( 'NONE', #5334, #17030, #4634, .T. ) ;
#11286 = CIRCLE ( 'NONE', #4866, 5.009999999999999787 ) ;
#11287 = AXIS2_PLACEMENT_3D ( 'NONE', #18906, #5842, #26090 ) ;
#11288 = CARTESIAN_POINT ( 'NONE',  ( 101.8535835026724925, -4.790122518509368099, 2.790665559886620795 ) ) ;
#11289 = FACE_OUTER_BOUND ( 'NONE', #25885, .T. ) ;
#11290 = VECTOR ( 'NONE', #838, 1000.000000000000114 ) ;
#11291 = DIRECTION ( 'NONE',  ( 0.000000000000000000, 1.000000000000000000, 0.000000000000000000 ) ) ;
#11292 = VECTOR ( 'NONE', #2956, 1000.000000000000000 ) ;
#11293 = VECTOR ( 'NONE', #33013, 1000.000000000000000 ) ;
#11294 = CARTESIAN_POINT ( 'NONE',  ( -3.671333707197877479E-13, 1.999317321091317545, -10.76487093102143433 ) ) ;
#11295 = DIRECTION ( 'NONE',  ( -1.000000000000000000, 0.000000000000000000, 0.000000000000000000 ) ) ;
#11296 = FACE_OUTER_BOUND ( 'NONE', #7465, .T. ) ;
#11297 = AXIS2_PLACEMENT_3D ( 'NONE', #28647, #8075, #15272 ) ;
#11298 = CIRCLE ( 'NONE', #20894, 0.5000000000000004441 ) ;
#11299 = CARTESIAN_POINT ( 'NONE',  ( 25.75999999999999801, -5.000000000000005329, 6.123233995736771213E-16 ) ) ;
#11300 = FACE_OUTER_BOUND ( 'NONE', #20115, .T. ) ;
#11301 = CARTESIAN_POINT ( 'NONE',  ( 107.6244361484700534, 18.92564684440470657, -5.076485033663518109 ) ) ;
#11302 = CARTESIAN_POINT ( 'NONE',  ( -33.00121834596181714, -0.06979899340500209104, 3.000000000000004441 ) ) ;
#11303 = CYLINDRICAL_SURFACE ( 'NONE', #8111, 2.499999999999997780 ) ;
#11304 = CARTESIAN_POINT ( 'NONE',  ( -2.162550801365593856, 2.228590825266444142, 2.752080473201636845 ) ) ;
#11305 = ORIENTED_EDGE ( 'NONE', *, *, #22001, .F. ) ;
#11306 = CARTESIAN_POINT ( 'NONE',  ( -5.600050800000000883, -2.331437884370912705, 1.887961173149512062 ) ) ;
#11307 = AXIS2_PLACEMENT_3D ( 'NONE', #5225, #15576, #23282 ) ;
#11308 = DIRECTION ( 'NONE',  ( -1.000000000000000000, 0.000000000000000000, 0.000000000000000000 ) ) ;
#11309 = CARTESIAN_POINT ( 'NONE',  ( -5.312942406915326821, -3.366872799099910998E-15, -3.000000000000000000 ) ) ;
#11310 = CARTESIAN_POINT ( 'NONE',  ( 7.461135470892689803, -4.560857689779278523, 1.000000000000000000 ) ) ;
#11311 = ORIENTED_EDGE ( 'NONE', *, *, #15583, .F. ) ;
#11312 = CARTESIAN_POINT ( 'NONE',  ( -7.306376978575949366, -0.1572233378491242062, 2.999999999999999556 ) ) ;
#11313 = CIRCLE ( 'NONE', #1729, 0.4500000000000012879 ) ;
#11314 = ORIENTED_EDGE ( 'NONE', *, *, #32445, .F. ) ;
#11315 = CARTESIAN_POINT ( 'NONE',  ( 0.6388753366353405738, -7.663106119046291020, 1.499999999999999556 ) ) ;
#11316 = APPROVAL_ROLE ( '' ) ;
#11317 = CARTESIAN_POINT ( 'NONE',  ( 18.84933643290985827, -4.861339035673776898, 4.155404940064419961 ) ) ;
#11318 = TOROIDAL_SURFACE ( 'NONE', #15591, 6.818740222761507042, 0.5000000000000000000 ) ;
#11319 = ADVANCED_FACE ( 'NONE', ( #20341 ), #12146, .F. ) ;
#11320 = EDGE_CURVE ( 'NONE', #28727, #11796, #6885, .T. ) ;
#11321 = CIRCLE ( 'NONE', #2267, 4.000000000000001776 ) ;
#11322 = FACE_OUTER_BOUND ( 'NONE', #31996, .T. ) ;
#11323 = LINE ( 'NONE', #26399, #3801 ) ;
#11324 = CARTESIAN_POINT ( 'NONE',  ( 2.589203020517547138, 5.222514179739501827, 8.895471158038665394 ) ) ;
#11325 = EDGE_CURVE ( 'NONE', #17664, #30219, #4452, .T. ) ;
#11326 = EDGE_LOOP ( 'NONE', ( #25422, #17794, #24667, #555 ) ) ;
#11327 = LINE ( 'NONE', #18864, #15156 ) ;
#11328 = CARTESIAN_POINT ( 'NONE',  ( -31.52072750637464083, 0.5000000000000022204, 1.500000000000000000 ) ) ;
#11329 = CARTESIAN_POINT ( 'NONE',  ( 6.524595395369783724, -7.902859683906637400, 3.538595500939559990 ) ) ;
#11331 = ORIENTED_EDGE ( 'NONE', *, *, #20079, .F. ) ;
#11330 = DIRECTION ( 'NONE',  ( 0.000000000000000000, -0.9659258262890674240, 0.2588190451025241257 ) ) ;
#11332 = VECTOR ( 'NONE', #16248, 1000.000000000000000 ) ;
#11333 = CARTESIAN_POINT ( 'NONE',  ( -3.462550801365593678, -3.521866450007987037, -0.3701630799359323931 ) ) ;
#11334 = CARTESIAN_POINT ( 'NONE',  ( 17.32050807568873552, 10.00000000000002309, -4.612695725900422872 ) ) ;
#11335 = CARTESIAN_POINT ( 'NONE',  ( -31.57659242536668742, -27.93932300454937590, -0.9999999999999981126 ) ) ;
#11336 = CIRCLE ( 'NONE', #6532, 8.750000000000000000 ) ;
#11337 = VECTOR ( 'NONE', #5109, 999.9999999999998863 ) ;
#11338 = CIRCLE ( 'NONE', #23117, 4.000000000000001776 ) ;
#11339 = CARTESIAN_POINT ( 'NONE',  ( -31.68476024375366862, -21.93625144121646642, 1.063946347602459319 ) ) ;
#11340 =( BOUNDED_SURFACE ( )  B_SPLINE_SURFACE ( 1, 3, ( 
 ( #26821, #28569, #6412, #6601 ),
 ( #1083, #16798, #16610, #3943 ) ),
 .UNSPECIFIED., .F., .F., .F. ) 
 B_SPLINE_SURFACE_WITH_KNOTS ( ( 2, 2 ),
 ( 4, 4 ),
 ( 0.000000000000000000, 1.000000000000000000 ),
 ( 0.000000000000000000, 1.000000000000000000 ),
 .UNSPECIFIED. ) 
 GEOMETRIC_REPRESENTATION_ITEM ( )  RATIONAL_B_SPLINE_SURFACE ( (
 ( 1.000000000000000000, 0.9321687722090974404, 0.9321687722090974404, 1.000000000000000000),
 ( 1.000000000000000000, 0.9321687722090974404, 0.9321687722090974404, 1.000000000000000000) ) ) 
 REPRESENTATION_ITEM ( '' )  SURFACE ( )  );
#11342 = VECTOR ( 'NONE', #26224, 1000.000000000000227 ) ;
#11341 = CYLINDRICAL_SURFACE ( 'NONE', #1175, 2.499999999999997780 ) ;
#11343 = FACE_OUTER_BOUND ( 'NONE', #6323, .T. ) ;
#11344 = CARTESIAN_POINT ( 'NONE',  ( 12.44989959798868817, 0.4999999999999998890, 13.00000000000004441 ) ) ;
#11345 = ORIENTED_EDGE ( 'NONE', *, *, #23486, .F. ) ;
#11346 = CIRCLE ( 'NONE', #22570, 4.000000000000001776 ) ;
#11347 = CARTESIAN_POINT ( 'NONE',  ( -7.000050800000001239, 0.000000000000000000, 0.000000000000000000 ) ) ;
#11348 = ORIENTED_EDGE ( 'NONE', *, *, #24095, .F. ) ;
#11349 = CIRCLE ( 'NONE', #1769, 5.009999999999999787 ) ;
#11350 = CARTESIAN_POINT ( 'NONE',  ( 24.80306213860490061, -17.49230408913781787, -1.500000000000000000 ) ) ;
#11351 = CARTESIAN_POINT ( 'NONE',  ( -57.40374817251313999, -2.616512360834425621, 5.500000000000000000 ) ) ;
#11352 = CARTESIAN_POINT ( 'NONE',  ( -3.987550801365593145, 3.521866450007987037, 0.3701630799359328372 ) ) ;
#11353 = LINE ( 'NONE', #10678, #6040 ) ;
#11354 = CARTESIAN_POINT ( 'NONE',  ( 85.10567447696165289, -6.328783234401409885, 2.184955974440073945 ) ) ;
#11355 = ORIENTED_EDGE ( 'NONE', *, *, #33060, .F. ) ;
#11356 = CARTESIAN_POINT ( 'NONE',  ( 107.7536796087345294, 16.80655079293032017, -1.379243061950440108 ) ) ;
#11357 = VECTOR ( 'NONE', #14188, 1000.000000000000000 ) ;
#11358 = EDGE_CURVE ( 'NONE', #2704, #27064, #20984, .T. ) ;
#11359 = VECTOR ( 'NONE', #23348, 1000.000000000000114 ) ;
#11360 = ORIENTED_EDGE ( 'NONE', *, *, #11405, .T. ) ;
#11362 = VECTOR ( 'NONE', #5536, 1000.000000000000000 ) ;
#11361 = PERSON_AND_ORGANIZATION ( #6766, #25292 ) ;
#11363 = CARTESIAN_POINT ( 'NONE',  ( 40.88398506880648142, -6.895404553204455667, 3.995336175096711795 ) ) ;
#11364 = AXIS2_PLACEMENT_3D ( 'NONE', #7351, #2873, #18204 ) ;
#11365 = CIRCLE ( 'NONE', #7621, 4.000000000000001776 ) ;
#11366 = DIRECTION ( 'NONE',  ( -7.023442172597800162E-17, -0.8191520442889850262, -0.5735764363510558184 ) ) ;
#11367 = EDGE_LOOP ( 'NONE', ( #10573, #25410, #24183, #28602 ) ) ;
#11368 = CARTESIAN_POINT ( 'NONE',  ( 34.55406472725060496, 0.5174497483512505713, -3.046515352619024508 ) ) ;
#11370 = VERTEX_POINT ( 'NONE', #17489 ) ;
#11369 = VECTOR ( 'NONE', #207, 1000.000000000000000 ) ;
#11371 = VERTEX_POINT ( 'NONE', #27859 ) ;
#11372 = AXIS2_PLACEMENT_3D ( 'NONE', #23959, #16286, #22256 ) ;
#11373 = CARTESIAN_POINT ( 'NONE',  ( -4.013969549054187630E-16, -4.681538312723522388, 0.8254815157535098091 ) ) ;
#11374 = CARTESIAN_POINT ( 'NONE',  ( -2.812550801365592879, -1.828967928396026732, 3.368539882008728004 ) ) ;
#11375 = CARTESIAN_POINT ( 'NONE',  ( 22.73500000000000298, -0.2613211581691358698, -2.486304738420681559 ) ) ;
#11376 = CIRCLE ( 'NONE', #184, 0.5000000000000004441 ) ;
#11377 = CARTESIAN_POINT ( 'NONE',  ( 4.749760686538667009, 7.530955069117551304, -2.741043480754851380 ) ) ;
#11379 = ORIENTED_EDGE ( 'NONE', *, *, #14282, .F. ) ;
#11378 = CARTESIAN_POINT ( 'NONE',  ( 7.249760686538667009, 3.748318449932404484, -7.906491560603625679 ) ) ;
#11380 = CARTESIAN_POINT ( 'NONE',  ( -6.387550801365593500, 3.521866450007987037, 0.3701630799359328372 ) ) ;
#11381 = CARTESIAN_POINT ( 'NONE',  ( 19.03564543760834482, 14.58476759512525334, 1.500000000000000000 ) ) ;
#11382 = CARTESIAN_POINT ( 'NONE',  ( 11.72329880919066980, -20.06223657121697812, 1.500000000001569189 ) ) ;
#11383 = CARTESIAN_POINT ( 'NONE',  ( 108.0981717737601997, -19.48301123670199075, -2.289311975395072363 ) ) ;
#11385 = ORIENTED_EDGE ( 'NONE', *, *, #16435, .F. ) ;
#11384 = LINE ( 'NONE', #13216, #24586 ) ;
#11386 = CIRCLE ( 'NONE', #15660, 11.00000000000000000 ) ;
#11387 = AXIS2_PLACEMENT_3D ( 'NONE', #3488, #18661, #5960 ) ;
#11388 = CARTESIAN_POINT ( 'NONE',  ( 22.23500000273118715, 2.486304738420679783, -0.2613211581691337604 ) ) ;
#11389 = CIRCLE ( 'NONE', #8196, 8.500000000000000000 ) ;
#11390 = AXIS2_PLACEMENT_3D ( 'NONE', #12166, #17673, #7321 ) ;
#11391 = CARTESIAN_POINT ( 'NONE',  ( 6.530491482054475050, -0.8857639883442328665, -8.615020591497811964 ) ) ;
#11392 = CARTESIAN_POINT ( 'NONE',  ( 101.8082167159056581, -4.136852074903159426, -3.842005631892731365 ) ) ;
#11393 = CARTESIAN_POINT ( 'NONE',  ( -4.179222253013961996, -3.233748670362141198, -1.499999999999999112 ) ) ;
#11394 = CARTESIAN_POINT ( 'NONE',  ( 0.5704039292223109792, -6.124150562935243514, -7.316743080999502880 ) ) ;
#11395 = EDGE_CURVE ( 'NONE', #6345, #32276, #28999, .T. ) ;
#11396 = LOCAL_TIME ( 16, 7, 10.00000000000000000, #6013 ) ;
#11397 = LINE ( 'NONE', #21594, #2307 ) ;
#11398 = CARTESIAN_POINT ( 'NONE',  ( -8.000050800000000351, 0.000000000000000000, -3.000000000000000444 ) ) ;
#11399 = EDGE_LOOP ( 'NONE', ( #12867, #33062, #8775, #27301 ) ) ;
#11400 = CARTESIAN_POINT ( 'NONE',  ( 20.92250000136559507, 0.3178988483021036315, 3.024605502323848949 ) ) ;
#11401 = EDGE_CURVE ( 'NONE', #17041, #31833, #4977, .T. ) ;
#11402 = DIRECTION ( 'NONE',  ( 0.000000000000000000, 0.000000000000000000, 1.000000000000000000 ) ) ;
#11404 = CARTESIAN_POINT ( 'NONE',  ( 6.357667975083865386, -7.724391461487817523, 3.797112024431991362 ) ) ;
#11403 = CARTESIAN_POINT ( 'NONE',  ( 25.75999999999999801, -2.208672634433321348E-15, 0.000000000000000000 ) ) ;
#11405 = EDGE_CURVE ( 'NONE', #7918, #8629, #17344, .T. ) ;
#11406 = EDGE_LOOP ( 'NONE', ( #29705, #15226, #771, #28787 ) ) ;
#11407 = CIRCLE ( 'NONE', #8728, 10.94895958125474245 ) ;
#11408 = CYLINDRICAL_SURFACE ( 'NONE', #12859, 2.999999999999999112 ) ;
#11409 = VERTEX_POINT ( 'NONE', #14968 ) ;
#11411 = ORIENTED_EDGE ( 'NONE', *, *, #19461, .F. ) ;
#11410 = CARTESIAN_POINT ( 'NONE',  ( 40.87775403842539390, -5.752705061965228239, -3.999773184981716412 ) ) ;
#11412 = ORIENTED_EDGE ( 'NONE', *, *, #10018, .F. ) ;
#11413 = CARTESIAN_POINT ( 'NONE',  ( -8.000050800000002127, 3.543061387910618976, -0.5685797888652569521 ) ) ;
#11414 = AXIS2_PLACEMENT_3D ( 'NONE', #28327, #12769, #2779 ) ;
#11415 = EDGE_CURVE ( 'NONE', #6905, #14707, #30621, .T. ) ;
#11416 = AXIS2_PLACEMENT_3D ( 'NONE', #19245, #888, #24079 ) ;
#11417 = FACE_OUTER_BOUND ( 'NONE', #11457, .T. ) ;
#11419 = ORIENTED_EDGE ( 'NONE', *, *, #27712, .F. ) ;
#11418 = CARTESIAN_POINT ( 'NONE',  ( 5.489344046532322885, -3.969101778623974397, 7.082516960462303501 ) ) ;
#11420 = CARTESIAN_POINT ( 'NONE',  ( 16.51080712756689195, 12.51274273092968592, -1.500000000000000000 ) ) ;
#11421 = CARTESIAN_POINT ( 'NONE',  ( -3.657526656857886582, -9.739650026832221030, -1.743552401303936517 ) ) ;
#11422 = CARTESIAN_POINT ( 'NONE',  ( 108.0688902883350693, -19.06136513089643714, -3.153541353326339891 ) ) ;
#11423 = CC_DESIGN_APPROVAL ( #12877, ( #26353 ) ) ;
#11424 = CARTESIAN_POINT ( 'NONE',  ( 7.168700581567057029, -6.410142746916854151, -1.500000000000142553 ) ) ;
#11425 = DIRECTION ( 'NONE',  ( 1.000000000000000000, 0.000000000000000000, 0.000000000000000000 ) ) ;
#11426 = DIRECTION ( 'NONE',  ( 0.000000000000000000, 0.000000000000000000, 1.000000000000000000 ) ) ;
#11427 = EDGE_CURVE ( 'NONE', #21433, #12973, #32739, .T. ) ;
#11428 = CARTESIAN_POINT ( 'NONE',  ( 56.97280603064898941, -277.2763395528616002, -0.4463807625373771293 ) ) ;
#11429 = DIRECTION ( 'NONE',  ( -1.000000000000000000, 0.000000000000000000, 0.000000000000000000 ) ) ;
#11430 = CARTESIAN_POINT ( 'NONE',  ( -3.616018626656801960, -10.49347358198851943, 1.500000000000000000 ) ) ;
#11431 = DIRECTION ( 'NONE',  ( 0.000000000000000000, 0.000000000000000000, -1.000000000000000000 ) ) ;
#11432 = AXIS2_PLACEMENT_3D ( 'NONE', #17168, #22034, #29729 ) ;
#11433 = EDGE_LOOP ( 'NONE', ( #22359, #6518, #31325, #7659, #11725 ) ) ;
#11434 = DIRECTION ( 'NONE',  ( -1.000000000000000000, 8.574039729943019576E-17, -0.000000000000000000 ) ) ;
#11435 = DIRECTION ( 'NONE',  ( -1.000000000000000000, 0.000000000000000000, -0.000000000000000000 ) ) ;
#11436 = FACE_BOUND ( 'NONE', #21295, .T. ) ;
#11437 = ORIENTED_EDGE ( 'NONE', *, *, #26525, .T. ) ;
#11438 = DIRECTION ( 'NONE',  ( 0.03662738895564519870, -0.5274252892134370096, 0.8488115212910427587 ) ) ;
#11439 = EDGE_CURVE ( 'NONE', #293, #8403, #19680, .T. ) ;
#11440 = DIRECTION ( 'NONE',  ( -0.000000000000000000, 0.000000000000000000, 1.000000000000000000 ) ) ;
#11441 = APPROVAL_PERSON_ORGANIZATION ( #3273, #16528, #13611 ) ;
#11442 = ORIENTED_EDGE ( 'NONE', *, *, #17467, .T. ) ;
#11443 = FACE_OUTER_BOUND ( 'NONE', #23328, .T. ) ;
#11444 = EDGE_CURVE ( 'NONE', #16406, #22729, #27537, .T. ) ;
#11445 = ORIENTED_EDGE ( 'NONE', *, *, #26053, .F. ) ;
#11446 = ORIENTED_EDGE ( 'NONE', *, *, #19665, .T. ) ;
#11447 = CARTESIAN_POINT ( 'NONE',  ( 25.33940588721724296, -17.54454932707515979, -1.176512215459074806 ) ) ;
#11449 = VERTEX_POINT ( 'NONE', #12643 ) ;
#11448 = CARTESIAN_POINT ( 'NONE',  ( 5.489321486716459475, -8.012877392144806876, 1.307389195612950639 ) ) ;
#11450 = ORIENTED_EDGE ( 'NONE', *, *, #16499, .T. ) ;
#11451 = CARTESIAN_POINT ( 'NONE',  ( 3.249999999999999556, 7.360373001730986964, -4.729683950898791345 ) ) ;
#11452 = ORIENTED_EDGE ( 'NONE', *, *, #21954, .T. ) ;
#11453 = PLANE ( 'NONE',  #15650 ) ;
#11454 = CARTESIAN_POINT ( 'NONE',  ( 6.357667873252800028, -7.873899671211468387, -3.476490553296930131 ) ) ;
#11455 = CIRCLE ( 'NONE', #26922, 0.9999999999999991118 ) ;
#11457 = EDGE_LOOP ( 'NONE', ( #10789, #8131, #5340, #4878 ) ) ;
#11456 = CARTESIAN_POINT ( 'NONE',  ( 102.2233072702345282, -1.127920370132908578, -0.07017451552782009994 ) ) ;
#11458 = LINE ( 'NONE', #16614, #19887 ) ;
#11459 = FACE_OUTER_BOUND ( 'NONE', #22322, .T. ) ;
#11460 = CARTESIAN_POINT ( 'NONE',  ( -1.361091220733346370E-15, -7.944914065997057406, -7.533794289458144000 ) ) ;
#11461 = DIRECTION ( 'NONE',  ( 0.000000000000000000, -0.8191520442889866915, -0.5735764363510533759 ) ) ;
#11462 = CARTESIAN_POINT ( 'NONE',  ( 107.5625314920286399, -18.99452983251758553, 4.492264565199928228 ) ) ;
#11463 = ADVANCED_FACE ( 'NONE', ( #22847 ), #6957, .T. ) ;
#11464 = CARTESIAN_POINT ( 'NONE',  ( -0.5616989984784648282, -12.44624546261723985, -4.522129901861166701 ) ) ;
#11465 = CARTESIAN_POINT ( 'NONE',  ( 3.499999999999999556, -6.106419733534973027, -3.518755179752868223 ) ) ;
#11466 = CARTESIAN_POINT ( 'NONE',  ( -31.35000000000000142, -10.96966150227469328, 4.000000000000000000 ) ) ;
#11467 = DIRECTION ( 'NONE',  ( 1.000000000000000000, 0.000000000000000000, 0.000000000000000000 ) ) ;
#11468 = PLANE ( 'NONE',  #5455 ) ;
#11469 = CARTESIAN_POINT ( 'NONE',  ( -2.912942406915326909, 4.884725290497410777E-15, -2.999999999999999556 ) ) ;
#11470 = CARTESIAN_POINT ( 'NONE',  ( -2.558315521542159132, 0.4094970184090410137, -1.491740999229417941 ) ) ;
#11471 = B_SPLINE_CURVE_WITH_KNOTS ( 'NONE', 3,
 ( #14091, #3253, #757, #31831, #31490, #21456, #31674, #18961, #29148, #13900 ),
 .UNSPECIFIED., .F., .F.,
 ( 4, 2, 2, 2, 4 ),
 ( 2.740849916244211241E-07, 0.0005478761651001751599, 0.001095478245208724409, 0.001643080325317273658, 0.002190682405425823341 ),
 .UNSPECIFIED. ) ;
#11472 = CARTESIAN_POINT ( 'NONE',  ( 21.35999999999999943, -1.573300977624594976, 1.942864903642425700 ) ) ;
#11473 = CARTESIAN_POINT ( 'NONE',  ( -6.650050802731187538, 1.887961173149511618, 2.331437884370912705 ) ) ;
#11474 = ORIENTED_EDGE ( 'NONE', *, *, #25085, .F. ) ;
#11475 = EDGE_CURVE ( 'NONE', #10376, #5304, #3287, .T. ) ;
#11476 = CARTESIAN_POINT ( 'NONE',  ( -7.950050800000001416, -3.113457007523259268, 0.9222479816126455399 ) ) ;
#11477 = VECTOR ( 'NONE', #3867, 1000.000000000000000 ) ;
#11478 = CARTESIAN_POINT ( 'NONE',  ( 107.2357173345097578, 16.72967893420071661, -2.193670894733765309 ) ) ;
#11479 = CARTESIAN_POINT ( 'NONE',  ( -31.10918640827616244, -25.93932300454937945, 1.404595502311727362 ) ) ;
#11480 = CARTESIAN_POINT ( 'NONE',  ( 6.800570610007250494, -8.349954097221042204, 1.500000000000000000 ) ) ;
#11481 = ORIENTED_EDGE ( 'NONE', *, *, #16384, .T. ) ;
#11482 = CYLINDRICAL_SURFACE ( 'NONE', #10300, 8.749000000000002331 ) ;
#11483 = ORIENTED_EDGE ( 'NONE', *, *, #20651, .T. ) ;
#11484 = CARTESIAN_POINT ( 'NONE',  ( 2.325079879153031825, -10.58907985611580216, 1.500000000000000444 ) ) ;
#11485 = DATE_AND_TIME ( #16824, #29042 ) ;
#11486 = ORIENTED_EDGE ( 'NONE', *, *, #2650, .T. ) ;
#11487 = CARTESIAN_POINT ( 'NONE',  ( 18.83159731376371937, -5.059626785736968557, 4.275175838856085875 ) ) ;
#11488 = CARTESIAN_POINT ( 'NONE',  ( 9.302055952181039089, 0.2457637073014079521, -1.050000000000000044 ) ) ;
#11489 = CARTESIAN_POINT ( 'NONE',  ( 28.68519643165576838, -5.941144522439076425, -4.275175838848107368 ) ) ;
#11490 = CARTESIAN_POINT ( 'NONE',  ( 23.72853298629051366, -17.37454644214605537, -1.486007232662901023 ) ) ;
#11491 = CARTESIAN_POINT ( 'NONE',  ( 7.249760686538667009, 8.014274990069656823, -8.669741416787380218E-17 ) ) ;
#11492 = ORIENTED_EDGE ( 'NONE', *, *, #16384, .F. ) ;
#11493 = CARTESIAN_POINT ( 'NONE',  ( 23.22234552117474848, -21.93639154742791675, -1.104776480646283643 ) ) ;
#11494 = CARTESIAN_POINT ( 'NONE',  ( -50.81000000000000227, -10.96999999999998643, 9.000000000000000000 ) ) ;
#11495 = LINE ( 'NONE', #6646, #18858 ) ;
#11497 = ORIENTED_EDGE ( 'NONE', *, *, #1517, .F. ) ;
#11496 = CARTESIAN_POINT ( 'NONE',  ( 25.64588685331300510, 2.156159481431626279, -1.970234872520904901 ) ) ;
#11498 = CARTESIAN_POINT ( 'NONE',  ( -3.212550801365593678, 1.828967928396027176, -3.368539882008727115 ) ) ;
#11499 = DIRECTION ( 'NONE',  ( -1.000000000000000000, -0.000000000000000000, 0.000000000000000000 ) ) ;
#11500 = CYLINDRICAL_SURFACE ( 'NONE', #18819, 11.00000000000000000 ) ;
#11501 = DIRECTION ( 'NONE',  ( 3.623545766764117864E-17, 0.4226182617406882835, 0.9063077870366551547 ) ) ;
#11502 = DIRECTION ( 'NONE',  ( -0.03488359650710489562, -0.9989355049964836475, 0.03018263660036206095 ) ) ;
#11503 = CARTESIAN_POINT ( 'NONE',  ( 107.6937183830913654, -18.97455548421143590, 4.522180808795155826 ) ) ;
#11504 = DIRECTION ( 'NONE',  ( 0.000000000000000000, 0.000000000000000000, -1.000000000000000000 ) ) ;
#11505 = CARTESIAN_POINT ( 'NONE',  ( 24.49290772595112742, 0.1310194482076003919, 2.499999999999998668 ) ) ;
#11506 = CARTESIAN_POINT ( 'NONE',  ( 13.24595149388699511, -17.70232641593399947, 5.485967528433933538 ) ) ;
#11507 = ORIENTED_EDGE ( 'NONE', *, *, #6571, .F. ) ;
#11508 = EDGE_CURVE ( 'NONE', #13878, #24971, #21530, .T. ) ;
#11509 = CARTESIAN_POINT ( 'NONE',  ( -2.607304909706597229, 1.062355717592091686, 3.000000000000001332 ) ) ;
#11510 = ORIENTED_EDGE ( 'NONE', *, *, #10950, .F. ) ;
#11511 = EDGE_CURVE ( 'NONE', #15150, #780, #3899, .T. ) ;
#11512 = DIRECTION ( 'NONE',  ( -0.000000000000000000, -0.000000000000000000, -1.000000000000000000 ) ) ;
#11513 = CARTESIAN_POINT ( 'NONE',  ( 0.000000000000000000, 0.000000000000000000, 0.000000000000000000 ) ) ;
#11514 = EDGE_CURVE ( 'NONE', #2486, #2084, #32439, .T. ) ;
#11515 = CARTESIAN_POINT ( 'NONE',  ( -2.269454921107341594, 1.816023192640135786, 3.086171154715485088 ) ) ;
#11516 = FACE_OUTER_BOUND ( 'NONE', #7721, .T. ) ;
#11517 = CARTESIAN_POINT ( 'NONE',  ( 7.249760686538667009, 0.000000000000000000, 0.000000000000000000 ) ) ;
#11518 = ORIENTED_EDGE ( 'NONE', *, *, #8981, .F. ) ;
#11519 = LINE ( 'NONE', #6982, #30582 ) ;
#11520 = ORIENTED_EDGE ( 'NONE', *, *, #25526, .T. ) ;
#11521 = SECURITY_CLASSIFICATION_LEVEL ( 'unclassified' ) ;
#11522 = CARTESIAN_POINT ( 'NONE',  ( 40.88398722466511259, -6.895802492134996520, 3.994702139290142284 ) ) ;
#11523 = CARTESIAN_POINT ( 'NONE',  ( 10.57125986779756843, 4.681538312723528605, -0.8254815157534771686 ) ) ;
#11524 = VERTEX_POINT ( 'NONE', #605 ) ;
#11525 = CARTESIAN_POINT ( 'NONE',  ( 0.000000000000000000, -10.85582367538895276, 1.425064293572299023 ) ) ;
#11526 = ORIENTED_EDGE ( 'NONE', *, *, #32492, .T. ) ;
#11527 = ORIENTED_EDGE ( 'NONE', *, *, #16769, .T. ) ;
#11528 = CARTESIAN_POINT ( 'NONE',  ( 24.42249999999999943, -2.378061970571983430, 1.291182301015471490 ) ) ;
#11529 = CARTESIAN_POINT ( 'NONE',  ( -2.762550801365593500, -2.752080473201636845, 2.228590825266444586 ) ) ;
#11530 = CARTESIAN_POINT ( 'NONE',  ( 22.23500000000000298, 0.2613211581691317065, 2.486304738420681559 ) ) ;
#11531 = DIRECTION ( 'NONE',  ( -1.000000000000000000, 8.574039729943018344E-17, -0.000000000000000000 ) ) ;
#11532 =( BOUNDED_CURVE ( )  B_SPLINE_CURVE ( 3, ( #839, #15713, #6164, #23384 ),
 .UNSPECIFIED., .F., .F. ) 
 B_SPLINE_CURVE_WITH_KNOTS ( ( 4, 4 ),
 ( 1.570796326794896558, 3.141592653589793116 ),
 .UNSPECIFIED. ) 
 CURVE ( )  GEOMETRIC_REPRESENTATION_ITEM ( )  RATIONAL_B_SPLINE_CURVE ( ( 1.000000000000000000, 0.8047378541243649375, 0.8047378541243649375, 1.000000000000000000 ) ) 
 REPRESENTATION_ITEM ( '' )  );
#11534 = VERTEX_POINT ( 'NONE', #23672 ) ;
#11533 = CARTESIAN_POINT ( 'NONE',  ( 7.249760686538667009, -6.139290821770219786, -5.151476664237539360 ) ) ;
#11535 = CARTESIAN_POINT ( 'NONE',  ( -5.287550801365593856, -2.752080473201636845, 2.228590825266444586 ) ) ;
#11536 = CARTESIAN_POINT ( 'NONE',  ( 107.8039769746389425, 17.08662637267895690, -1.979454822623186949 ) ) ;
#11537 = DIRECTION ( 'NONE',  ( -1.000000000000000000, -0.000000000000000000, -0.000000000000000000 ) ) ;
#11538 = LINE ( 'NONE', #6842, #17816 ) ;
#11539 = ORIENTED_EDGE ( 'NONE', *, *, #28831, .T. ) ;
#11541 = ORIENTED_EDGE ( 'NONE', *, *, #15380, .T. ) ;
#11540 = CARTESIAN_POINT ( 'NONE',  ( 7.064632940817594076, -7.199384779417085767, -4.973063321323950348 ) ) ;
#11542 = DIRECTION ( 'NONE',  ( -1.000000000000000000, 0.000000000000000000, -0.000000000000000000 ) ) ;
#11543 = CARTESIAN_POINT ( 'NONE',  ( 23.23500000273119070, 2.486304738420679783, -0.2613211581691337604 ) ) ;
#11544 = EDGE_CURVE ( 'NONE', #4684, #11582, #19388, .T. ) ;
#11545 = CARTESIAN_POINT ( 'NONE',  ( 24.80306213860341558, -17.49230408913766865, 1.499999999999999778 ) ) ;
#11546 = EDGE_CURVE ( 'NONE', #20076, #6604, #792, .T. ) ;
#11547 = CARTESIAN_POINT ( 'NONE',  ( -30.09452540745392923, 13.10954151769360720, 1.499999999999227507 ) ) ;
#11548 = CARTESIAN_POINT ( 'NONE',  ( -23.54713438637982748, 8.275374457817617824, 8.599999999999999645 ) ) ;
#11549 = CARTESIAN_POINT ( 'NONE',  ( 0.3749740905865315277, -6.632019415960365372, -7.612528756000566332 ) ) ;
#11550 = DIRECTION ( 'NONE',  ( -1.000000000000000000, 0.000000000000000000, 0.000000000000000000 ) ) ;
#11551 = CARTESIAN_POINT ( 'NONE',  ( -3.187550801365593767, 3.521866450007987037, 0.3701630799359328372 ) ) ;
#11552 = DIRECTION ( 'NONE',  ( 0.7822388118548811997, -0.4516257885949860884, 0.4291113938172938513 ) ) ;
#11553 = ORIENTED_EDGE ( 'NONE', *, *, #25102, .T. ) ;
#11554 = CARTESIAN_POINT ( 'NONE',  ( -34.48223484310472031, 0.5000000000000000000, 2.552009564962237853 ) ) ;
#11555 = LINE ( 'NONE', #26119, #21561 ) ;
#11557 = DIRECTION ( 'NONE',  ( -1.000000000000000000, -0.000000000000000000, -0.000000000000000000 ) ) ;
#11556 = CARTESIAN_POINT ( 'NONE',  ( 3.249999999999999556, 2.223716399045570835, 8.461683424509324425 ) ) ;
#11558 = ORIENTED_EDGE ( 'NONE', *, *, #13035, .T. ) ;
#11559 = CARTESIAN_POINT ( 'NONE',  ( 7.249760686538667009, 6.139290821770327256, -5.151476664237414127 ) ) ;
#11560 = VERTEX_POINT ( 'NONE', #121 ) ;
#11561 = DIRECTION ( 'NONE',  ( -0.000000000000000000, 0.000000000000000000, 1.000000000000000000 ) ) ;
#11563 = ORIENTED_EDGE ( 'NONE', *, *, #7288, .T. ) ;
#11562 = CARTESIAN_POINT ( 'NONE',  ( 69.01325465695039441, -4.970808894665998068, -3.994703126863269560 ) ) ;
#11564 = ORIENTED_EDGE ( 'NONE', *, *, #29337, .T. ) ;
#11565 = DIRECTION ( 'NONE',  ( -0.000000000000000000, 1.000000000000000000, 0.000000000000000000 ) ) ;
#11567 = VERTEX_POINT ( 'NONE', #5785 ) ;
#11566 = CARTESIAN_POINT ( 'NONE',  ( -4.075703125331459731, -9.746317125368902268, -1.500000000000000222 ) ) ;
#11568 = LINE ( 'NONE', #32482, #32549 ) ;
#11569 = EDGE_CURVE ( 'NONE', #17732, #11755, #707, .T. ) ;
#11570 = FACE_OUTER_BOUND ( 'NONE', #21771, .T. ) ;
#11571 = CARTESIAN_POINT ( 'NONE',  ( 6.879500825888936077, -8.675028761530066745, -1.500000000000000000 ) ) ;
#11573 = EDGE_LOOP ( 'NONE', ( #22756, #8378, #22758, #7129, #19933, #549, #17086, #26857, #24366, #24582, #2018, #16109, #24775, #29673, #6704, #27259, #21832, #13621, #2383, #9408, #17579, #14038, #1692, #2530, #14900, #25243, #12706, #16205, #30851, #817, #28248, #11228, #2282, #26335, #14534, #5131, #26084, #16501, #15865, #30327, #6301, #25916, #12238, #18893, #27274, #5920, #14803, #9312, #109, #2320, #31818, #29259, #13819, #1988, #18090, #30230, #18 ) ) ;
#11572 = CARTESIAN_POINT ( 'NONE',  ( 108.0572303891428589, -18.89346548315845098, -4.650729098309561493 ) ) ;
#11574 = DIRECTION ( 'NONE',  ( 0.4809547266710045843, 0.000000000000000000, -0.8767454310646957127 ) ) ;
#11575 = EDGE_CURVE ( 'NONE', #9413, #993, #3387, .T. ) ;
#11576 = CARTESIAN_POINT ( 'NONE',  ( 0.000000000000000000, 0.000000000000000000, 0.000000000000000000 ) ) ;
#11577 = DIRECTION ( 'NONE',  ( 8.574039729943018344E-17, 1.000000000000000000, 0.000000000000000000 ) ) ;
#11578 = EDGE_CURVE ( 'NONE', #4101, #9572, #8448, .T. ) ;
#11579 = DESIGN_CONTEXT ( 'detailed design', #2234, 'design' ) ;
#11580 = DIRECTION ( 'NONE',  ( 0.9993908270190957621, 0.03489949670250105246, 3.467333458611667963E-15 ) ) ;
#11581 = CARTESIAN_POINT ( 'NONE',  ( 41.44567272411835290, -7.615257740949710197, -4.522129901861164036 ) ) ;
#11582 = VERTEX_POINT ( 'NONE', #23195 ) ;
#11583 = CARTESIAN_POINT ( 'NONE',  ( -17.45597128428592981, -27.93932300454937590, 11.50000000000000000 ) ) ;
#11584 = ADVANCED_FACE ( 'NONE', ( #15471 ), #15818, .F. ) ;
#11585 = B_SPLINE_CURVE_WITH_KNOTS ( 'NONE', 3,
 ( #26457, #16389, #3399, #29120, #16051, #6205, #26600, #1374, #3703, #21747 ),
 .UNSPECIFIED., .F., .F.,
 ( 4, 3, 3, 4 ),
 ( 2.268813642641003460E-14, 3.069467774972272057E-06, 2.471397395936450551E-05, 3.618126716052627069E-05 ),
 .UNSPECIFIED. ) ;
#11586 = PLANE ( 'NONE',  #25197 ) ;
#11587 = DIRECTION ( 'NONE',  ( -1.000000000000000000, 8.574039729943018344E-17, 0.000000000000000000 ) ) ;
#11588 = ORIENTED_EDGE ( 'NONE', *, *, #23419, .F. ) ;
#11589 = CARTESIAN_POINT ( 'NONE',  ( 25.05656763645044904, 0.8852964313267434049, -2.499999999999997780 ) ) ;
#11590 = EDGE_CURVE ( 'NONE', #2834, #22995, #10310, .T. ) ;
#11591 = CARTESIAN_POINT ( 'NONE',  ( 109.7786606840771952, 18.61415246516070354, -5.396302277755718357 ) ) ;
#11592 = ORIENTED_EDGE ( 'NONE', *, *, #28848, .F. ) ;
#11593 = CARTESIAN_POINT ( 'NONE',  ( 3.744708216408842549, 0.000000000000000000, 1.000000000000000000 ) ) ;
#11594 = ORIENTED_EDGE ( 'NONE', *, *, #23713, .T. ) ;
#11595 = ORIENTED_EDGE ( 'NONE', *, *, #5669, .T. ) ;
#11596 = CARTESIAN_POINT ( 'NONE',  ( 41.43369393131069245, -3.642920876114430495, -2.713652344655540727 ) ) ;
#11597 = B_SPLINE_SURFACE_WITH_KNOTS ( 'NONE', 3, 3, ( 
 ( #17399, #6853, #19734, #4366, #30132, #32121, #14548, #24566, #2028, #24758 ),
 ( #29775, #27088, #17039, #12053, #9018, #1878, #4190, #26939, #27594, #22249 ),
 ( #6533, #32459, #1525, #4542, #11888, #9518, #22096, #14357, #27440, #4042 ),
 ( #17236, #25065, #12370, #16737, #11701, #14716, #12200, #1690, #22400, #6702 ),
 ( #32618, #2183, #9697, #31954, #19923, #7207, #19239, #4695, #29438, #14210 ),
 ( #24408, #21903, #9198, #19427, #29620, #18054, #22590, #32804, #10026, #17719 ),
 ( #27930, #10523, #22900, #2, #5349, #20236, #23245, #17902, #10187, #2682 ) ),
 .UNSPECIFIED., .F., .F., .F.,
 ( 4, 3, 4 ),
 ( 4, 3, 3, 4 ),
 ( -5.867317828880905293E-13, 0.4999999999997066236, 1.000000000000000000 ),
 ( 0.003598893295620731597, 0.5017994466482779137, 0.7508997233246064162, 1.000000000000935030 ),
 .UNSPECIFIED. ) ;
#11599 = ORIENTED_EDGE ( 'NONE', *, *, #15508, .F. ) ;
#11598 = DIRECTION ( 'NONE',  ( -1.000000000000000000, 0.000000000000000000, 0.000000000000000000 ) ) ;
#11600 = ORIENTED_EDGE ( 'NONE', *, *, #26078, .T. ) ;
#11601 = CARTESIAN_POINT ( 'NONE',  ( 23.23500000136559862, -1.570731468192933633, -2.892927487894330962 ) ) ;
#11602 = EDGE_CURVE ( 'NONE', #4019, #15085, #20832, .T. ) ;
#11603 = ORIENTED_EDGE ( 'NONE', *, *, #13508, .T. ) ;
#11604 = CARTESIAN_POINT ( 'NONE',  ( -1.694237876703138967, -1.500727999663424184, 4.522129901861158707 ) ) ;
#11605 = LINE ( 'NONE', #26649, #2733 ) ;
#11607 = ORIENTED_EDGE ( 'NONE', *, *, #21346, .F. ) ;
#11606 = CARTESIAN_POINT ( 'NONE',  ( 25.75960661490314507, 24.76082900280849586, -0.4463807625373413246 ) ) ;
#11608 = CARTESIAN_POINT ( 'NONE',  ( 21.67250000273118715, -2.378061970571983430, 1.291182301015471490 ) ) ;
#11609 = CARTESIAN_POINT ( 'NONE',  ( 6.037141812302424526, 1.028012177296197871, -8.411869123983606755 ) ) ;
#11610 = EDGE_CURVE ( 'NONE', #17346, #27475, #26027, .T. ) ;
#11611 = CARTESIAN_POINT ( 'NONE',  ( 101.8601177974632463, -4.884214737968172848, 2.639238349664508654 ) ) ;
#11612 = CARTESIAN_POINT ( 'NONE',  ( 3.249999999999999556, -4.729683950898817102, -7.360373001730970977 ) ) ;
#11613 = CARTESIAN_POINT ( 'NONE',  ( 108.0284409662735641, -18.47890495573541969, 4.354626199043353019 ) ) ;
#11614 = CARTESIAN_POINT ( 'NONE',  ( 3.249999999999999556, 8.264486777890107660, -4.472189673936814991 ) ) ;
#11615 = CYLINDRICAL_SURFACE ( 'NONE', #31046, 8.500000000000000000 ) ;
#11616 = DIRECTION ( 'NONE',  ( 1.000000000000000000, -0.000000000000000000, -0.000000000000000000 ) ) ;
#11617 = EDGE_CURVE ( 'NONE', #2486, #32250, #10313, .T. ) ;
#11618 = EDGE_CURVE ( 'NONE', #22141, #25215, #17807, .T. ) ;
#11619 = CARTESIAN_POINT ( 'NONE',  ( 109.1472041058641196, 18.90877050785844204, 4.999054092451761022 ) ) ;
#11620 = CARTESIAN_POINT ( 'NONE',  ( 3.078042720788278785, 4.239848598108514111, -5.465019080499220472 ) ) ;
#11621 = DIRECTION ( 'NONE',  ( 0.000000000000000000, 0.000000000000000000, 1.000000000000000000 ) ) ;
#11622 = CARTESIAN_POINT ( 'NONE',  ( 0.000000000000000000, 20.00000000000000000, 0.000000000000000000 ) ) ;
#11623 = EDGE_CURVE ( 'NONE', #28172, #4208, #25839, .T. ) ;
#11624 = CARTESIAN_POINT ( 'NONE',  ( -7.450050802731187360, 1.887961173149511618, 2.331437884370912705 ) ) ;
#11625 = ORIENTED_EDGE ( 'NONE', *, *, #32353, .T. ) ;
#11626 = CARTESIAN_POINT ( 'NONE',  ( -6.100050799999999995, 0.3135853898029611342, -2.983565686104819648 ) ) ;
#11627 = CARTESIAN_POINT ( 'NONE',  ( 107.1965041332822324, 16.51130747298126167, -1.725725757970127505 ) ) ;
#11628 = DIRECTION ( 'NONE',  ( -1.000000000000000000, 0.000000000000000000, 0.000000000000000000 ) ) ;
#11629 = CARTESIAN_POINT ( 'NONE',  ( 9.134478070377040737, -0.4075412271181343971, 1.000000000000000000 ) ) ;
#11630 = ORIENTED_EDGE ( 'NONE', *, *, #11578, .F. ) ;
#11631 = CARTESIAN_POINT ( 'NONE',  ( 8.037025183208234225, -10.89872694351413784, -1.499999999999999778 ) ) ;
#11632 = EDGE_CURVE ( 'NONE', #29340, #8396, #15122, .T. ) ;
#11633 = ORIENTED_EDGE ( 'NONE', *, *, #12400, .F. ) ;
#11634 = CARTESIAN_POINT ( 'NONE',  ( 3.866684586168369187, -11.79807535627656279, 1.500000000000000000 ) ) ;
#11635 = APPROVAL_DATE_TIME ( #1457, #11877 ) ;
#11636 = DIRECTION ( 'NONE',  ( 7.472768010111188679E-18, 0.08715574274765867935, -0.9961946980917455452 ) ) ;
#11637 = EDGE_LOOP ( 'NONE', ( #17904, #8509, #31405, #7747 ) ) ;
#11638 = CARTESIAN_POINT ( 'NONE',  ( 102.3474756592083850, -2.905342955644300673, 4.074610060380101650 ) ) ;
#11639 = CARTESIAN_POINT ( 'NONE',  ( 20.95640594539235835, 16.13890008475014071, -1.050000000000000044 ) ) ;
#11640 = CARTESIAN_POINT ( 'NONE',  ( 18.78723038048999072, -5.555560056344673647, -4.275175838854464061 ) ) ;
#11641 = DIRECTION ( 'NONE',  ( 1.000000000000000000, -8.574039729943018344E-17, -0.000000000000000000 ) ) ;
#11642 = DIRECTION ( 'NONE',  ( -0.000000000000000000, -0.7071067811865507924, -0.7071067811865441310 ) ) ;
#11643 = ORIENTED_EDGE ( 'NONE', *, *, #23466, .F. ) ;
#11644 = CARTESIAN_POINT ( 'NONE',  ( -17.34999999999999787, -10.96966150227469505, -1.500000000000000000 ) ) ;
#11645 = EDGE_CURVE ( 'NONE', #29851, #4862, #16054, .T. ) ;
#11646 = CARTESIAN_POINT ( 'NONE',  ( 23.27353278736381981, -21.94187821002792660, -1.000000000000000000 ) ) ;
#11647 = CARTESIAN_POINT ( 'NONE',  ( 6.880159540721329847, -7.943102264535277790, 3.624895993596839894 ) ) ;
#11649 = ORIENTED_EDGE ( 'NONE', *, *, #30354, .F. ) ;
#11648 = DIRECTION ( 'NONE',  ( -1.000000000000000000, 0.000000000000000000, 0.000000000000000000 ) ) ;
#11650 = DIRECTION ( 'NONE',  ( -0.000000000000000000, -0.000000000000000000, -1.000000000000000000 ) ) ;
#11651 = CARTESIAN_POINT ( 'NONE',  ( 1.624999999999999778, -4.762163868918207754, -9.915734732513271865 ) ) ;
#11652 = CARTESIAN_POINT ( 'NONE',  ( -0.9232102171129827894, 0.000000000000000000, -4.522129901861166701 ) ) ;
#11653 = CARTESIAN_POINT ( 'NONE',  ( 24.72695737054825926, 18.91229966141139229, 1.500000000000000000 ) ) ;
#11654 = DIRECTION ( 'NONE',  ( 1.000000000000000000, 0.000000000000000000, 1.388624693425297016E-14 ) ) ;
#11655 = ADVANCED_FACE ( 'NONE', ( #31708 ), #9271, .T. ) ;
#11656 = CARTESIAN_POINT ( 'NONE',  ( 6.749760686538667009, 0.000000000000000000, 0.000000000000000000 ) ) ;
#11657 = CARTESIAN_POINT ( 'NONE',  ( -3.449949199999996274, 7.347880794884120722E-16, 6.000000000000000888 ) ) ;
#11658 = CARTESIAN_POINT ( 'NONE',  ( 10.00000000000000178, -4.884328206559832353, -1.115095498423360754 ) ) ;
#11659 = VERTEX_POINT ( 'NONE', #23976 ) ;
#11660 = CARTESIAN_POINT ( 'NONE',  ( 5.887530024394193262, 2.518482652462555649, 8.008238305624853837 ) ) ;
#11661 = ORIENTED_EDGE ( 'NONE', *, *, #6044, .F. ) ;
#11662 = FACE_OUTER_BOUND ( 'NONE', #9336, .T. ) ;
#11663 = EDGE_CURVE ( 'NONE', #516, #19070, #26515, .T. ) ;
#11664 = CARTESIAN_POINT ( 'NONE',  ( -59.75626822162179508, -5.804869634004071521, 5.128141679950119602 ) ) ;
#11665 = CARTESIAN_POINT ( 'NONE',  ( 18.68265047573912341, -6.724553502642427461, -4.522129901861164036 ) ) ;
#11666 = CARTESIAN_POINT ( 'NONE',  ( 2.976845824368064442, 7.725179967474443465, -4.933977349953490688 ) ) ;
#11667 = CARTESIAN_POINT ( 'NONE',  ( 20.86000000136559507, 0.3178988483021036315, 3.024605502323848949 ) ) ;
#11668 = ORIENTED_EDGE ( 'NONE', *, *, #6491, .F. ) ;
#11669 = CARTESIAN_POINT ( 'NONE',  ( 107.2640681281359178, 16.88755960000225897, -2.532220120516956552 ) ) ;
#11670 = EDGE_CURVE ( 'NONE', #1567, #22104, #1435, .T. ) ;
#11671 = CC_DESIGN_PERSON_AND_ORGANIZATION_ASSIGNMENT ( #20094, #25754, ( #25253 ) ) ;
#11672 = VERTEX_POINT ( 'NONE', #8605 ) ;
#11673 = APPROVAL_STATUS ( 'not_yet_approved' ) ;
#11674 = CARTESIAN_POINT ( 'NONE',  ( 69.07039640138465586, -6.115296054910306367, 3.995337163039132555 ) ) ;
#11675 = CARTESIAN_POINT ( 'NONE',  ( -2.794738735352966685, 0.000000000000000000, 1.508259000770582059 ) ) ;
#11676 = ORIENTED_EDGE ( 'NONE', *, *, #9356, .T. ) ;
#11677 = CARTESIAN_POINT ( 'NONE',  ( 5.612718825656739519, 6.163864706064027033, -5.432357446996346262 ) ) ;
#11678 = ORIENTED_EDGE ( 'NONE', *, *, #23114, .F. ) ;
#11679 = ORIENTED_EDGE ( 'NONE', *, *, #14073, .F. ) ;
#11680 = CARTESIAN_POINT ( 'NONE',  ( 25.75999999999999801, -2.208672634433321348E-15, 0.000000000000000000 ) ) ;
#11681 = CARTESIAN_POINT ( 'NONE',  ( 4.749760686538667009, -6.940565734314625423, 4.007137495034787555 ) ) ;
#11682 = EDGE_CURVE ( 'NONE', #28172, #28865, #15686, .T. ) ;
#11683 = CARTESIAN_POINT ( 'NONE',  ( 21.60999999999999943, -1.942864903642428587, -1.573300977624592756 ) ) ;
#11684 = CARTESIAN_POINT ( 'NONE',  ( 3.640821217203817461, -12.13691508638171435, -1.758209645160216938 ) ) ;
#11686 = ORIENTED_EDGE ( 'NONE', *, *, #9488, .F. ) ;
#11685 = DIRECTION ( 'NONE',  ( -7.472768010112310340E-18, -0.08715574274767159957, 0.9961946980917444350 ) ) ;
#11687 = CARTESIAN_POINT ( 'NONE',  ( -3.187550801365593767, 3.521866450007987037, 0.3701630799359328372 ) ) ;
#11688 = DIRECTION ( 'NONE',  ( -0.1437473352845080599, 0.000000000000000000, 0.9896144216807893912 ) ) ;
#11689 = EDGE_CURVE ( 'NONE', #14000, #31571, #18825, .T. ) ;
#11690 = CARTESIAN_POINT ( 'NONE',  ( -58.25958745446412479, -3.632822961816825291, 5.448103880042390657 ) ) ;
#11691 = LINE ( 'NONE', #24246, #22090 ) ;
#11692 = VERTEX_POINT ( 'NONE', #19493 ) ;
#11694 = ORIENTED_EDGE ( 'NONE', *, *, #7407, .F. ) ;
#11693 = CYLINDRICAL_SURFACE ( 'NONE', #22456, 0.5000000000000000000 ) ;
#11695 = CARTESIAN_POINT ( 'NONE',  ( -6.800050800000000173, 2.331437884370912705, -1.887961173149511618 ) ) ;
#11696 = CARTESIAN_POINT ( 'NONE',  ( 20.86000000273118715, -1.942864903642428587, -1.573300977624592756 ) ) ;
#11697 = CARTESIAN_POINT ( 'NONE',  ( -17.74503016599027916, 14.86020659576482039, 1.860696004609410315 ) ) ;
#11698 = CARTESIAN_POINT ( 'NONE',  ( -30.18078978763795561, 12.16064947808525787, 1.928605623396606683 ) ) ;
#11699 = CARTESIAN_POINT ( 'NONE',  ( -4.224514321812577577, -5.429116791541773956, -1.500000000000080602 ) ) ;
#11700 = DIRECTION ( 'NONE',  ( 1.000000000000000000, -8.574039729943018344E-17, -0.000000000000000000 ) ) ;
#11701 = CARTESIAN_POINT ( 'NONE',  ( 47.88515715254438021, -3.977125052580793518, 1.169950612146031466 ) ) ;
#11702 = CARTESIAN_POINT ( 'NONE',  ( -2.637550801365593500, -1.088641768524163389, -3.675193018007246071 ) ) ;
#11703 = EDGE_LOOP ( 'NONE', ( #4078, #22800, #33031, #11018 ) ) ;
#11704 = CARTESIAN_POINT ( 'NONE',  ( 101.7025720532070778, -2.615595213129288332, 3.539106238044632313 ) ) ;
#11705 = EDGE_LOOP ( 'NONE', ( #29014, #28684, #8303, #29533 ) ) ;
#11706 = CIRCLE ( 'NONE', #22407, 2.999999999999998668 ) ;
#11707 = DIRECTION ( 'NONE',  ( -1.000000000000000000, 0.000000000000000000, -0.000000000000000000 ) ) ;
#11708 = CARTESIAN_POINT ( 'NONE',  ( 41.43369393131070666, -3.642920876109168926, -2.713652344655542503 ) ) ;
#11710 = CARTESIAN_POINT ( 'NONE',  ( 0.000000000000000000, 0.000000000000000000, -1.000000000000000000 ) ) ;
#11709 = FACE_OUTER_BOUND ( 'NONE', #10641, .T. ) ;
#11711 = ORIENTED_EDGE ( 'NONE', *, *, #11940, .F. ) ;
#11712 = VECTOR ( 'NONE', #30006, 1000.000000000000114 ) ;
#11713 =( BOUNDED_SURFACE ( )  B_SPLINE_SURFACE ( 1, 3, ( 
 ( #11775, #26837, #24328, #27154 ),
 ( #21324, #16958, #31527, #19315 ) ),
 .UNSPECIFIED., .F., .F., .F. ) 
 B_SPLINE_SURFACE_WITH_KNOTS ( ( 2, 2 ),
 ( 4, 4 ),
 ( 0.000000000000000000, 1.000000000000000000 ),
 ( 0.000000000000000000, 1.000000000000000000 ),
 .UNSPECIFIED. ) 
 GEOMETRIC_REPRESENTATION_ITEM ( )  RATIONAL_B_SPLINE_SURFACE ( (
 ( 1.000000000000000000, 0.9917560313531952332, 0.9917560313531952332, 1.000000000000000000),
 ( 1.000000000000000000, 0.9917560313531952332, 0.9917560313531952332, 1.000000000000000000) ) ) 
 REPRESENTATION_ITEM ( '' )  SURFACE ( )  );
#11714 = CARTESIAN_POINT ( 'NONE',  ( 17.99869063401903446, -21.49583829453732875, 1.499999999999999556 ) ) ;
#11715 = ORIENTED_EDGE ( 'NONE', *, *, #28362, .F. ) ;
#11716 = FACE_OUTER_BOUND ( 'NONE', #23661, .T. ) ;
#11718 = ORIENTED_EDGE ( 'NONE', *, *, #25443, .F. ) ;
#11717 = CARTESIAN_POINT ( 'NONE',  ( 84.96572415149093160, -4.061352282173294803, -3.997237729493234859 ) ) ;
#11719 = ORIENTED_EDGE ( 'NONE', *, *, #24763, .F. ) ;
#11720 = ADVANCED_FACE ( 'NONE', ( #11289 ), #11771, .F. ) ;
#11721 = CARTESIAN_POINT ( 'NONE',  ( 23.54750000000000654, -2.594547506269383685, -0.7685399846772043020 ) ) ;
#11722 = ADVANCED_FACE ( 'NONE', ( #6608 ), #18991, .F. ) ;
#11723 = DIRECTION ( 'NONE',  ( 0.000000000000000000, 0.000000000000000000, -1.000000000000000000 ) ) ;
#11725 = ORIENTED_EDGE ( 'NONE', *, *, #353, .F. ) ;
#11724 = DIRECTION ( 'NONE',  ( -1.000000000000000000, 0.000000000000000000, 0.000000000000000000 ) ) ;
#11726 = DIRECTION ( 'NONE',  ( 0.000000000000000000, -1.000000000000000000, 8.673617379884035472E-16 ) ) ;
#11727 = DIRECTION ( 'NONE',  ( -1.000000000000000000, -0.000000000000000000, -0.000000000000000000 ) ) ;
#11728 = CARTESIAN_POINT ( 'NONE',  ( 0.000000000000000000, 0.000000000000000000, 0.000000000000000000 ) ) ;
#11729 = CARTESIAN_POINT ( 'NONE',  ( 7.289999264625085296, -8.244573099997934307, -1.000000000000000000 ) ) ;
#11731 = VERTEX_POINT ( 'NONE', #27002 ) ;
#11730 = CARTESIAN_POINT ( 'NONE',  ( 108.0183420873304101, -18.33348361123931625, -4.566453197885271820 ) ) ;
#11732 = CARTESIAN_POINT ( 'NONE',  ( 10.00000000000000000, 4.467071865485470639, 1.625881193364712596 ) ) ;
#11733 = AXIS2_PLACEMENT_3D ( 'NONE', #15764, #18441, #10911 ) ;
#11734 = CIRCLE ( 'NONE', #31504, 8.500000000000000000 ) ;
#11735 = FACE_OUTER_BOUND ( 'NONE', #11399, .T. ) ;
#11736 = CARTESIAN_POINT ( 'NONE',  ( 0.000000000000000000, 0.000000000000000000, 0.000000000000000000 ) ) ;
#11737 = CARTESIAN_POINT ( 'NONE',  ( -2.675165579483918421, 0.2071067811865475727, 1.500000000000000000 ) ) ;
#11738 = CARTESIAN_POINT ( 'NONE',  ( 0.5032041927225600064, -6.298925283836295463, 7.418882907483850708 ) ) ;
#11739 = AXIS2_PLACEMENT_3D ( 'NONE', #7232, #27619, #7545 ) ;
#11740 = ORIENTED_EDGE ( 'NONE', *, *, #6735, .F. ) ;
#11741 = CARTESIAN_POINT ( 'NONE',  ( 108.5619817448483531, 15.65002148400673754, 0.4463807625373211185 ) ) ;
#11742 = DIRECTION ( 'NONE',  ( 0.000000000000000000, 0.8191520442889889120, 0.5735764363510503783 ) ) ;
#11743 = DIRECTION ( 'NONE',  ( 1.000000000000000000, 0.000000000000000000, 0.000000000000000000 ) ) ;
#11744 = ORIENTED_EDGE ( 'NONE', *, *, #2916, .F. ) ;
#11745 = B_SPLINE_CURVE_WITH_KNOTS ( 'NONE', 3,
 ( #28077, #30774, #12346, #14699, #2009, #22382, #12680, #7494, #20386, #22566 ),
 .UNSPECIFIED., .F., .F.,
 ( 4, 2, 2, 2, 4 ),
 ( -5.999999992363981562E-08, 0.0004826362445849100968, 0.0009653324891697438346, 0.001448028733754577789, 0.001930724978339411419 ),
 .UNSPECIFIED. ) ;
#11746 = LINE ( 'NONE', #14100, #7147 ) ;
#11747 = VECTOR ( 'NONE', #7329, 1000.000000000000000 ) ;
#11748 = DIRECTION ( 'NONE',  ( 0.000000000000000000, 2.042810365310287719E-14, 1.000000000000000000 ) ) ;
#11749 = VERTEX_POINT ( 'NONE', #8787 ) ;
#11750 = CARTESIAN_POINT ( 'NONE',  ( 7.452628691521980819, -4.595576623638184977, 1.000000000000000222 ) ) ;
#11751 = EDGE_LOOP ( 'NONE', ( #10964, #27764, #8070, #2354, #28537 ) ) ;
#11752 = AXIS2_PLACEMENT_3D ( 'NONE', #3651, #11330, #6460 ) ;
#11753 = EDGE_CURVE ( 'NONE', #6454, #32072, #13517, .T. ) ;
#11754 = AXIS2_PLACEMENT_3D ( 'NONE', #29917, #19220, #14339 ) ;
#11755 = VERTEX_POINT ( 'NONE', #21497 ) ;
#11756 = CARTESIAN_POINT ( 'NONE',  ( 0.000000000000000000, 0.000000000000000000, 0.000000000000000000 ) ) ;
#11757 = CALENDAR_DATE ( 2026, 6, 10 ) ;
#11759 = ORIENTED_EDGE ( 'NONE', *, *, #4999, .F. ) ;
#11758 = CARTESIAN_POINT ( 'NONE',  ( 5.377543748152549874, -7.892520144992443143, 1.391664247347202288 ) ) ;
#11760 = EDGE_LOOP ( 'NONE', ( #1868, #7503, #24957, #25296 ) ) ;
#11761 = CARTESIAN_POINT ( 'NONE',  ( 21.17250000136559507, -2.363507492473152283, -1.913930629741525280 ) ) ;
#11762 = ORIENTED_EDGE ( 'NONE', *, *, #15821, .T. ) ;
#11764 = VECTOR ( 'NONE', #30231, 1000.000000000000000 ) ;
#11763 = PLANE ( 'NONE',  #27390 ) ;
#11765 = DIRECTION ( 'NONE',  ( 0.1908089953765452762, -4.720536385445197917E-14, 0.9816271834476639757 ) ) ;
#11767 = ORIENTED_EDGE ( 'NONE', *, *, #7715, .T. ) ;
#11766 = LINE ( 'NONE', #30004, #30997 ) ;
#11768 = CARTESIAN_POINT ( 'NONE',  ( 10.00000000000000000, -3.641590349731949505, 3.055657119358789142 ) ) ;
#11769 = CARTESIAN_POINT ( 'NONE',  ( -56.39515584769779366, 0.01341171002345545316, -1.010295832186372422 ) ) ;
#11770 = DIRECTION ( 'NONE',  ( 0.000000000000000000, 0.000000000000000000, 1.000000000000000000 ) ) ;
#11771 = PLANE ( 'NONE',  #28508 ) ;
#11772 = AXIS2_PLACEMENT_3D ( 'NONE', #4175, #29760, #1510 ) ;
#11773 = CARTESIAN_POINT ( 'NONE',  ( -1.824298235657398903, -2.866444442093540879, -5.485967528433938867 ) ) ;
#11774 = EDGE_CURVE ( 'NONE', #28142, #22329, #21974, .T. ) ;
#11775 = CARTESIAN_POINT ( 'NONE',  ( 16.36487458112949511, 19.37645981759117575, 4.629213727441584325 ) ) ;
#11776 = CARTESIAN_POINT ( 'NONE',  ( 15.28872660057388799, 20.76088595412472415, -4.612695725900421984 ) ) ;
#11777 = AXIS2_PLACEMENT_3D ( 'NONE', #29679, #6114, #1086 ) ;
#11778 = CIRCLE ( 'NONE', #1101, 0.4999999999999997224 ) ;
#11779 = DIRECTION ( 'NONE',  ( 1.000000000000000000, -8.574039729943018344E-17, -0.000000000000000000 ) ) ;
#11780 = CARTESIAN_POINT ( 'NONE',  ( 0.000000000000000000, 0.000000000000000000, 11.50000000000000000 ) ) ;
#11781 = PLANE ( 'NONE',  #13445 ) ;
#11782 = AXIS2_PLACEMENT_3D ( 'NONE', #11681, #21880, #32096 ) ;
#11783 = EDGE_CURVE ( 'NONE', #27107, #25565, #11277, .T. ) ;
#11784 = CARTESIAN_POINT ( 'NONE',  ( 108.1033190332167351, 18.75348106957532579, 4.532405376036182432 ) ) ;
#11785 = CARTESIAN_POINT ( 'NONE',  ( -7.150050802731187538, -2.983565686104819648, -0.3135853898029605791 ) ) ;
#11786 = VERTEX_POINT ( 'NONE', #3615 ) ;
#11787 = CARTESIAN_POINT ( 'NONE',  ( -7.637550801365593500, -3.675193018007246071, 1.088641768524163167 ) ) ;
#11788 = CIRCLE ( 'NONE', #16048, 0.4500000000000021205 ) ;
#11789 = ADVANCED_FACE ( 'NONE', ( #13775 ), #24156, .F. ) ;
#11790 = CARTESIAN_POINT ( 'NONE',  ( -50.81000000000000227, -10.96999999999998643, 5.871858320049875957 ) ) ;
#11791 = CARTESIAN_POINT ( 'NONE',  ( -5.407304909706597051, -1.062355717592097015, -2.999999999999998668 ) ) ;
#11792 = CARTESIAN_POINT ( 'NONE',  ( 7.192400642327566374, -7.644771086454712261, 1.500000000000285549 ) ) ;
#11793 = VERTEX_POINT ( 'NONE', #27502 ) ;
#11794 = DIRECTION ( 'NONE',  ( -6.062761635205610267E-17, -0.7071067811865509034, 0.7071067811865441310 ) ) ;
#11795 = CARTESIAN_POINT ( 'NONE',  ( -7.200050800000000528, -2.331437884370912705, 1.887961173149512062 ) ) ;
#11796 = VERTEX_POINT ( 'NONE', #32522 ) ;
#11797 = CARTESIAN_POINT ( 'NONE',  ( 0.2521140843041953516, -7.034306361774945948, 1.499999999999964473 ) ) ;
#11798 = PERSON_AND_ORGANIZATION ( #6766, #25292 ) ;
#11799 = VECTOR ( 'NONE', #8456, 1000.000000000000000 ) ;
#11800 = DIRECTION ( 'NONE',  ( 1.000000000000000000, -0.000000000000000000, -0.000000000000000000 ) ) ;
#11802 = ADVANCED_FACE ( 'NONE', ( #27152 ), #9772, .T. ) ;
#11801 = ORIENTED_EDGE ( 'NONE', *, *, #29356, .F. ) ;
#11803 = CARTESIAN_POINT ( 'NONE',  ( 3.326350470277788407, -17.46743482665522151, 1.499999999999998446 ) ) ;
#11804 = EDGE_CURVE ( 'NONE', #3232, #19511, #21014, .T. ) ;
#11805 = CIRCLE ( 'NONE', #9117, 12.49867430706171767 ) ;
#11806 = AXIS2_PLACEMENT_3D ( 'NONE', #18874, #21212, #23380 ) ;
#11807 = CARTESIAN_POINT ( 'NONE',  ( -5.757304906975409864, 1.062355717592095683, 2.999999999999999112 ) ) ;
#11808 = CARTESIAN_POINT ( 'NONE',  ( 40.88087200082812700, -6.322651088315213386, -4.312042181584450518 ) ) ;
#11809 = VECTOR ( 'NONE', #5254, 1000.000000000000000 ) ;
#11810 = CARTESIAN_POINT ( 'NONE',  ( 24.31705961742920863, -17.33693665021395347, -1.331050360515587005 ) ) ;
#11811 = CARTESIAN_POINT ( 'NONE',  ( 10.57125986779756843, -4.681538312723523276, 0.8254815157535098091 ) ) ;
#11812 = ORIENTED_EDGE ( 'NONE', *, *, #27003, .F. ) ;
#11813 = DIRECTION ( 'NONE',  ( 1.000000000000000000, -8.574039729943018344E-17, -0.000000000000000000 ) ) ;
#11814 = CARTESIAN_POINT ( 'NONE',  ( -56.28351068136514357, 0.000000000000000000, 0.000000000000000000 ) ) ;
#11815 = DIRECTION ( 'NONE',  ( 1.000000000000000000, -0.000000000000000000, -0.000000000000000000 ) ) ;
#11816 = VECTOR ( 'NONE', #27528, 999.9999999999998863 ) ;
#11818 = ORIENTED_EDGE ( 'NONE', *, *, #18827, .T. ) ;
#11817 = DIRECTION ( 'NONE',  ( -0.000000000000000000, -1.000000000000000000, -0.000000000000000000 ) ) ;
#11819 = DIRECTION ( 'NONE',  ( 8.574039729943018344E-17, 1.000000000000000000, 0.000000000000000000 ) ) ;
#11820 = CARTESIAN_POINT ( 'NONE',  ( 19.10390797508231131, -2.015740111943978619, -0.07017451552781628354 ) ) ;
#11821 = CARTESIAN_POINT ( 'NONE',  ( 0.3285611067768016147, -13.34342412962908320, -4.522129901861166701 ) ) ;
#11822 = CARTESIAN_POINT ( 'NONE',  ( 25.71957259916088390, 19.01870514234148857, 1.360524438179210538 ) ) ;
#11823 = CYLINDRICAL_SURFACE ( 'NONE', #5582, 0.4500000000000025646 ) ;
#11824 = ADVANCED_FACE ( 'NONE', ( #11963 ), #32865, .F. ) ;
#11825 = CARTESIAN_POINT ( 'NONE',  ( 10.57125986779756843, 4.681538312723516171, 0.8254815157535410064 ) ) ;
#11826 = LINE ( 'NONE', #19862, #13416 ) ;
#11827 = LINE ( 'NONE', #9321, #5989 ) ;
#11828 = CARTESIAN_POINT ( 'NONE',  ( 84.65816297383794620, -6.961284151106944762, 0.07017451552781739377 ) ) ;
#11829 = VERTEX_POINT ( 'NONE', #12607 ) ;
#11830 = CIRCLE ( 'NONE', #26253, 4.000000000000001776 ) ;
#11831 = CARTESIAN_POINT ( 'NONE',  ( 7.249760686538667009, 2.318425219014230265, 8.437262856154170265 ) ) ;
#11832 = VERTEX_POINT ( 'NONE', #4602 ) ;
#11833 = AXIS2_PLACEMENT_3D ( 'NONE', #27336, #19815, #1776 ) ;
#11834 = AXIS2_PLACEMENT_3D ( 'NONE', #3431, #19271, #11087 ) ;
#11835 = CARTESIAN_POINT ( 'NONE',  ( 25.29647035826949875, -17.54044501667244305, -1.294083318812917494 ) ) ;
#11836 = CARTESIAN_POINT ( 'NONE',  ( 109.1169603330106526, 18.74036124698735151, 5.233955722116973241 ) ) ;
#11837 = LINE ( 'NONE', #17006, #14043 ) ;
#11838 = CARTESIAN_POINT ( 'NONE',  ( -17.45597128428593336, -27.93932300454937590, 11.00000000000000000 ) ) ;
#11839 = DIRECTION ( 'NONE',  ( -0.000000000000000000, -0.000000000000000000, -1.000000000000000000 ) ) ;
#11840 = VECTOR ( 'NONE', #18563, 1000.000000000000000 ) ;
#11841 = ORIENTED_EDGE ( 'NONE', *, *, #2235, .F. ) ;
#11842 = CARTESIAN_POINT ( 'NONE',  ( -31.43793636962776006, -25.49623161314221065, 1.500000000000015765 ) ) ;
#11843 = ADVANCED_FACE ( 'NONE', ( #22810 ), #20302, .T. ) ;
#11844 = AXIS2_PLACEMENT_3D ( 'NONE', #15766, #23435, #17592 ) ;
#11845 = CIRCLE ( 'NONE', #10248, 8.500000000000000000 ) ;
#11846 = ORIENTED_EDGE ( 'NONE', *, *, #27024, .T. ) ;
#11847 = COORDINATED_UNIVERSAL_TIME_OFFSET ( 0, 0, .AHEAD. ) ;
#11848 = ADVANCED_FACE ( 'NONE', ( #30193 ), #32690, .T. ) ;
#11849 = CARTESIAN_POINT ( 'NONE',  ( 40.88390192208362350, -6.880058196568322515, 4.018749766545396618 ) ) ;
#11850 = EDGE_CURVE ( 'NONE', #8422, #29995, #24216, .T. ) ;
#11851 = CARTESIAN_POINT ( 'NONE',  ( -7.000050800000000351, 0.000000000000000000, 0.000000000000000000 ) ) ;
#11852 = VECTOR ( 'NONE', #9374, 1000.000000000000000 ) ;
#11853 = CARTESIAN_POINT ( 'NONE',  ( 10.00000000000000000, -2.376879293651093406, 4.116875700062075261 ) ) ;
#11854 = ORIENTED_EDGE ( 'NONE', *, *, #16432, .T. ) ;
#11855 = AXIS2_PLACEMENT_3D ( 'NONE', #25613, #388, #17582 ) ;
#11856 = VERTEX_POINT ( 'NONE', #4445 ) ;
#11857 = VECTOR ( 'NONE', #16687, 1000.000000000000000 ) ;
#11858 = DIRECTION ( 'NONE',  ( 1.000000000000000000, 0.000000000000000000, 0.000000000000000000 ) ) ;
#11859 = CARTESIAN_POINT ( 'NONE',  ( -2.212550801365593234, 3.368539882008727115, 1.828967928396027176 ) ) ;
#11860 = AXIS2_PLACEMENT_3D ( 'NONE', #12615, #30711, #20311 ) ;
#11861 = CARTESIAN_POINT ( 'NONE',  ( 24.85999999999999943, 1.573300977624590313, -1.942864903642426144 ) ) ;
#11862 = CIRCLE ( 'NONE', #18814, 11.00000000000000000 ) ;
#11863 = CARTESIAN_POINT ( 'NONE',  ( 8.397335469007884967, -14.43511845646028391, -1.755102877586449450 ) ) ;
#11865 = ORIENTED_EDGE ( 'NONE', *, *, #32853, .F. ) ;
#11864 = CYLINDRICAL_SURFACE ( 'NONE', #32056, 4.000000000000001776 ) ;
#11866 = CARTESIAN_POINT ( 'NONE',  ( -4.587550801365592790, -0.3701630799359326152, 3.521866450007987037 ) ) ;
#11867 = VECTOR ( 'NONE', #22031, 1000.000000000000000 ) ;
#11868 = CARTESIAN_POINT ( 'NONE',  ( 25.56776753627337229, -17.11417227705151234, 1.000000000000000000 ) ) ;
#11869 = CARTESIAN_POINT ( 'NONE',  ( -50.59999999999987352, -21.43932300454937945, 1.500000000000000000 ) ) ;
#11870 = FACE_OUTER_BOUND ( 'NONE', #3305, .T. ) ;
#11871 = AXIS2_PLACEMENT_3D ( 'NONE', #5195, #17722, #25259 ) ;
#11872 = ORIENTED_EDGE ( 'NONE', *, *, #32033, .T. ) ;
#11874 = VERTEX_POINT ( 'NONE', #19994 ) ;
#11873 = LINE ( 'NONE', #16536, #25656 ) ;
#11875 = AXIS2_PLACEMENT_3D ( 'NONE', #31648, #24272, #9033 ) ;
#11876 = EDGE_CURVE ( 'NONE', #18235, #30423, #27815, .T. ) ;
#11877 = APPROVAL ( #19018, 'UNSPECIFIED' ) ;
#11878 = CARTESIAN_POINT ( 'NONE',  ( 0.000000000000000000, 5.241389472434724084, -4.711457988287002685 ) ) ;
#11879 = CARTESIAN_POINT ( 'NONE',  ( 10.56870887191539587, 4.467071865485470639, 1.625881193364712596 ) ) ;
#11880 = CARTESIAN_POINT ( 'NONE',  ( 24.73500000136559507, 3.156283516753366047, 0.9349337715887203748 ) ) ;
#11881 = AXIS2_PLACEMENT_3D ( 'NONE', #19848, #30057, #27686 ) ;
#11882 = CARTESIAN_POINT ( 'NONE',  ( -6.300050802731188782, -2.853674364686378695, -1.549418761218566809 ) ) ;
#11883 = DIRECTION ( 'NONE',  ( -1.000000000000000000, 0.000000000000000000, 0.000000000000000000 ) ) ;
#11884 = CIRCLE ( 'NONE', #32708, 8.750000000000000000 ) ;
#11885 = CARTESIAN_POINT ( 'NONE',  ( 10.00000000000000000, -0.8254815157534942660, -4.681538312723525053 ) ) ;
#11886 = TOROIDAL_SURFACE ( 'NONE', #6014, 10.46966150227468795, 0.5000000000000000000 ) ;
#11887 = AXIS2_PLACEMENT_3D ( 'NONE', #12085, #32652, #24791 ) ;
#11888 = CARTESIAN_POINT ( 'NONE',  ( 47.88685968119389003, -4.079890078784098151, 1.529339664924048048 ) ) ;
#11889 = CARTESIAN_POINT ( 'NONE',  ( -2.937550801365593323, -1.828967928396026510, 3.368539882008728004 ) ) ;
#11890 = EDGE_LOOP ( 'NONE', ( #2888, #15220, #28278, #27491 ) ) ;
#11891 = CARTESIAN_POINT ( 'NONE',  ( -2.921917104085828724E-16, -3.407865132560154997, -3.672404558090073490 ) ) ;
#11892 = ORIENTED_EDGE ( 'NONE', *, *, #18269, .T. ) ;
#11893 = EDGE_CURVE ( 'NONE', #26782, #25696, #30510, .T. ) ;
#11894 = AXIS2_PLACEMENT_3D ( 'NONE', #28127, #7556, #22283 ) ;
#11895 = VECTOR ( 'NONE', #3739, 1000.000000000000227 ) ;
#11896 = LINE ( 'NONE', #27600, #25753 ) ;
#11897 = AXIS2_PLACEMENT_3D ( 'NONE', #7540, #27955, #5060 ) ;
#11898 = DIRECTION ( 'NONE',  ( 0.000000000000000000, 0.000000000000000000, 1.000000000000000000 ) ) ;
#11899 = CARTESIAN_POINT ( 'NONE',  ( 6.749760686538667009, 6.429395695523604153E-16, -5.000000000000000000 ) ) ;
#11900 = CARTESIAN_POINT ( 'NONE',  ( 22.99325939039831823, -17.14855239172962698, 1.466877076793034140 ) ) ;
#11901 = ORIENTED_EDGE ( 'NONE', *, *, #23455, .F. ) ;
#11902 = AXIS2_PLACEMENT_3D ( 'NONE', #8848, #13838, #8510 ) ;
#11903 = DIRECTION ( 'NONE',  ( 0.1908089953765453595, -0.000000000000000000, 0.9816271834476638647 ) ) ;
#11904 = ORIENTED_EDGE ( 'NONE', *, *, #32458, .T. ) ;
#11905 = CARTESIAN_POINT ( 'NONE',  ( 8.923848839947336131, 0.3991291121161160138, 1.500000000000000000 ) ) ;
#11907 = VERTEX_POINT ( 'NONE', #4255 ) ;
#11906 = CARTESIAN_POINT ( 'NONE',  ( 54.94549555304173083, -5.360154568442904832, -3.994702633084190158 ) ) ;
#11908 = VERTEX_POINT ( 'NONE', #17455 ) ;
#11909 = CARTESIAN_POINT ( 'NONE',  ( 0.000000000000000000, 37.67766952966368876, 0.000000000000000000 ) ) ;
#11910 = VECTOR ( 'NONE', #16870, 1000.000000000000000 ) ;
#11911 = CARTESIAN_POINT ( 'NONE',  ( 23.95058674323829706, -2.449331254355760823, 0.07017451552782173751 ) ) ;
#11913 = EDGE_LOOP ( 'NONE', ( #5093, #19259, #26812 ) ) ;
#11912 = CARTESIAN_POINT ( 'NONE',  ( -3.727414643486526291, -1.844583555841048828, -1.500000000000000222 ) ) ;
#11914 = VECTOR ( 'NONE', #31564, 1000.000000000000000 ) ;
#11915 = CARTESIAN_POINT ( 'NONE',  ( 20.83472080799475989, 16.60661545279006290, -1.500000000000000000 ) ) ;
#11916 = AXIS2_PLACEMENT_3D ( 'NONE', #26716, #3524, #13187 ) ;
#11917 = CARTESIAN_POINT ( 'NONE',  ( 5.489321606599603776, -2.874206582856462688, 7.593050043411102124 ) ) ;
#11918 = AXIS2_PLACEMENT_3D ( 'NONE', #9324, #29735, #6813 ) ;
#11919 = CARTESIAN_POINT ( 'NONE',  ( 11.50505501463289626, -13.50304080202293555, -1.500000000000000000 ) ) ;
#11922 = ADVANCED_FACE ( 'NONE', ( #24822 ), #16955, .F. ) ;
#11921 = ORIENTED_EDGE ( 'NONE', *, *, #11145, .T. ) ;
#11920 = CARTESIAN_POINT ( 'NONE',  ( 107.4506475752643553, -17.36872507146703626, -4.544694954819969546 ) ) ;
#11923 = DIRECTION ( 'NONE',  ( 0.000000000000000000, 0.4226182617406930020, 0.9063077870366529343 ) ) ;
#11924 = CIRCLE ( 'NONE', #29008, 8.750000000000000000 ) ;
#11925 = AXIS2_PLACEMENT_3D ( 'NONE', #29436, #8534, #16735 ) ;
#11926 = CARTESIAN_POINT ( 'NONE',  ( 7.249760686538667009, -2.318425219014174754, -8.437262856154184476 ) ) ;
#11927 = CARTESIAN_POINT ( 'NONE',  ( 24.23500000136559507, -1.570731468192933633, -2.892927487894330074 ) ) ;
#11928 = APPROVAL_PERSON_ORGANIZATION ( #24886, #12272, #7176 ) ;
#11929 = CARTESIAN_POINT ( 'NONE',  ( 24.80306213860490061, -17.49230408913781787, -1.500000000000000000 ) ) ;
#11930 = DIRECTION ( 'NONE',  ( -1.000000000000000000, -0.000000000000000000, -0.000000000000000000 ) ) ;
#11931 = ORIENTED_EDGE ( 'NONE', *, *, #12794, .F. ) ;
#11932 = CARTESIAN_POINT ( 'NONE',  ( -6.506376978575948655, -0.1572233378491221800, 3.000000000000000000 ) ) ;
#11933 = CARTESIAN_POINT ( 'NONE',  ( 101.6058450947822109, -1.222751074449340614, -0.8125824203206647445 ) ) ;
#11934 = EDGE_CURVE ( 'NONE', #12106, #10302, #2439, .T. ) ;
#11935 = CARTESIAN_POINT ( 'NONE',  ( 3.020080256212049896, -5.680439424464590381, -6.926136578642559272 ) ) ;
#11936 = VERTEX_POINT ( 'NONE', #22160 ) ;
#11937 = ADVANCED_FACE ( 'NONE', ( #4756 ), #28356, .T. ) ;
#11938 =( BOUNDED_CURVE ( )  B_SPLINE_CURVE ( 2, ( #2101, #20013, #7127, #24990, #19826, #22496, #27518, #27168, #30208, #4273, #19662 ),
 .UNSPECIFIED., .F., .F. ) 
 B_SPLINE_CURVE_WITH_KNOTS ( ( 3, 2, 2, 2, 2, 3 ),
 ( 0.6228822619934377691, 0.6250000000000000000, 0.6406250000000000000, 0.6562500000000000000, 0.6718750000000000000, 0.6853822619934377691 ),
 .UNSPECIFIED. ) 
 CURVE ( )  GEOMETRIC_REPRESENTATION_ITEM ( )  RATIONAL_B_SPLINE_CURVE ( ( 0.9821626249036861100, 0.9896829947469995004, 1.000000000000000000, 0.9238795325112867385, 1.000000000000000000, 0.9238795325112867385, 1.000000000000000000, 0.9238795325112867385, 1.000000000000000000, 0.9341965377642872381, 0.9821626249036861100 ) ) 
 REPRESENTATION_ITEM ( '' )  );
#11939 = AXIS2_PLACEMENT_3D ( 'NONE', #16086, #23795, #21284 ) ;
#11940 = EDGE_CURVE ( 'NONE', #15458, #13197, #17306, .T. ) ;
#11941 = AXIS2_PLACEMENT_3D ( 'NONE', #11479, #21673, #20775 ) ;
#11942 = CARTESIAN_POINT ( 'NONE',  ( 2.437082531750065950, -7.214115859539295350, 7.858345965138763489 ) ) ;
#11943 = ORIENTED_EDGE ( 'NONE', *, *, #7888, .F. ) ;
#11944 = EDGE_LOOP ( 'NONE', ( #24247, #13533, #11411, #12998 ) ) ;
#11945 = AXIS2_PLACEMENT_3D ( 'NONE', #17628, #11979, #4951 ) ;
#11946 = VECTOR ( 'NONE', #27556, 1000.000000000000000 ) ;
#11947 = ORIENTED_EDGE ( 'NONE', *, *, #10579, .T. ) ;
#11948 = CARTESIAN_POINT ( 'NONE',  ( -2.972652642344170371, -0.1886749676218029415, 1.397177942464156608 ) ) ;
#11950 = EDGE_LOOP ( 'NONE', ( #4562, #1046, #31431, #5687 ) ) ;
#11949 = CARTESIAN_POINT ( 'NONE',  ( 2.970200481232436740, -4.917777846806421493, 7.729547851449619422 ) ) ;
#11951 = VERTEX_POINT ( 'NONE', #5422 ) ;
#11952 = CARTESIAN_POINT ( 'NONE',  ( 21.54750000136559507, 3.024605502323846729, -0.3178988483021056854 ) ) ;
#11953 = LOCAL_TIME ( 16, 7, 10.00000000000000000, #25218 ) ;
#11954 = ORIENTED_EDGE ( 'NONE', *, *, #29748, .T. ) ;
#11955 = CARTESIAN_POINT ( 'NONE',  ( 108.1300413742128228, -19.94772548867836193, -1.389623142575152848 ) ) ;
#11956 = CARTESIAN_POINT ( 'NONE',  ( -4.317168503051449946, -7.715934794172482292, -1.500000000000000000 ) ) ;
#11958 = EDGE_LOOP ( 'NONE', ( #1342, #13504, #2291, #27387 ) ) ;
#11957 = DIRECTION ( 'NONE',  ( 1.000000000000000000, 0.000000000000000000, 0.000000000000000000 ) ) ;
#11959 = DIRECTION ( 'NONE',  ( -1.000000000000000000, -0.000000000000000000, -0.000000000000000000 ) ) ;
#11960 = CARTESIAN_POINT ( 'NONE',  ( -1.762942409646513164, -5.022711880624455567E-15, 2.999999999999999556 ) ) ;
#11961 = DIRECTION ( 'NONE',  ( 1.000000000000000000, -0.000000000000000000, -0.000000000000000000 ) ) ;
#11962 = CARTESIAN_POINT ( 'NONE',  ( 25.36000000136559862, 0.9349337715887185984, -3.156283516753368268 ) ) ;
#11963 = FACE_OUTER_BOUND ( 'NONE', #16790, .T. ) ;
#11964 = VECTOR ( 'NONE', #32064, 1000.000000000000114 ) ;
#11965 = CARTESIAN_POINT ( 'NONE',  ( -2.386718424894326063, -9.330009425477191698, -4.522129901861166701 ) ) ;
#11966 = PLANE ( 'NONE',  #2230 ) ;
#11967 = DIRECTION ( 'NONE',  ( -2.219124775574878265E-17, -0.2588190451025149663, -0.9659258262890698665 ) ) ;
#11968 = EDGE_CURVE ( 'NONE', #19129, #31349, #4478, .T. ) ;
#11969 = CARTESIAN_POINT ( 'NONE',  ( -5.061877160328744907, 19.51744974835124324, -5.285536848417983435 ) ) ;
#11970 = DIRECTION ( 'NONE',  ( -1.000000000000000000, 0.000000000000000000, 0.000000000000000000 ) ) ;
#11971 = LINE ( 'NONE', #19324, #32164 ) ;
#11972 = APPROVAL_PERSON_ORGANIZATION ( #7947, #32320, #5627 ) ;
#11973 = CARTESIAN_POINT ( 'NONE',  ( 5.240875073191910261, 0.000000000000000000, 3.405250132838362642 ) ) ;
#11974 = CARTESIAN_POINT ( 'NONE',  ( -6.200050802731188249, -0.9222479816126459840, -3.113457007523259268 ) ) ;
#11975 = ORIENTED_EDGE ( 'NONE', *, *, #15680, .T. ) ;
#11976 = EDGE_CURVE ( 'NONE', #3357, #30805, #3099, .T. ) ;
#11977 = CARTESIAN_POINT ( 'NONE',  ( -3.950050800000000084, -3.113457007523259268, 0.9222479816126455399 ) ) ;
#11978 = DIRECTION ( 'NONE',  ( 0.000000000000000000, 0.000000000000000000, 1.000000000000000000 ) ) ;
#11979 = DIRECTION ( 'NONE',  ( -0.000000000000000000, 0.000000000000000000, 1.000000000000000000 ) ) ;
#11980 = ORIENTED_EDGE ( 'NONE', *, *, #5999, .F. ) ;
#11981 = CARTESIAN_POINT ( 'NONE',  ( 10.56183597391177464, 0.2499999999999808209, 5.003758587302149508 ) ) ;
#11982 = CARTESIAN_POINT ( 'NONE',  ( 3.249999999999999556, 0.000000000000000000, 0.000000000000000000 ) ) ;
#11983 = ORIENTED_EDGE ( 'NONE', *, *, #2916, .T. ) ;
#11984 = CARTESIAN_POINT ( 'NONE',  ( 0.000000000000000000, 0.000000000000000000, 0.000000000000000000 ) ) ;
#11985 = PERSON_AND_ORGANIZATION_ROLE ( 'classification_officer' ) ;
#11986 = CARTESIAN_POINT ( 'NONE',  ( 3.063284526839887167, 0.000000000000000000, 0.000000000000000000 ) ) ;
#11987 = ORIENTED_EDGE ( 'NONE', *, *, #31684, .T. ) ;
#11988 = CARTESIAN_POINT ( 'NONE',  ( -4.547415420290301213, -6.122835645405422689, 1.499999999999999778 ) ) ;
#11989 = CARTESIAN_POINT ( 'NONE',  ( 102.3922829939881325, -3.552157972614133907, -4.312042181587000478 ) ) ;
#11990 = CARTESIAN_POINT ( 'NONE',  ( 5.377543748152550762, -1.391664247347281780, 7.892520144992429820 ) ) ;
#11991 = CARTESIAN_POINT ( 'NONE',  ( -3.135269660805078740, -0.5000000000000000000, -1.500000000000000000 ) ) ;
#11992 = ORIENTED_EDGE ( 'NONE', *, *, #22437, .F. ) ;
#11993 = CC_DESIGN_SECURITY_CLASSIFICATION ( #8747, ( #1824 ) ) ;
#11994 = CARTESIAN_POINT ( 'NONE',  ( 56.97280603064898941, -277.2763395528616002, 0.000000000000000000 ) ) ;
#11995 = DIRECTION ( 'NONE',  ( 8.574039729943018344E-17, 1.000000000000000000, 0.000000000000000000 ) ) ;
#11996 = CARTESIAN_POINT ( 'NONE',  ( 101.7460786050199033, -3.242078736165208586, 4.282223226228373036 ) ) ;
#11998 = ORIENTED_EDGE ( 'NONE', *, *, #2496, .F. ) ;
#11997 = CARTESIAN_POINT ( 'NONE',  ( 25.62966469407293602, 1.793355229293301489, -2.284851768092018176 ) ) ;
#11999 = CARTESIAN_POINT ( 'NONE',  ( -3.936147556303791983, 18.00000000000000355, 4.854816414140053382 ) ) ;
#12000 = EDGE_CURVE ( 'NONE', #25815, #31589, #9669, .T. ) ;
#12001 = CARTESIAN_POINT ( 'NONE',  ( 41.43141396789281572, -2.886852813804338780, -0.07017451552781628354 ) ) ;
#12002 = LINE ( 'NONE', #4639, #21493 ) ;
#12003 = CARTESIAN_POINT ( 'NONE',  ( 26.08945412691624099, 19.05746434167065928, 1.050000000000000044 ) ) ;
#12004 = DIRECTION ( 'NONE',  ( 1.000000000000000000, -0.000000000000000000, -0.000000000000000000 ) ) ;
#12005 = ADVANCED_FACE ( 'NONE', ( #269 ), #13111, .T. ) ;
#12006 = CARTESIAN_POINT ( 'NONE',  ( 0.000000000000000000, 0.000000000000000000, 0.000000000000000000 ) ) ;
#12007 = AXIS2_PLACEMENT_3D ( 'NONE', #1057, #21939, #13899 ) ;
#12008 = CARTESIAN_POINT ( 'NONE',  ( 25.36146786571785583, -17.53026108976559527, -1.090855922821712731 ) ) ;
#12009 = CARTESIAN_POINT ( 'NONE',  ( -2.506376978575949099, -0.1572233378491262878, 2.999999999999999556 ) ) ;
#12010 = CARTESIAN_POINT ( 'NONE',  ( -26.58934670263598932, 4.786513315057209894, 2.124342492591765996 ) ) ;
#12011 = EDGE_LOOP ( 'NONE', ( #10517, #10740, #5444, #10872 ) ) ;
#12012 = EDGE_CURVE ( 'NONE', #12213, #5578, #4892, .T. ) ;
#12013 = EDGE_CURVE ( 'NONE', #545, #2120, #28655, .T. ) ;
#12014 = CARTESIAN_POINT ( 'NONE',  ( 20.61000000273118715, -1.573300977624594976, 1.942864903642425700 ) ) ;
#12015 = ORIENTED_EDGE ( 'NONE', *, *, #21807, .T. ) ;
#12016 = CARTESIAN_POINT ( 'NONE',  ( -8.354531657079157014, 3.105402419394639235, -0.9198621039125850496 ) ) ;
#12017 = EDGE_CURVE ( 'NONE', #22797, #17929, #6468, .T. ) ;
#12018 = FACE_OUTER_BOUND ( 'NONE', #4697, .T. ) ;
#12019 = CARTESIAN_POINT ( 'NONE',  ( 2.589203020517547582, 8.895471158038725790, -5.222514179739403239 ) ) ;
#12020 = LINE ( 'NONE', #19699, #30100 ) ;
#12021 = ORIENTED_EDGE ( 'NONE', *, *, #21682, .T. ) ;
#12022 = DIRECTION ( 'NONE',  ( -0.000000000000000000, -0.000000000000000000, -1.000000000000000000 ) ) ;
#12023 = ORIENTED_EDGE ( 'NONE', *, *, #3089, .F. ) ;
#12024 = APPROVAL_ROLE ( '' ) ;
#12025 = CARTESIAN_POINT ( 'NONE',  ( 102.4221483139552191, -3.983281035618068344, 4.018750258902361594 ) ) ;
#12026 = EDGE_CURVE ( 'NONE', #21233, #28961, #10859, .T. ) ;
#12027 = CARTESIAN_POINT ( 'NONE',  ( 107.4500593345382811, -17.36019228850094720, 4.522129901861156931 ) ) ;
#12029 = PLANE ( 'NONE',  #2805 ) ;
#12028 = CARTESIAN_POINT ( 'NONE',  ( 6.530491712438077023, 3.778856441136722477, 7.792522225867655195 ) ) ;
#12030 = ORIENTED_EDGE ( 'NONE', *, *, #1911, .T. ) ;
#12031 = ORIENTED_EDGE ( 'NONE', *, *, #10654, .F. ) ;
#12032 = DIRECTION ( 'NONE',  ( 0.000000000000000000, -0.2588190451025184080, -0.9659258262890689783 ) ) ;
#12033 = CARTESIAN_POINT ( 'NONE',  ( -2.362550801365593589, 2.752080473201636845, -2.228590825266444142 ) ) ;
#12034 = CARTESIAN_POINT ( 'NONE',  ( 25.42249999999999943, -2.378061970571983430, 1.291182301015471712 ) ) ;
#12035 = CARTESIAN_POINT ( 'NONE',  ( 0.6082178693771017608, -7.500533726306640503, -1.499999999999999556 ) ) ;
#12037 = ORIENTED_EDGE ( 'NONE', *, *, #19635, .T. ) ;
#12036 = DIRECTION ( 'NONE',  ( -1.000000000000000000, 0.000000000000000000, 0.000000000000000000 ) ) ;
#12038 = CARTESIAN_POINT ( 'NONE',  ( -3.337550801365593678, 1.828967928396027176, -3.368539882008727115 ) ) ;
#12039 = DIRECTION ( 'NONE',  ( 1.000000000000000000, 0.000000000000000000, 0.000000000000000000 ) ) ;
#12040 = CARTESIAN_POINT ( 'NONE',  ( 85.08949032934707191, -1.315411135598756553, 0.07017451552782173751 ) ) ;
#12041 = CARTESIAN_POINT ( 'NONE',  ( 108.0597073579235570, -18.92913321739595744, -4.563813387244610276 ) ) ;
#12042 = ORIENTED_EDGE ( 'NONE', *, *, #5574, .T. ) ;
#12044 = ORIENTED_EDGE ( 'NONE', *, *, #28333, .T. ) ;
#12043 = FACE_OUTER_BOUND ( 'NONE', #25123, .T. ) ;
#12045 = CARTESIAN_POINT ( 'NONE',  ( 107.4385791398478744, 17.85938043952733878, 4.629213727441584325 ) ) ;
#12046 = FACE_OUTER_BOUND ( 'NONE', #896, .T. ) ;
#12047 = EDGE_CURVE ( 'NONE', #22885, #29923, #10874, .T. ) ;
#12048 = EDGE_CURVE ( 'NONE', #21127, #17768, #21138, .T. ) ;
#12049 = CARTESIAN_POINT ( 'NONE',  ( -21.80695521468690146, 18.27315738579030935, 1.777518634817766063 ) ) ;
#12050 = CARTESIAN_POINT ( 'NONE',  ( -28.85861747572623059, 15.66456206417216102, 1.840856759657213848 ) ) ;
#12051 = CARTESIAN_POINT ( 'NONE',  ( 3.503099671769901224, -17.24542532612569445, -1.499999999999682920 ) ) ;
#12052 = LINE ( 'NONE', #9873, #5514 ) ;
#12053 = CARTESIAN_POINT ( 'NONE',  ( 54.90853374638842865, -4.039626021003883238, 1.873789188464484390 ) ) ;
#12054 = CARTESIAN_POINT ( 'NONE',  ( -3.687550801365593323, -2.752080473201636845, 2.228590825266444586 ) ) ;
#12055 = EDGE_LOOP ( 'NONE', ( #28678, #2556, #3942, #26905, #25896 ) ) ;
#12056 = EDGE_CURVE ( 'NONE', #16695, #6314, #11407, .T. ) ;
#12057 = CARTESIAN_POINT ( 'NONE',  ( 0.000000000000000000, 10.82112760146738850, -1.975651141462128280 ) ) ;
#12058 = ORIENTED_EDGE ( 'NONE', *, *, #14434, .T. ) ;
#12059 = B_SPLINE_CURVE_WITH_KNOTS ( 'NONE', 3,
 ( #25096, #17270, #24942, #27115, #4570, #14744, #2055, #2214 ),
 .UNSPECIFIED., .F., .F.,
 ( 4, 2, 2, 4 ),
 ( 2.213836054482316663E-07, 0.001261154818855362647, 0.001891621536480320902, 0.002522088254105278940 ),
 .UNSPECIFIED. ) ;
#12060 = CARTESIAN_POINT ( 'NONE',  ( 109.2693081351234241, 19.58869392272333343, 0.4463807625373348298 ) ) ;
#12061 = CARTESIAN_POINT ( 'NONE',  ( 10.00000000000000000, -4.467071865485483961, 1.625881193364682842 ) ) ;
#12062 = CYLINDRICAL_SURFACE ( 'NONE', #24071, 6.248999999999999666 ) ;
#12063 = ORIENTED_EDGE ( 'NONE', *, *, #1444, .F. ) ;
#12064 = EDGE_CURVE ( 'NONE', #3656, #24705, #4073, .T. ) ;
#12065 = CARTESIAN_POINT ( 'NONE',  ( 20.66542725970865746, -21.74162791314449805, 1.399019267719741499 ) ) ;
#12066 = ORIENTED_EDGE ( 'NONE', *, *, #5328, .F. ) ;
#12067 = DIRECTION ( 'NONE',  ( 0.005016709653754843068, -0.9993908270190956511, -0.03453704524619621158 ) ) ;
#12069 = EDGE_LOOP ( 'NONE', ( #7792, #9794, #31882, #20924 ) ) ;
#12068 = CARTESIAN_POINT ( 'NONE',  ( 54.94551756700143841, -5.360949955573579118, -3.995970705067843909 ) ) ;
#12070 = VERTEX_POINT ( 'NONE', #11085 ) ;
#12071 = CARTESIAN_POINT ( 'NONE',  ( 2.736976356551361622, -8.480777311736980906, 5.155436092272288384 ) ) ;
#12072 = CARTESIAN_POINT ( 'NONE',  ( 102.5829460782277351, -0.8583298743146012821, 2.713652344655541615 ) ) ;
#12074 = ORIENTED_EDGE ( 'NONE', *, *, #3476, .T. ) ;
#12073 = CARTESIAN_POINT ( 'NONE',  ( 107.4196074183075638, -16.92202192504116809, 3.623753903136544885 ) ) ;
#12075 = CARTESIAN_POINT ( 'NONE',  ( 26.23135861748343700, 19.12135596485594746, -1.050000000000000044 ) ) ;
#12076 = CARTESIAN_POINT ( 'NONE',  ( 8.914564461877821699, -1.485434449214014388E-07, -1.044418714689423711 ) ) ;
#12077 = CARTESIAN_POINT ( 'NONE',  ( -3.789033621533670182, -3.338956497497331366, 1.747105405493127428 ) ) ;
#12078 = CARTESIAN_POINT ( 'NONE',  ( 2.274274201625327230, 10.82112760146739028, -1.975651141462127391 ) ) ;
#12080 = ORIENTED_EDGE ( 'NONE', *, *, #12206, .F. ) ;
#12079 = CARTESIAN_POINT ( 'NONE',  ( 107.9822453661852393, -17.81369980648333851, -4.398297061781460293 ) ) ;
#12081 = DIRECTION ( 'NONE',  ( 1.000000000000000000, 5.361488761196502513E-16, -0.000000000000000000 ) ) ;
#12082 = DIRECTION ( 'NONE',  ( -1.000000000000000000, -0.000000000000000000, -0.000000000000000000 ) ) ;
#12083 = DIRECTION ( 'NONE',  ( 0.000000000000000000, 0.9510565162951544194, -0.3090169943749449533 ) ) ;
#12084 = ADVANCED_FACE ( 'NONE', ( #8414 ), #31665, .T. ) ;
#12085 = CARTESIAN_POINT ( 'NONE',  ( 3.249999999999999556, 8.264486777890107660, 4.472189673936814991 ) ) ;
#12086 = CARTESIAN_POINT ( 'NONE',  ( 3.499999999999999556, -6.200809695932780308, 0.7745709230444962623 ) ) ;
#12087 = PLANE ( 'NONE',  #25229 ) ;
#12088 = ORIENTED_EDGE ( 'NONE', *, *, #3496, .T. ) ;
#12089 = DIRECTION ( 'NONE',  ( -0.9896144216807905014, -0.000000000000000000, -0.1437473352845004826 ) ) ;
#12090 = CYLINDRICAL_SURFACE ( 'NONE', #19330, 11.00000000000000000 ) ;
#12091 = CARTESIAN_POINT ( 'NONE',  ( -6.887550801365593500, -2.752080473201636845, 2.228590825266444586 ) ) ;
#12092 = EDGE_LOOP ( 'NONE', ( #14237, #20173, #12477, #9151 ) ) ;
#12093 = DIRECTION ( 'NONE',  ( 1.000000000000000000, -8.574039729943018344E-17, -0.000000000000000000 ) ) ;
#12094 = CARTESIAN_POINT ( 'NONE',  ( 40.91321928711694511, -19.30714377375492674, -0.9788672205888330202 ) ) ;
#12095 = ORIENTED_EDGE ( 'NONE', *, *, #11023, .F. ) ;
#12096 = CARTESIAN_POINT ( 'NONE',  ( 108.2840637929470091, 19.75993920999055931, 3.584100151297118231 ) ) ;
#12097 = EDGE_LOOP ( 'NONE', ( #20982, #197, #17081, #1860 ) ) ;
#12098 = EDGE_CURVE ( 'NONE', #24740, #21393, #12453, .T. ) ;
#12099 = CC_DESIGN_PERSON_AND_ORGANIZATION_ASSIGNMENT ( #3529, #8206, ( #12467 ) ) ;
#12100 = ORIENTED_EDGE ( 'NONE', *, *, #31328, .T. ) ;
#12101 = CARTESIAN_POINT ( 'NONE',  ( 4.749760686538667009, 6.139290821770327256, -5.151476664237414127 ) ) ;
#12103 = ORIENTED_EDGE ( 'NONE', *, *, #7676, .T. ) ;
#12102 = DIRECTION ( 'NONE',  ( 0.000000000000000000, 0.000000000000000000, 1.000000000000000000 ) ) ;
#12104 = VERTEX_POINT ( 'NONE', #29295 ) ;
#12105 = CARTESIAN_POINT ( 'NONE',  ( 23.79750000136559507, 0.3178988483021036315, 3.024605502323848949 ) ) ;
#12106 = VERTEX_POINT ( 'NONE', #24434 ) ;
#12107 = DIRECTION ( 'NONE',  ( 1.000000000000000000, -8.574039729943018344E-17, -0.000000000000000000 ) ) ;
#12109 = ORIENTED_EDGE ( 'NONE', *, *, #24301, .F. ) ;
#12108 = DIRECTION ( 'NONE',  ( -0.000000000000000000, -0.000000000000000000, -1.000000000000000000 ) ) ;
#12110 = CARTESIAN_POINT ( 'NONE',  ( -56.35010546049321789, 0.004916966322057593312, -1.004378502258694628 ) ) ;
#12111 = B_SPLINE_CURVE_WITH_KNOTS ( 'NONE', 3,
 ( #20212, #22727, #22555, #5167, #33079, #10156, #10347, #22876, #30408, #2504 ),
 .UNSPECIFIED., .F., .F.,
 ( 4, 2, 2, 2, 4 ),
 ( 0.000000000000000000, 0.0004294301528457186799, 0.0008588603056914373597, 0.001288290458537156040, 0.001717720611382874719 ),
 .UNSPECIFIED. ) ;
#12112 = CARTESIAN_POINT ( 'NONE',  ( 102.6609843814833027, -1.982062027707615526, -4.522129901861162260 ) ) ;
#12113 = CARTESIAN_POINT ( 'NONE',  ( 22.54750000136559507, 3.024605502323846729, -0.3178988483021056854 ) ) ;
#12114 = CARTESIAN_POINT ( 'NONE',  ( 107.6648144168582775, -20.46701934092494568, 1.481717219550688913 ) ) ;
#12115 = EDGE_CURVE ( 'NONE', #26383, #22729, #3581, .T. ) ;
#12116 = EDGE_CURVE ( 'NONE', #15020, #18257, #29550, .T. ) ;
#12117 = CARTESIAN_POINT ( 'NONE',  ( 42.67399297346870668, -22.27808837056542046, -5.485967528433938867 ) ) ;
#12118 = FACE_OUTER_BOUND ( 'NONE', #27101, .T. ) ;
#12119 = CARTESIAN_POINT ( 'NONE',  ( 25.41068576271580781, -17.53965252855324053, 1.057866664602795437 ) ) ;
#12120 = CARTESIAN_POINT ( 'NONE',  ( 17.84081991000783418, -19.48375781953046371, 5.485967528433935314 ) ) ;
#12121 = CARTESIAN_POINT ( 'NONE',  ( -5.561021557437524798, 7.493231324518994541, -2.854557343487579502 ) ) ;
#12122 = CARTESIAN_POINT ( 'NONE',  ( 35.23476908784418526, -3.791088091780328906, 0.07017451550800198057 ) ) ;
#12123 = CARTESIAN_POINT ( 'NONE',  ( 18.68265047573912341, -6.724553502642427461, 4.522129901861163148 ) ) ;
#12124 = CARTESIAN_POINT ( 'NONE',  ( -4.900050802731187538, -1.549418761218565477, 2.853674364686380471 ) ) ;
#12125 = VERTEX_POINT ( 'NONE', #31337 ) ;
#12126 = CARTESIAN_POINT ( 'NONE',  ( -2.900050800000000706, 0.3135853898029611342, -2.983565686104819648 ) ) ;
#12127 = CARTESIAN_POINT ( 'NONE',  ( -34.98193025661426248, 0.5174497483512505713, -2.482234843104711430 ) ) ;
#12128 = CARTESIAN_POINT ( 'NONE',  ( -0.000000000000000000, 0.5000000000000000000, -1.000000000000000000 ) ) ;
#12129 = VERTEX_POINT ( 'NONE', #31826 ) ;
#12130 = LINE ( 'NONE', #7282, #2129 ) ;
#12131 = CARTESIAN_POINT ( 'NONE',  ( 2.864531314636033610, 7.330015575757897750, 6.140839842381188518 ) ) ;
#12132 = ORIENTED_EDGE ( 'NONE', *, *, #29979, .T. ) ;
#12133 = CARTESIAN_POINT ( 'NONE',  ( 2.990360172271274486, 7.668143846948784592, 4.902036888218493260 ) ) ;
#12134 = PERSON_AND_ORGANIZATION_ROLE ( 'design_owner' ) ;
#12135 = CARTESIAN_POINT ( 'NONE',  ( 0.000000000000000000, 0.000000000000000000, 0.000000000000000000 ) ) ;
#12136 = ORIENTED_EDGE ( 'NONE', *, *, #32790, .F. ) ;
#12137 = CARTESIAN_POINT ( 'NONE',  ( 9.295344188488364523, -0.03282880342717523631, -1.183647805826461674 ) ) ;
#12138 = DIRECTION ( 'NONE',  ( 1.000000000000000000, -0.000000000000000000, 0.000000000000000000 ) ) ;
#12139 = CARTESIAN_POINT ( 'NONE',  ( 28.66985322744200815, -6.539611658422689544, -4.215290389460269793 ) ) ;
#12140 = CARTESIAN_POINT ( 'NONE',  ( -50.60000000000000142, -10.96966150227468972, 0.9999999999999991118 ) ) ;
#12141 = CARTESIAN_POINT ( 'NONE',  ( 10.57125986779756843, 0.8254815157535241310, 4.681538312723519724 ) ) ;
#12142 =( BOUNDED_SURFACE ( )  B_SPLINE_SURFACE ( 3, 2, ( 
 ( #11646, #14304, #4485 ),
 ( #22193, #16485, #24684 ),
 ( #10085, #1812, #6799 ),
 ( #16986, #27186, #24502 ),
 ( #1624, #9463, #22021 ),
 ( #19679, #6956, #14659 ),
 ( #24855, #2437, #30508 ),
 ( #8964, #32054, #19355 ),
 ( #2589, #28152, #21135 ),
 ( #28308, #15926, #13406 ),
 ( #28002, #18112, #30999 ),
 ( #8266, #28652, #5602 ) ),
 .UNSPECIFIED., .F., .F., .F. ) 
 B_SPLINE_SURFACE_WITH_KNOTS ( ( 4, 2, 2, 2, 2, 4 ),
 ( 3, 3 ),
 ( 0.01237460209466449690, 0.01250742172631360075, 0.01264024135796270286, 0.01290588062126090882, 0.01343715914785732247, 0.01449971620105014805 ),
 ( 0.000000000000000000, 1.000000000000000000 ),
 .UNSPECIFIED. ) 
 GEOMETRIC_REPRESENTATION_ITEM ( )  RATIONAL_B_SPLINE_SURFACE ( (
 ( 1.000000000000000000, 0.9985794324048127280, 1.000000000000000000),
 ( 1.000000000000000000, 0.9985649967291553297, 1.000000000000000000),
 ( 1.000000000000000000, 0.9977546568864327226, 1.000000000000000000),
 ( 1.000000000000000000, 0.9959318651690590718, 1.000000000000000000),
 ( 1.000000000000000000, 0.9948682866525003776, 1.000000000000000000),
 ( 1.000000000000000000, 0.9916149370760384274, 1.000000000000000000),
 ( 1.000000000000000000, 0.9892930324833787425, 1.000000000000000000),
 ( 1.000000000000000000, 0.9821212088646953386, 1.000000000000000000),
 ( 1.000000000000000000, 0.9771237707448936494, 1.000000000000000000),
 ( 1.000000000000000000, 0.9616790524996320366, 1.000000000000000000),
 ( 1.000000000000000000, 0.9507373671942048743, 1.000000000000000000),
 ( 1.000000000000000000, 0.9391581256477382622, 1.000000000000000000) ) ) 
 REPRESENTATION_ITEM ( '' )  SURFACE ( )  );
#12143 = VERTEX_POINT ( 'NONE', #13589 ) ;
#12144 = EDGE_CURVE ( 'NONE', #10538, #26682, #14466, .T. ) ;
#12145 = CARTESIAN_POINT ( 'NONE',  ( 21.47444597020330193, -21.75444421693962482, -1.464466272521893098 ) ) ;
#12146 = PLANE ( 'NONE',  #2875 ) ;
#12147 = ADVANCED_FACE ( 'NONE', ( #16770 ), #16417, .T. ) ;
#12149 = EDGE_LOOP ( 'NONE', ( #836, #26040, #7315, #23333 ) ) ;
#12148 = CARTESIAN_POINT ( 'NONE',  ( -10.00000000000000000, 0.000000000000000000, 0.000000000000000000 ) ) ;
#12150 = PLANE ( 'NONE',  #16184 ) ;
#12151 = CARTESIAN_POINT ( 'NONE',  ( -50.60000000000000142, 0.000000000000000000, 1.500000000000000000 ) ) ;
#12152 = DIRECTION ( 'NONE',  ( 0.4999999999999977796, 0.8660254037844398178, 0.000000000000000000 ) ) ;
#12153 = DIRECTION ( 'NONE',  ( -0.1413077769430314268, 0.9899657126261587337, 0.000000000000000000 ) ) ;
#12154 = CARTESIAN_POINT ( 'NONE',  ( 85.13613392229179055, -2.069934983084471103, -2.713652344655540727 ) ) ;
#12155 = CARTESIAN_POINT ( 'NONE',  ( -8.000050800000003903, 3.519328457705152235, 0.3516833816935649448 ) ) ;
#12156 = CARTESIAN_POINT ( 'NONE',  ( 6.530491751506347420, -6.216163082443024734, -6.030130624359239633 ) ) ;
#12157 = DIRECTION ( 'NONE',  ( 2.473959037481237219E-13, 1.000000000000000000, -0.000000000000000000 ) ) ;
#12158 = CARTESIAN_POINT ( 'NONE',  ( 4.749760686538667009, 8.385837730238846314E-14, -8.014274990069656823 ) ) ;
#12159 = ORIENTED_EDGE ( 'NONE', *, *, #31043, .F. ) ;
#12160 = CARTESIAN_POINT ( 'NONE',  ( 20.92250000273118715, -1.291182301015472600, -2.378061970571982098 ) ) ;
#12161 = VERTEX_POINT ( 'NONE', #11732 ) ;
#12162 = CARTESIAN_POINT ( 'NONE',  ( -5.304531657079158080, 0.3127741368606810068, -2.975847129947406522 ) ) ;
#12163 = CARTESIAN_POINT ( 'NONE',  ( 24.98500000136559507, -0.9349337715887248157, 3.156283516753367824 ) ) ;
#12164 = CARTESIAN_POINT ( 'NONE',  ( 48.05280571049738825, -6.817569152029394175, -5.695980980372493008 ) ) ;
#12165 = CARTESIAN_POINT ( 'NONE',  ( 3.249999999999999556, 1.239665997526887109, 9.314797388894895391 ) ) ;
#12166 = CARTESIAN_POINT ( 'NONE',  ( -12.44989959798873791, 0.4999999999999998890, -12.99999999999999645 ) ) ;
#12167 = ORIENTED_EDGE ( 'NONE', *, *, #12269, .T. ) ;
#12168 = CARTESIAN_POINT ( 'NONE',  ( 21.40255435829265451, -21.75563089608565903, 1.444450440414875692 ) ) ;
#12169 = EDGE_CURVE ( 'NONE', #9705, #19878, #24286, .T. ) ;
#12170 = ORIENTED_EDGE ( 'NONE', *, *, #267, .T. ) ;
#12171 = DATE_TIME_ROLE ( 'classification_date' ) ;
#12172 = CARTESIAN_POINT ( 'NONE',  ( 85.03499643008539977, -5.191404901269152106, 4.013697181026976146 ) ) ;
#12173 = ADVANCED_FACE ( 'NONE', ( #21772 ), #11245, .T. ) ;
#12174 = CARTESIAN_POINT ( 'NONE',  ( -23.35000000000000142, -10.96966150227469505, 4.500000000000000888 ) ) ;
#12176 = FACE_OUTER_BOUND ( 'NONE', #21680, .T. ) ;
#12175 = DIRECTION ( 'NONE',  ( 0.000000000000000000, 0.000000000000000000, -1.000000000000000000 ) ) ;
#12177 = ORIENTED_EDGE ( 'NONE', *, *, #18920, .T. ) ;
#12178 = DIRECTION ( 'NONE',  ( -1.000000000000000000, 0.000000000000000000, 0.000000000000000000 ) ) ;
#12179 = CARTESIAN_POINT ( 'NONE',  ( 25.75999999999999801, -2.208672634433321348E-15, 0.000000000000000000 ) ) ;
#12180 = CARTESIAN_POINT ( 'NONE',  ( 25.61000000136559507, 2.892927487894327410, -1.570731468192931635 ) ) ;
#12181 = CARTESIAN_POINT ( 'NONE',  ( 4.832428952779699749, -12.72822366752450307, -1.499999999999158451 ) ) ;
#12183 = ORIENTED_EDGE ( 'NONE', *, *, #1183, .T. ) ;
#12182 = CARTESIAN_POINT ( 'NONE',  ( 6.530491482054475050, 8.615020591497813740, -0.8857639883442027795 ) ) ;
#12184 = CARTESIAN_POINT ( 'NONE',  ( -4.787550801365593856, 3.521866450007987037, 0.3701630799359328372 ) ) ;
#12185 = CARTESIAN_POINT ( 'NONE',  ( -29.85000000000000497, -10.96966150227469505, -11.00000000000000000 ) ) ;
#12186 = EDGE_CURVE ( 'NONE', #5075, #1352, #26363, .T. ) ;
#12187 = LINE ( 'NONE', #1864, #8123 ) ;
#12188 = CARTESIAN_POINT ( 'NONE',  ( 3.499999999999999556, 4.561279057474472154, -4.271385531633124621 ) ) ;
#12189 = EDGE_LOOP ( 'NONE', ( #10792, #831, #11767, #29132 ) ) ;
#12191 = ORIENTED_EDGE ( 'NONE', *, *, #23302, .F. ) ;
#12190 = CARTESIAN_POINT ( 'NONE',  ( 6.357667975083868050, -7.150591204917362553, -4.790963222208079131 ) ) ;
#12192 = DIRECTION ( 'NONE',  ( -1.000000000000000000, -0.000000000000000000, -0.000000000000000000 ) ) ;
#12193 = DIRECTION ( 'NONE',  ( 0.8660254037844409281, -0.4999999999999960587, 0.000000000000000000 ) ) ;
#12194 = EDGE_CURVE ( 'NONE', #17962, #17857, #14087, .T. ) ;
#12195 = CARTESIAN_POINT ( 'NONE',  ( 24.29750000136559507, -2.363507492473152283, -1.913930629741525280 ) ) ;
#12196 = CARTESIAN_POINT ( 'NONE',  ( -6.400050802731188426, -3.113457007523259268, 0.9222479816126455399 ) ) ;
#12197 = CARTESIAN_POINT ( 'NONE',  ( 5.539315478094516187, -17.99457612246279936, -1.748481423779015609 ) ) ;
#12198 = DIRECTION ( 'NONE',  ( -1.000000000000000000, 8.574039729943018344E-17, -0.000000000000000000 ) ) ;
#12199 = EDGE_CURVE ( 'NONE', #17109, #19335, #19412, .T. ) ;
#12200 = CARTESIAN_POINT ( 'NONE',  ( 35.33972979713486495, -3.946928302550552825, 1.169950777404600739 ) ) ;
#12201 = CARTESIAN_POINT ( 'NONE',  ( 0.5032041927271341253, 7.418882907476129773, 6.298925283824120314 ) ) ;
#12202 = ORIENTED_EDGE ( 'NONE', *, *, #27448, .T. ) ;
#12203 = CARTESIAN_POINT ( 'NONE',  ( 7.249760686538667009, 7.530955069117513112, 2.741043480754951744 ) ) ;
#12204 = VERTEX_POINT ( 'NONE', #907 ) ;
#12205 = CYLINDRICAL_SURFACE ( 'NONE', #20414, 5.010000000000000675 ) ;
#12206 = EDGE_CURVE ( 'NONE', #25095, #2157, #8567, .T. ) ;
#12207 = DIRECTION ( 'NONE',  ( 0.000000000000000000, 0.000000000000000000, 1.000000000000000000 ) ) ;
#12208 = ORIENTED_EDGE ( 'NONE', *, *, #8888, .T. ) ;
#12209 = CYLINDRICAL_SURFACE ( 'NONE', #17658, 297.9387600756452343 ) ;
#12210 = VERTEX_POINT ( 'NONE', #15067 ) ;
#12211 = CARTESIAN_POINT ( 'NONE',  ( -35.00000000000000000, 0.000000000000000000, 3.000000000000004441 ) ) ;
#12213 = VERTEX_POINT ( 'NONE', #30309 ) ;
#12212 = CARTESIAN_POINT ( 'NONE',  ( 28.69339080511027973, -5.623844247569588894, -4.006107076269940670 ) ) ;
#12214 = VERTEX_POINT ( 'NONE', #25286 ) ;
#12215 = EDGE_CURVE ( 'NONE', #5480, #29891, #27773, .T. ) ;
#12216 = EDGE_CURVE ( 'NONE', #26576, #2834, #19636, .T. ) ;
#12217 = DIRECTION ( 'NONE',  ( 0.000000000000000000, 0.000000000000000000, -1.000000000000000000 ) ) ;
#12218 = CARTESIAN_POINT ( 'NONE',  ( 85.48138648428260922, -7.654866896025225742, -1.915219082070897638 ) ) ;
#12220 = ORIENTED_EDGE ( 'NONE', *, *, #22277, .T. ) ;
#12219 = DIRECTION ( 'NONE',  ( 0.000000000000000000, -0.7431448254773862505, -0.6691306063588670083 ) ) ;
#12221 = CARTESIAN_POINT ( 'NONE',  ( 5.377543748152548986, 4.007137495034812424, 6.940565734314612101 ) ) ;
#12222 = CARTESIAN_POINT ( 'NONE',  ( 8.878230740118540965, 3.506306759228156664E-16, -1.080849929302612367 ) ) ;
#12223 = CARTESIAN_POINT ( 'NONE',  ( -3.349881330687049630, -1.984754805279889345, 1.747784029808686412 ) ) ;
#12224 = CARTESIAN_POINT ( 'NONE',  ( 9.134478070376893299, -0.4075412271184362112, -1.000000000000000000 ) ) ;
#12226 = ORIENTED_EDGE ( 'NONE', *, *, #19417, .T. ) ;
#12225 = CARTESIAN_POINT ( 'NONE',  ( 107.9868730121348506, -17.88033675694570945, -4.506462841229693872 ) ) ;
#12227 = CARTESIAN_POINT ( 'NONE',  ( 2.274274201625319236, -9.680994141368833183, 5.222868219166820758 ) ) ;
#12228 = CARTESIAN_POINT ( 'NONE',  ( 23.05656763645045615, 0.8852964313267427388, -2.499999999999999112 ) ) ;
#12229 = CARTESIAN_POINT ( 'NONE',  ( 23.86000000136559507, -0.9349337715887248157, 3.156283516753367824 ) ) ;
#12230 = CARTESIAN_POINT ( 'NONE',  ( 107.4385791398478602, 17.85938043952733878, -4.612695725900422872 ) ) ;
#12231 = ADVANCED_FACE ( 'NONE', ( #27468 ), #25863, .T. ) ;
#12232 = CARTESIAN_POINT ( 'NONE',  ( -35.00000000000000000, 0.000000000000000000, -2.999999999999995559 ) ) ;
#12233 = CARTESIAN_POINT ( 'NONE',  ( -2.715612589025698131, -0.5453662152015711362, -1.748464016170166113 ) ) ;
#12234 = VERTEX_POINT ( 'NONE', #12227 ) ;
#12235 = CARTESIAN_POINT ( 'NONE',  ( 78.40736801748178664, 24.56822898102832653, 4.629213727441585213 ) ) ;
#12236 = DIRECTION ( 'NONE',  ( 0.000000000000000000, 0.000000000000000000, 1.000000000000000000 ) ) ;
#12237 = CARTESIAN_POINT ( 'NONE',  ( -5.337550801365593678, -1.828967928396026732, 3.368539882008728004 ) ) ;
#12238 = ORIENTED_EDGE ( 'NONE', *, *, #24697, .T. ) ;
#12239 = B_SPLINE_CURVE_WITH_KNOTS ( 'NONE', 3,
 ( #19008, #16465, #29194, #28558, #13643, #23694 ),
 .UNSPECIFIED., .F., .F.,
 ( 4, 2, 4 ),
 ( 4.171616645832102339E-14, 0.0003905687335822774888, 0.0007811374671228388895 ),
 .UNSPECIFIED. ) ;
#12240 = EDGE_CURVE ( 'NONE', #14180, #4101, #22619, .T. ) ;
#12241 = LINE ( 'NONE', #25113, #2366 ) ;
#12242 = CARTESIAN_POINT ( 'NONE',  ( 2.632061376486627413, -0.5000000000000007772, -1.500000000000000444 ) ) ;
#12243 = ORIENTED_EDGE ( 'NONE', *, *, #31252, .F. ) ;
#12244 = CARTESIAN_POINT ( 'NONE',  ( 107.8757006203288142, 20.33592830972715504, 2.535883260025156183 ) ) ;
#12245 = EDGE_CURVE ( 'NONE', #29709, #11749, #7696, .T. ) ;
#12246 = ORIENTED_EDGE ( 'NONE', *, *, #10247, .F. ) ;
#12247 = EDGE_LOOP ( 'NONE', ( #28065, #21917, #1732, #6578 ) ) ;
#12248 = CARTESIAN_POINT ( 'NONE',  ( 10.57125986779756843, -4.681538312723512618, -0.8254815157535732029 ) ) ;
#12250 = ORIENTED_EDGE ( 'NONE', *, *, #19952, .T. ) ;
#12249 = LINE ( 'NONE', #30334, #8535 ) ;
#12251 = EDGE_LOOP ( 'NONE', ( #5977, #8849, #15709, #4459 ) ) ;
#12252 = CARTESIAN_POINT ( 'NONE',  ( 22.29750000136559507, -0.3178988483021076838, -3.024605502323848949 ) ) ;
#12253 = EDGE_CURVE ( 'NONE', #20952, #3262, #32268, .T. ) ;
#12254 = EDGE_CURVE ( 'NONE', #12214, #1670, #9230, .T. ) ;
#12255 = ORIENTED_EDGE ( 'NONE', *, *, #2443, .T. ) ;
#12256 = DIRECTION ( 'NONE',  ( 0.000000000000000000, -0.9063077870366482713, 0.4226182617407029940 ) ) ;
#12258 = ORIENTED_EDGE ( 'NONE', *, *, #9644, .F. ) ;
#12257 = CARTESIAN_POINT ( 'NONE',  ( 54.91389575944440793, -4.233367447934999639, -2.184956776131685707 ) ) ;
#12259 = AXIS2_PLACEMENT_3D ( 'NONE', #16060, #8542, #18748 ) ;
#12260 = CARTESIAN_POINT ( 'NONE',  ( 0.000000000000000000, 0.000000000000000000, 0.000000000000000000 ) ) ;
#12261 = CARTESIAN_POINT ( 'NONE',  ( 85.20563808598696198, -3.194259795296082061, -4.522129901861162260 ) ) ;
#12262 = CARTESIAN_POINT ( 'NONE',  ( 25.79750000136559507, 0.3178988483021036315, 3.024605502323848949 ) ) ;
#12263 = CARTESIAN_POINT ( 'NONE',  ( 10.56870887191539587, -1.625881193364669297, -4.467071865485488402 ) ) ;
#12264 = CIRCLE ( 'NONE', #16002, 0.4999999999999995559 ) ;
#12265 = B_SPLINE_CURVE_WITH_KNOTS ( 'NONE', 3,
 ( #21272, #16256, #10577, #11072, #3412, #11226 ),
 .UNSPECIFIED., .F., .F.,
 ( 4, 2, 4 ),
 ( -6.819812922326889058E-06, 0.0003932617828678426023, 0.0007933433786580120200 ),
 .UNSPECIFIED. ) ;
#12266 = CARTESIAN_POINT ( 'NONE',  ( 3.424298583717193057E-16, 3.993798362933351775, -3.024842911000649615 ) ) ;
#12267 = DIRECTION ( 'NONE',  ( 0.000000000000000000, 0.000000000000000000, -1.000000000000000000 ) ) ;
#12268 = CARTESIAN_POINT ( 'NONE',  ( 25.33940588721780784, -17.54454932707527348, 1.176512215458641819 ) ) ;
#12269 = EDGE_CURVE ( 'NONE', #17891, #20953, #15773, .T. ) ;
#12270 = LINE ( 'NONE', #4606, #4348 ) ;
#12271 = CARTESIAN_POINT ( 'NONE',  ( 10.52034268205830259, -3.055657119358826446, 3.641590349731918863 ) ) ;
#12272 = APPROVAL ( #9658, 'UNSPECIFIED' ) ;
#12273 = CARTESIAN_POINT ( 'NONE',  ( 0.000000000000000000, 7.533794289458167981, -7.944914065997031649 ) ) ;
#12274 = DIRECTION ( 'NONE',  ( -1.000000000000000000, -0.000000000000000000, -0.000000000000000000 ) ) ;
#12275 = CARTESIAN_POINT ( 'NONE',  ( 85.38119660045754244, -6.034158634414237277, 4.522129901861163148 ) ) ;
#12276 = CARTESIAN_POINT ( 'NONE',  ( -3.900050802731187982, -2.853674364686378695, -1.549418761218566809 ) ) ;
#12277 = VERTEX_POINT ( 'NONE', #32488 ) ;
#12278 = CARTESIAN_POINT ( 'NONE',  ( -3.650050800000000706, 1.549418761218566143, -2.853674364686379583 ) ) ;
#12279 = VECTOR ( 'NONE', #3992, 1000.000000000000000 ) ;
#12280 = AXIS2_PLACEMENT_3D ( 'NONE', #14118, #12108, #24318 ) ;
#12281 = CARTESIAN_POINT ( 'NONE',  ( 23.20536262852492726, -21.93817978746277220, -1.034581372269383293 ) ) ;
#12282 = CARTESIAN_POINT ( 'NONE',  ( -3.900050802731187982, -2.853674364686378695, -1.549418761218566809 ) ) ;
#12283 = ORIENTED_EDGE ( 'NONE', *, *, #2050, .T. ) ;
#12284 = CARTESIAN_POINT ( 'NONE',  ( -1.850050802731187716, 1.887961173149511618, 2.331437884370912705 ) ) ;
#12285 = SHAPE_REPRESENTATION_RELATIONSHIP ( 'NONE' , 'NONE' ,  #5606, #18723 ) ;
#12286 = EDGE_CURVE ( 'NONE', #28961, #16345, #31733, .T. ) ;
#12287 = AXIS2_PLACEMENT_3D ( 'NONE', #10217, #30659, #7736 ) ;
#12288 = ORIENTED_EDGE ( 'NONE', *, *, #2552, .T. ) ;
#12289 = DIRECTION ( 'NONE',  ( 1.000000000000000000, -8.574039729943018344E-17, -0.000000000000000000 ) ) ;
#12290 = DATE_AND_TIME ( #7286, #21072 ) ;
#12291 = DIRECTION ( 'NONE',  ( 0.000000000000000000, 0.9961946980917454342, 0.08715574274765866547 ) ) ;
#12292 = ORIENTED_EDGE ( 'NONE', *, *, #12642, .F. ) ;
#12293 = CARTESIAN_POINT ( 'NONE',  ( 0.2308133903883674287, -15.52418313443756048, 1.500000000000000666 ) ) ;
#12294 = VERTEX_POINT ( 'NONE', #6732 ) ;
#12295 = DIRECTION ( 'NONE',  ( -0.03488359650710490256, -0.9989355049964836475, 0.03018263660036206442 ) ) ;
#12296 = CARTESIAN_POINT ( 'NONE',  ( 18.80941384712907904, -5.307593421025357472, -4.312042181584450518 ) ) ;
#12297 = CARTESIAN_POINT ( 'NONE',  ( -56.77537022611499395, 0.4514244267945254907, 2.028141679927229379 ) ) ;
#12298 = DIRECTION ( 'NONE',  ( -0.000000000000000000, -0.000000000000000000, -1.000000000000000000 ) ) ;
#12299 = ORIENTED_EDGE ( 'NONE', *, *, #7742, .T. ) ;
#12300 = CARTESIAN_POINT ( 'NONE',  ( 21.73787281414312034, -21.77158151251076035, -1.493747827548021156 ) ) ;
#12301 = CARTESIAN_POINT ( 'NONE',  ( 101.7221769401408551, -2.897900707893039662, 3.993434276071444078 ) ) ;
#12302 = AXIS2_PLACEMENT_3D ( 'NONE', #16233, #26270, #13854 ) ;
#12304 = ORIENTED_EDGE ( 'NONE', *, *, #13414, .T. ) ;
#12303 = CARTESIAN_POINT ( 'NONE',  ( -3.250050802731187183, -2.331437884370912705, 1.887961173149512062 ) ) ;
#12305 = AXIS2_PLACEMENT_3D ( 'NONE', #13542, #30954, #1009 ) ;
#12306 = PLANE ( 'NONE',  #25663 ) ;
#12307 = CARTESIAN_POINT ( 'NONE',  ( -2.786590204610737587, -5.640011313469492471, -4.522129901861166701 ) ) ;
#12308 = FACE_OUTER_BOUND ( 'NONE', #17023, .T. ) ;
#12309 = CARTESIAN_POINT ( 'NONE',  ( 101.6572086713194665, -1.962373798936464242, -2.487845072520846301 ) ) ;
#12310 = AXIS2_PLACEMENT_3D ( 'NONE', #23779, #29128, #31646 ) ;
#12311 = CARTESIAN_POINT ( 'NONE',  ( -8.000050800000002127, 2.629983047553211328, 2.147054542866906779 ) ) ;
#12312 = CARTESIAN_POINT ( 'NONE',  ( 7.064632951172269415, -6.226446564517874371, -6.147671362329281131 ) ) ;
#12313 = CARTESIAN_POINT ( 'NONE',  ( -56.28660922948461121, 0.003949738777827453869, -1.069323361021561558 ) ) ;
#12314 = CARTESIAN_POINT ( 'NONE',  ( 23.13226153066085899, -21.93404782914829809, 1.074068642720903632 ) ) ;
#12315 = EDGE_LOOP ( 'NONE', ( #3918, #17529, #13657, #4704 ) ) ;
#12316 = CARTESIAN_POINT ( 'NONE',  ( -6.312550801365593323, 3.675193018007247403, -1.088641768524161391 ) ) ;
#12317 = EDGE_LOOP ( 'NONE', ( #21364, #14107, #2895, #4003 ) ) ;
#12318 = CARTESIAN_POINT ( 'NONE',  ( -7.454531657079158435, 2.846291840500173365, 1.545410377633946952 ) ) ;
#12319 = CARTESIAN_POINT ( 'NONE',  ( 0.000000000000000000, 7.347880794884120722E-16, 6.000000000000000888 ) ) ;
#12320 = AXIS2_PLACEMENT_3D ( 'NONE', #24163, #26375, #21814 ) ;
#12321 = CARTESIAN_POINT ( 'NONE',  ( 23.72239361537270241, -6.441344918482257320, -5.695980980372493008 ) ) ;
#12322 = CIRCLE ( 'NONE', #8577, 5.000000000000003553 ) ;
#12323 = CARTESIAN_POINT ( 'NONE',  ( 14.53002800497467462, -16.11929632631086307, 1.753673441884563200 ) ) ;
#12324 = FACE_OUTER_BOUND ( 'NONE', #32672, .T. ) ;
#12325 = ORIENTED_EDGE ( 'NONE', *, *, #4495, .T. ) ;
#12326 = EDGE_CURVE ( 'NONE', #29752, #15174, #14894, .T. ) ;
#12327 = CARTESIAN_POINT ( 'NONE',  ( 18.97846294920043420, -3.417963736896675986, 1.868788737152642598 ) ) ;
#12328 = EDGE_CURVE ( 'NONE', #17825, #9859, #15711, .T. ) ;
#12329 = AXIS2_PLACEMENT_3D ( 'NONE', #32744, #4492, #7647 ) ;
#12330 = B_SPLINE_CURVE_WITH_KNOTS ( 'NONE', 3,
 ( #18395, #23549, #493, #2527, #20736, #30788 ),
 .UNSPECIFIED., .F., .F.,
 ( 4, 2, 4 ),
 ( 0.0008064882591616613769, 0.001664279756741902493, 0.002522071254322143935 ),
 .UNSPECIFIED. ) ;
#12331 =( BOUNDED_CURVE ( )  B_SPLINE_CURVE ( 3, ( #16904, #4199, #6551, #29788 ),
 .UNSPECIFIED., .F., .F. ) 
 B_SPLINE_CURVE_WITH_KNOTS ( ( 4, 4 ),
 ( 5.051426171356965256, 5.615871152429257940 ),
 .UNSPECIFIED. ) 
 CURVE ( )  GEOMETRIC_REPRESENTATION_ITEM ( )  RATIONAL_B_SPLINE_CURVE ( ( 1.000000000000000000, 0.9736259116362534494, 0.9736259116362534494, 1.000000000000000000 ) ) 
 REPRESENTATION_ITEM ( '' )  );
#12332 = VERTEX_POINT ( 'NONE', #7058 ) ;
#12333 = DIRECTION ( 'NONE',  ( 1.000000000000000000, -0.000000000000000000, -0.000000000000000000 ) ) ;
#12334 = EDGE_CURVE ( 'NONE', #18943, #6749, #12059, .T. ) ;
#12335 = PERSON_AND_ORGANIZATION ( #6766, #25292 ) ;
#12336 = CARTESIAN_POINT ( 'NONE',  ( 28.66422432450819358, -6.760491130759657352, 4.001040682715384378 ) ) ;
#12337 = VECTOR ( 'NONE', #6674, 1000.000000000000114 ) ;
#12338 = CARTESIAN_POINT ( 'NONE',  ( 107.4500446874327935, -17.36019328965565123, 4.522129901861156931 ) ) ;
#12340 = CARTESIAN_POINT ( 'NONE',  ( 1.624999999999999778, -7.593217523260639368, 7.958834565716742304 ) ) ;
#12339 = CARTESIAN_POINT ( 'NONE',  ( 6.880159396099833735, 7.882559112973164694, 3.754731129947811219 ) ) ;
#12341 = ORIENTED_EDGE ( 'NONE', *, *, #23419, .T. ) ;
#12342 = CARTESIAN_POINT ( 'NONE',  ( 20.74999999999999645, 5.999999999999998224, 0.000000000000000000 ) ) ;
#12343 = DIRECTION ( 'NONE',  ( 0.000000000000000000, 0.000000000000000000, 1.000000000000000000 ) ) ;
#12344 = CARTESIAN_POINT ( 'NONE',  ( 23.36000000136559507, -1.570731468192933633, -2.892927487894330074 ) ) ;
#12345 = CARTESIAN_POINT ( 'NONE',  ( 3.164041846090267285, -11.65249415702359137, -1.500000000000000000 ) ) ;
#12347 = EDGE_LOOP ( 'NONE', ( #24853, #22074, #28765, #32620, #21312 ) ) ;
#12346 = CARTESIAN_POINT ( 'NONE',  ( 107.4685439760147432, 18.03024793969074935, 4.906145018174012939 ) ) ;
#12348 = CARTESIAN_POINT ( 'NONE',  ( -4.837550801365592790, 3.675193018007247403, -1.088641768524161391 ) ) ;
#12349 = DIRECTION ( 'NONE',  ( 6.938893903907228378E-15, 0.000000000000000000, -1.000000000000000000 ) ) ;
#12350 = VECTOR ( 'NONE', #13465, 1000.000000000000114 ) ;
#12351 = CARTESIAN_POINT ( 'NONE',  ( 41.43141396789280151, -2.886852813799071438, 0.07017451552782173751 ) ) ;
#12352 = DIRECTION ( 'NONE',  ( -3.623545766764274403E-17, -0.4226182617407064912, 0.9063077870366467170 ) ) ;
#12353 = EDGE_LOOP ( 'NONE', ( #12747, #4431, #32290 ) ) ;
#12355 = VERTEX_POINT ( 'NONE', #20116 ) ;
#12354 = CARTESIAN_POINT ( 'NONE',  ( -3.526383166312414108, 10.27186380921760289, 5.187041768249671669 ) ) ;
#12356 = VECTOR ( 'NONE', #15719, 1000.000000000000000 ) ;
#12357 = AXIS2_PLACEMENT_3D ( 'NONE', #11465, #6124, #1098 ) ;
#12359 = AXIS2_PLACEMENT_3D ( 'NONE', #31897, #24196, #1320 ) ;
#12358 = CARTESIAN_POINT ( 'NONE',  ( 0.000000000000000000, 4.057423117305393845, 8.475820894092990443 ) ) ;
#12360 = CARTESIAN_POINT ( 'NONE',  ( 25.75999999999999801, -2.208672634433321348E-15, 0.000000000000000000 ) ) ;
#12361 = CARTESIAN_POINT ( 'NONE',  ( 5.377543748152548986, 7.892520144992435149, 1.391664247347255134 ) ) ;
#12362 = AXIS2_PLACEMENT_3D ( 'NONE', #28147, #10257, #31179 ) ;
#12363 = CARTESIAN_POINT ( 'NONE',  ( -22.67670559979717382, 18.46223496596762459, 1.773004750130064533 ) ) ;
#12364 = CIRCLE ( 'NONE', #32697, 5.009999999999999787 ) ;
#12365 = CARTESIAN_POINT ( 'NONE',  ( 18.89400067069965772, -4.362082497104407430, 3.390608483629235614 ) ) ;
#12366 = CARTESIAN_POINT ( 'NONE',  ( 6.212874240570648965, -18.25778580431405018, -1.748739671137289342 ) ) ;
#12367 = CIRCLE ( 'NONE', #3323, 8.750000000000000000 ) ;
#12368 = ADVANCED_FACE ( 'NONE', ( #4215 ), #22431, .T. ) ;
#12369 = CARTESIAN_POINT ( 'NONE',  ( 25.04749999999999943, 2.594547506269380133, 0.7685399846772031918 ) ) ;
#12370 = CARTESIAN_POINT ( 'NONE',  ( 68.93397511290362445, -3.394585223421699549, 1.169951107274293856 ) ) ;
#12371 = CARTESIAN_POINT ( 'NONE',  ( 107.9151932992832315, -16.84816672447076513, 3.542199815866853729 ) ) ;
#12372 = ORIENTED_EDGE ( 'NONE', *, *, #2650, .F. ) ;
#12373 = DIRECTION ( 'NONE',  ( 0.000000000000000000, 0.000000000000000000, -1.000000000000000000 ) ) ;
#12374 = CIRCLE ( 'NONE', #6475, 8.749000000000002331 ) ;
#12375 = CARTESIAN_POINT ( 'NONE',  ( 2.357330058169019527, 7.401770933800327690, -7.915524238820659697 ) ) ;
#12376 = ORIENTED_EDGE ( 'NONE', *, *, #1514, .F. ) ;
#12377 = AXIS2_PLACEMENT_3D ( 'NONE', #2814, #20353, #18159 ) ;
#12378 = VECTOR ( 'NONE', #20928, 1000.000000000000000 ) ;
#12379 = CARTESIAN_POINT ( 'NONE',  ( 107.5346493233867875, 18.40935155254226174, -5.110104196312056146 ) ) ;
#12380 = AXIS2_PLACEMENT_3D ( 'NONE', #6876, #9899, #32483 ) ;
#12381 = ORIENTED_EDGE ( 'NONE', *, *, #11358, .T. ) ;
#12382 = CARTESIAN_POINT ( 'NONE',  ( 3.499999999999999556, -8.497168642645963388, -0.2193742428685781509 ) ) ;
#12384 = ORIENTED_EDGE ( 'NONE', *, *, #14349, .T. ) ;
#12383 = CARTESIAN_POINT ( 'NONE',  ( 54.94602868030273868, -5.379417012101376017, -4.023790190284213253 ) ) ;
#12385 = EDGE_LOOP ( 'NONE', ( #8314, #8170, #2982, #28382 ) ) ;
#12386 = VECTOR ( 'NONE', #5208, 1000.000000000000000 ) ;
#12387 = CARTESIAN_POINT ( 'NONE',  ( 23.42250000000000298, -2.378061970571983430, 1.291182301015471490 ) ) ;
#12388 = AXIS2_PLACEMENT_3D ( 'NONE', #28177, #30725, #8289 ) ;
#12389 = LINE ( 'NONE', #9219, #28931 ) ;
#12391 = ORIENTED_EDGE ( 'NONE', *, *, #21793, .T. ) ;
#12390 = CARTESIAN_POINT ( 'NONE',  ( 0.1606233164486141063, 5.257199111574340833, 9.238724727304049367 ) ) ;
#12392 = CARTESIAN_POINT ( 'NONE',  ( 22.89387586468013325, 17.41384229115070426, -1.050000000000117950 ) ) ;
#12393 = CARTESIAN_POINT ( 'NONE',  ( 25.54995566824271336, 19.30806704599434553, 1.500000000000000000 ) ) ;
#12394 = DIRECTION ( 'NONE',  ( 0.000000000000000000, 0.000000000000000000, 1.000000000000000000 ) ) ;
#12395 = CARTESIAN_POINT ( 'NONE',  ( 3.499999999999999556, 0.000000000000000000, 0.000000000000000000 ) ) ;
#12396 = EDGE_CURVE ( 'NONE', #22604, #17057, #2362, .T. ) ;
#12397 = EDGE_LOOP ( 'NONE', ( #26357, #25927, #17885, #32233 ) ) ;
#12398 = CARTESIAN_POINT ( 'NONE',  ( 25.75999999999999801, -2.208672634433321348E-15, 0.000000000000000000 ) ) ;
#12399 = VECTOR ( 'NONE', #32974, 1000.000000000000227 ) ;
#12400 = EDGE_CURVE ( 'NONE', #18469, #23780, #15395, .T. ) ;
#12401 = CIRCLE ( 'NONE', #18807, 2.750000000000000444 ) ;
#12402 = DIRECTION ( 'NONE',  ( -0.1503837331804358524, 0.08682408883346492967, -0.9848077530122080203 ) ) ;
#12403 = CARTESIAN_POINT ( 'NONE',  ( 25.67250000136559507, 2.363507492473148286, 1.913930629741525058 ) ) ;
#12404 = AXIS2_PLACEMENT_3D ( 'NONE', #1984, #22039, #4148 ) ;
#12405 = CIRCLE ( 'NONE', #30038, 7.981930256614262476 ) ;
#12406 = CARTESIAN_POINT ( 'NONE',  ( 107.6696441609669819, 19.18460445470642739, -4.889496736489043371 ) ) ;
#12407 = CIRCLE ( 'NONE', #15642, 5.010000000000000675 ) ;
#12408 = DIRECTION ( 'NONE',  ( 1.224646799147353207E-16, 1.000000000000000000, 0.000000000000000000 ) ) ;
#12409 = CARTESIAN_POINT ( 'NONE',  ( 20.99695690729575048, -21.77932090203125526, -1.367431712678143008 ) ) ;
#12410 = VERTEX_POINT ( 'NONE', #18245 ) ;
#12411 = CARTESIAN_POINT ( 'NONE',  ( 109.6329156864505165, 19.01855260168436246, 4.629213727441584325 ) ) ;
#12412 = EDGE_CURVE ( 'NONE', #3558, #14852, #23418, .T. ) ;
#12413 = CIRCLE ( 'NONE', #16681, 10.94895958125474245 ) ;
#12414 = LINE ( 'NONE', #12900, #27873 ) ;
#12415 = EDGE_CURVE ( 'NONE', #10741, #19641, #10364, .T. ) ;
#12416 = CARTESIAN_POINT ( 'NONE',  ( -7.387550801365593500, 0.3701630799359330593, -3.521866450007987037 ) ) ;
#12417 = ORIENTED_EDGE ( 'NONE', *, *, #1034, .T. ) ;
#12418 = AXIS2_PLACEMENT_3D ( 'NONE', #20062, #15344, #15193 ) ;
#12419 = FACE_OUTER_BOUND ( 'NONE', #24385, .T. ) ;
#12420 = CYLINDRICAL_SURFACE ( 'NONE', #15159, 8.500000000000000000 ) ;
#12421 = CARTESIAN_POINT ( 'NONE',  ( 3.329122376115283277, 0.6654791810437885591, -0.9318852528018959358 ) ) ;
#12422 = ORIENTED_EDGE ( 'NONE', *, *, #27217, .F. ) ;
#12423 = CARTESIAN_POINT ( 'NONE',  ( 9.057441432442507434, -0.5488979288031592407, 0.9999999999999997780 ) ) ;
#12424 = EDGE_CURVE ( 'NONE', #17962, #9305, #230, .T. ) ;
#12425 = EDGE_LOOP ( 'NONE', ( #3634, #30532, #15776, #19736 ) ) ;
#12426 = CONICAL_SURFACE ( 'NONE', #14009, 3.024999999999999911, 0.7853981633974520538 ) ;
#12427 = CIRCLE ( 'NONE', #14575, 3.250000000000002665 ) ;
#12428 = CARTESIAN_POINT ( 'NONE',  ( 0.3045634402744727964, -4.096074720329294649, -9.425384029459461743 ) ) ;
#12429 = EDGE_LOOP ( 'NONE', ( #30757, #524, #33002, #17447 ) ) ;
#12430 = DIRECTION ( 'NONE',  ( 1.000000000000000000, -0.000000000000000000, 0.000000000000000000 ) ) ;
#12431 = PRODUCT ( 'Part3_SlicingGear', 'Part3_SlicingGear', '', ( #19706 ) ) ;
#12432 = AXIS2_PLACEMENT_3D ( 'NONE', #7516, #25420, #23389 ) ;
#12434 = ORIENTED_EDGE ( 'NONE', *, *, #6276, .T. ) ;
#12433 = CYLINDRICAL_SURFACE ( 'NONE', #2154, 5.010000000000000675 ) ;
#12435 = ORIENTED_EDGE ( 'NONE', *, *, #10634, .F. ) ;
#12436 = DIRECTION ( 'NONE',  ( 0.1441052676711226943, 0.9895623637898898206, 0.000000000000000000 ) ) ;
#12437 = CIRCLE ( 'NONE', #11364, 8.749000000000002331 ) ;
#12438 = AXIS2_PLACEMENT_3D ( 'NONE', #18543, #8192, #16007 ) ;
#12440 = ADVANCED_FACE ( 'NONE', ( #18080 ), #10221, .T. ) ;
#12439 = AXIS2_PLACEMENT_3D ( 'NONE', #31800, #11700, #19078 ) ;
#12441 = VERTEX_POINT ( 'NONE', #26104 ) ;
#12442 = DIRECTION ( 'NONE',  ( -0.000000000000000000, 0.000000000000000000, 1.000000000000000000 ) ) ;
#12444 = VERTEX_POINT ( 'NONE', #28271 ) ;
#12443 = CARTESIAN_POINT ( 'NONE',  ( 3.529609406779910419, -12.17998485103522199, 1.500000000000000000 ) ) ;
#12445 = DIRECTION ( 'NONE',  ( -1.224646799147353207E-16, 1.000000000000000000, 0.000000000000000000 ) ) ;
#12446 = CARTESIAN_POINT ( 'NONE',  ( 0.000000000000000000, 0.000000000000000000, 0.000000000000000000 ) ) ;
#12447 = CARTESIAN_POINT ( 'NONE',  ( -50.60000000000000142, -10.96966150227468972, 7.074999999999997513 ) ) ;
#12448 = CARTESIAN_POINT ( 'NONE',  ( -50.60000000000000142, -0.5000000000000000000, 1.500000000000000000 ) ) ;
#12449 = CARTESIAN_POINT ( 'NONE',  ( -3.362942409646513031, -5.022711880624455567E-15, 2.999999999999999556 ) ) ;
#12450 = CARTESIAN_POINT ( 'NONE',  ( 24.83519197235663256, -17.49564329958969111, 1.498842795365988412 ) ) ;
#12451 = CARTESIAN_POINT ( 'NONE',  ( 7.249760686538667009, 0.000000000000000000, 0.000000000000000000 ) ) ;
#12452 = FACE_OUTER_BOUND ( 'NONE', #23239, .T. ) ;
#12453 = CIRCLE ( 'NONE', #10336, 3.250000000000002665 ) ;
#12454 = CARTESIAN_POINT ( 'NONE',  ( 0.000000000000000000, 0.5174497483512452423, 0.000000000000000000 ) ) ;
#12455 = DIRECTION ( 'NONE',  ( 0.000000000000000000, 0.000000000000000000, -1.000000000000000000 ) ) ;
#12456 = AXIS2_PLACEMENT_3D ( 'NONE', #6625, #32035, #3969 ) ;
#12457 = ADVANCED_FACE ( 'NONE', ( #20443 ), #525, .T. ) ;
#12458 = DIRECTION ( 'NONE',  ( 0.000000000000000000, 0.2588190451025185190, -0.9659258262890689783 ) ) ;
#12459 = ADVANCED_FACE ( 'NONE', ( #3063 ), #31145, .T. ) ;
#12460 = CARTESIAN_POINT ( 'NONE',  ( -3.250050802731187183, -2.331437884370912705, 1.887961173149512062 ) ) ;
#12461 = VERTEX_POINT ( 'NONE', #25603 ) ;
#12462 = VECTOR ( 'NONE', #26567, 1000.000000000000114 ) ;
#12463 = AXIS2_PLACEMENT_3D ( 'NONE', #31789, #29258, #16534 ) ;
#12464 = CARTESIAN_POINT ( 'NONE',  ( -4.450050800000000528, 1.549418761218566143, -2.853674364686379583 ) ) ;
#12465 = CARTESIAN_POINT ( 'NONE',  ( 0.3749742847179773353, 3.955024136977333793, 9.289351359934620689 ) ) ;
#12466 = CARTESIAN_POINT ( 'NONE',  ( 0.000000000000000000, 9.241976615262160522, -1.699438267350404930 ) ) ;
#12467 = PRODUCT_DEFINITION_FORMATION_WITH_SPECIFIED_SOURCE ( 'ANY', '', #17492, .NOT_KNOWN. ) ;
#12468 = ORIENTED_EDGE ( 'NONE', *, *, #1345, .F. ) ;
#12469 = DIRECTION ( 'NONE',  ( 0.000000000000000000, 0.000000000000000000, 1.000000000000000000 ) ) ;
#12470 = DIRECTION ( 'NONE',  ( 1.000000000000000000, 0.000000000000000000, 0.000000000000000000 ) ) ;
#12471 = EDGE_CURVE ( 'NONE', #27615, #4248, #15751, .T. ) ;
#12472 = CARTESIAN_POINT ( 'NONE',  ( 108.0243507582653280, -18.42000697793362107, 4.471835319414810606 ) ) ;
#12473 = ORIENTED_EDGE ( 'NONE', *, *, #15001, .F. ) ;
#12474 = CARTESIAN_POINT ( 'NONE',  ( 101.7699185271994224, -3.585367684922579290, -4.312036717292317967 ) ) ;
#12475 = COORDINATED_UNIVERSAL_TIME_OFFSET ( 0, 0, .AHEAD. ) ;
#12476 = CARTESIAN_POINT ( 'NONE',  ( -2.962992063741595405, -11.77309494928644185, -1.499999999999999556 ) ) ;
#12477 = ORIENTED_EDGE ( 'NONE', *, *, #27272, .F. ) ;
#12478 = CARTESIAN_POINT ( 'NONE',  ( -2.596515638727389330, -12.68063260205361154, 1.500000000000000666 ) ) ;
#12479 = EDGE_CURVE ( 'NONE', #24378, #7137, #18430, .T. ) ;
#12480 = VERTEX_POINT ( 'NONE', #10403 ) ;
#12481 = FACE_OUTER_BOUND ( 'NONE', #1561, .T. ) ;
#12482 = VECTOR ( 'NONE', #28621, 1000.000000000000000 ) ;
#12483 = CARTESIAN_POINT ( 'NONE',  ( -54.00754732910517930, 5.431685566383787744, 1.345424820068321425 ) ) ;
#12484 = VECTOR ( 'NONE', #24500, 1000.000000000000000 ) ;
#12485 = DIRECTION ( 'NONE',  ( 1.000000000000000000, -8.574039729943018344E-17, -0.000000000000000000 ) ) ;
#12486 = CARTESIAN_POINT ( 'NONE',  ( -5.712942406915326288, 3.284080845023683730E-15, 3.000000000000000000 ) ) ;
#12487 =( REPRESENTATION_RELATIONSHIP ('NONE','NONE', #1085, #5606 ) REPRESENTATION_RELATIONSHIP_WITH_TRANSFORMATION ( #17477 )SHAPE_REPRESENTATION_RELATIONSHIP( ) );
#12488 = VECTOR ( 'NONE', #31205, 1000.000000000000000 ) ;
#12489 = CARTESIAN_POINT ( 'NONE',  ( 21.41614545859222929, -21.75488722177052026, -1.449289482123008899 ) ) ;
#12490 = DIRECTION ( 'NONE',  ( 0.000000000000000000, 0.000000000000000000, 1.000000000000000000 ) ) ;
#12491 = ORIENTED_EDGE ( 'NONE', *, *, #24185, .T. ) ;
#12492 = DIRECTION ( 'NONE',  ( 0.5075624751249186994, 0.8616149568369075862, -1.660737436530807968E-15 ) ) ;
#12493 = DIRECTION ( 'NONE',  ( 0.08343273266574550984, 0.4645863764670127849, -0.8815886103626664472 ) ) ;
#12494 = CARTESIAN_POINT ( 'NONE',  ( 0.6728000631949255794, 0.5626559339000506421, -9.133409206458198426 ) ) ;
#12495 = CARTESIAN_POINT ( 'NONE',  ( 102.5829460782277351, -0.8583298743145996168, -2.713652344655541615 ) ) ;
#12496 = B_SPLINE_CURVE_WITH_KNOTS ( 'NONE', 3,
 ( #19296, #16791, #29496, #26348, #8915, #11270, #928, #31694, #6594, #16289 ),
 .UNSPECIFIED., .F., .F.,
 ( 4, 2, 2, 2, 4 ),
 ( 1.968338519012340724E-07, 0.0005467927057105484217, 0.001093388577569195637, 0.001639984449427842744, 0.002186580321286490068 ),
 .UNSPECIFIED. ) ;
#12497 = CC_DESIGN_APPROVAL ( #6347, ( #27439 ) ) ;
#12498 = EDGE_CURVE ( 'NONE', #10411, #18566, #5380, .T. ) ;
#12499 = CARTESIAN_POINT ( 'NONE',  ( -50.81000000000000227, -10.96999999999998643, 8.549999999999998934 ) ) ;
#12500 = CARTESIAN_POINT ( 'NONE',  ( -56.32770133515839461, 0.5000000000000000000, -1.500000000000000000 ) ) ;
#12501 = CARTESIAN_POINT ( 'NONE',  ( 24.29750000273118715, 2.594547506269380133, 0.7685399846772031918 ) ) ;
#12503 = CARTESIAN_POINT ( 'NONE',  ( 23.22050010673017084, -21.93619796768861008, 1.062839084287792391 ) ) ;
#12502 = DESIGN_CONTEXT ( 'detailed design', #15441, 'design' ) ;
#12504 = ORIENTED_EDGE ( 'NONE', *, *, #31328, .F. ) ;
#12505 = CARTESIAN_POINT ( 'NONE',  ( -6.362550801365593145, 2.752080473201636845, -2.228590825266444142 ) ) ;
#12506 = ORIENTED_EDGE ( 'NONE', *, *, #21300, .T. ) ;
#12507 = CARTESIAN_POINT ( 'NONE',  ( -5.954531657079157547, 3.105402419394639235, -0.9198621039125850496 ) ) ;
#12508 = CIRCLE ( 'NONE', #16247, 5.000000000000000000 ) ;
#12509 = CARTESIAN_POINT ( 'NONE',  ( 5.377543748152548098, 6.940565734314597002, 4.007137495034836405 ) ) ;
#12510 = DIRECTION ( 'NONE',  ( 0.000000000000000000, 0.000000000000000000, 1.000000000000000000 ) ) ;
#12511 = CYLINDRICAL_SURFACE ( 'NONE', #16727, 11.00000000000000000 ) ;
#12512 = FACE_OUTER_BOUND ( 'NONE', #11573, .T. ) ;
#12513 = ORIENTED_EDGE ( 'NONE', *, *, #29243, .T. ) ;
#12514 = CARTESIAN_POINT ( 'NONE',  ( 21.36526493837866170, -21.76156136282174813, 1.423309099665599264 ) ) ;
#12515 = ORIENTED_EDGE ( 'NONE', *, *, #2113, .T. ) ;
#12516 = CARTESIAN_POINT ( 'NONE',  ( -3.650050800000000262, 1.549418761218566143, -2.853674364686379583 ) ) ;
#12517 = PERSON_AND_ORGANIZATION_ROLE ( 'creator' ) ;
#12519 = CARTESIAN_POINT ( 'NONE',  ( 40.88395664866006740, -6.890158765445390188, 4.003574183511678264 ) ) ;
#12518 = CC_DESIGN_APPROVAL ( #7567, ( #26402 ) ) ;
#12520 = CARTESIAN_POINT ( 'NONE',  ( 107.4500520110599240, -17.36019279015700079, 4.522129904808851464 ) ) ;
#12522 = DIRECTION ( 'NONE',  ( 0.000000000000000000, 0.000000000000000000, 1.000000000000000000 ) ) ;
#12521 = CARTESIAN_POINT ( 'NONE',  ( 0.5032040568826979809, 8.283195248915220077, -5.109302080990099526 ) ) ;
#12523 = ORIENTED_EDGE ( 'NONE', *, *, #28579, .T. ) ;
#12524 = CARTESIAN_POINT ( 'NONE',  ( 10.00000000000000000, 0.8254815157535864145, -4.681538312723508177 ) ) ;
#12525 = DIRECTION ( 'NONE',  ( 0.000000000000000000, 0.000000000000000000, 1.000000000000000000 ) ) ;
#12526 = CARTESIAN_POINT ( 'NONE',  ( 24.67250000136559507, 3.024605502323846729, -0.3178988483021056854 ) ) ;
#12527 = CARTESIAN_POINT ( 'NONE',  ( 21.04767255914890356, -17.06392231637721579, -1.499999999999999778 ) ) ;
#12529 = ORIENTED_EDGE ( 'NONE', *, *, #886, .T. ) ;
#12528 = CARTESIAN_POINT ( 'NONE',  ( 1.386174007446661749, -9.662292653395716968, 0.9788672205888330202 ) ) ;
#12530 = CARTESIAN_POINT ( 'NONE',  ( -5.312550801365592434, 1.088641768524161613, 3.675193018007247403 ) ) ;
#12531 = CARTESIAN_POINT ( 'NONE',  ( -40.73102457812986898, -13.75294349655999326, 5.448103877476410339 ) ) ;
#12532 = CARTESIAN_POINT ( 'NONE',  ( -31.80959807272228090, -0.0003384977252891612984, 0.000000000000000000 ) ) ;
#12533 = CARTESIAN_POINT ( 'NONE',  ( 85.03618457008526832, -5.204454441919745378, -3.993433531025833982 ) ) ;
#12534 = VERTEX_POINT ( 'NONE', #5716 ) ;
#12536 = VERTEX_POINT ( 'NONE', #13076 ) ;
#12535 = DIRECTION ( 'NONE',  ( -1.000000000000000000, 0.000000000000000000, 0.000000000000000000 ) ) ;
#12537 = EDGE_CURVE ( 'NONE', #21273, #1079, #27977, .T. ) ;
#12538 = CARTESIAN_POINT ( 'NONE',  ( 2.274274201627372705, 7.593217523255878731, 7.958834565715730669 ) ) ;
#12539 = CARTESIAN_POINT ( 'NONE',  ( 2.857987896746965184, -9.278099925236423573, -2.305585824582613519 ) ) ;
#12540 = B_SPLINE_CURVE_WITH_KNOTS ( 'NONE', 3,
 ( #17884, #32939, #15352, #12182, #17528, #20070, #25557, #30266, #7189, #15011 ),
 .UNSPECIFIED., .F., .F.,
 ( 4, 2, 2, 2, 4 ),
 ( 1.968338519002063038E-07, 0.0005467928198071719554, 0.001093388805762443572, 0.001639984791717715188, 0.002186580777672987239 ),
 .UNSPECIFIED. ) ;
#12541 = EDGE_CURVE ( 'NONE', #11793, #26254, #22778, .T. ) ;
#12542 = CARTESIAN_POINT ( 'NONE',  ( 21.42250000136559507, -0.3178988483021076838, -3.024605502323848949 ) ) ;
#12543 = CARTESIAN_POINT ( 'NONE',  ( 18.86054332783663767, -4.736068442360261699, 3.993434336035624366 ) ) ;
#12544 = CARTESIAN_POINT ( 'NONE',  ( 0.2700844563487312389, -15.55376400399037351, -1.499999999999999556 ) ) ;
#12545 = CARTESIAN_POINT ( 'NONE',  ( -34.31843563627105453, 19.51744974835125035, -2.301584610165037237 ) ) ;
#12546 =( BOUNDED_CURVE ( )  B_SPLINE_CURVE ( 2, ( #13797, #14151, #6294, #19167, #1614, #3982, #14461, #22186, #26863, #11807, #22015 ),
 .UNSPECIFIED., .F., .F. ) 
 B_SPLINE_CURVE_WITH_KNOTS ( ( 3, 2, 2, 2, 2, 3 ),
 ( 0.3728822619934377136, 0.3750000000000000000, 0.3906250000000000000, 0.4062500000000000000, 0.4218750000000000000, 0.4353822619934377136 ),
 .UNSPECIFIED. ) 
 CURVE ( )  GEOMETRIC_REPRESENTATION_ITEM ( )  RATIONAL_B_SPLINE_CURVE ( ( 0.9821626249036857770, 0.9896829947469991673, 1.000000000000000000, 0.9238795325112867385, 1.000000000000000000, 0.9238795325112867385, 1.000000000000000000, 0.9238795325112867385, 1.000000000000000000, 0.9341965377642874602, 0.9821626249036857770 ) ) 
 REPRESENTATION_ITEM ( '' )  );
#12547 = CARTESIAN_POINT ( 'NONE',  ( 7.249760686538667009, 7.892520144992435149, 1.391664247347255134 ) ) ;
#12548 = CARTESIAN_POINT ( 'NONE',  ( 41.44567272411835290, -7.615257740949710197, 4.522129901861162260 ) ) ;
#12549 = ORIENTED_EDGE ( 'NONE', *, *, #13272, .T. ) ;
#12550 = CARTESIAN_POINT ( 'NONE',  ( 3.063284526839887167, 8.461683424509313767, 2.223716399045601921 ) ) ;
#12551 = SECURITY_CLASSIFICATION_LEVEL ( 'unclassified' ) ;
#12552 = FACE_OUTER_BOUND ( 'NONE', #19978, .T. ) ;
#12553 = ORIENTED_EDGE ( 'NONE', *, *, #5165, .F. ) ;
#12554 = CARTESIAN_POINT ( 'NONE',  ( 107.4385791398479029, 17.85938043952739562, -4.612695725900423760 ) ) ;
#12555 = VERTEX_POINT ( 'NONE', #10552 ) ;
#12556 = CARTESIAN_POINT ( 'NONE',  ( -20.10769817351002331, 5.029112325015176133, 2.117653528444686906 ) ) ;
#12558 = ORIENTED_EDGE ( 'NONE', *, *, #8565, .F. ) ;
#12557 = CARTESIAN_POINT ( 'NONE',  ( 54.94593103970883163, -5.375889154831037686, -4.018750264957798635 ) ) ;
#12559 = ORIENTED_EDGE ( 'NONE', *, *, #23112, .T. ) ;
#12560 = CARTESIAN_POINT ( 'NONE',  ( 74.30107678963170770, -22.79527490385382649, -1.500000000000000000 ) ) ;
#12561 = CARTESIAN_POINT ( 'NONE',  ( -7.112550801365592257, 3.675193018007246959, -1.088641768524161391 ) ) ;
#12562 = LINE ( 'NONE', #7726, #7084 ) ;
#12563 = CARTESIAN_POINT ( 'NONE',  ( 69.41104820195521086, -8.577144703210709764, -1.915219082070897638 ) ) ;
#12565 = ORIENTED_EDGE ( 'NONE', *, *, #25836, .F. ) ;
#12564 = CARTESIAN_POINT ( 'NONE',  ( 0.000000000000000000, 8.357095590591338663, -1.552080310331533486 ) ) ;
#12566 = CARTESIAN_POINT ( 'NONE',  ( 26.23135861748343345, 19.12135596485594746, -1.500000000000000000 ) ) ;
#12567 = CARTESIAN_POINT ( 'NONE',  ( 0.000000000000000000, 0.000000000000000000, 0.000000000000000000 ) ) ;
#12568 = CARTESIAN_POINT ( 'NONE',  ( -4.174653281524877357, -9.415293141582383285, 1.500000000000000000 ) ) ;
#12569 = EDGE_CURVE ( 'NONE', #3086, #18770, #20763, .T. ) ;
#12570 = DIRECTION ( 'NONE',  ( -0.03662738895564521951, 0.5274252892134372317, -0.8488115212910425367 ) ) ;
#12571 = EDGE_CURVE ( 'NONE', #9130, #18033, #26392, .T. ) ;
#12573 = ORIENTED_EDGE ( 'NONE', *, *, #20135, .T. ) ;
#12572 = CARTESIAN_POINT ( 'NONE',  ( 108.0286247234065655, -18.48155101273792411, -4.347446253313675513 ) ) ;
#12574 = DIRECTION ( 'NONE',  ( 0.07591486983605109928, 0.4227239498242779114, -0.9030733053206351224 ) ) ;
#12575 = EDGE_CURVE ( 'NONE', #9383, #13763, #30964, .T. ) ;
#12576 = CARTESIAN_POINT ( 'NONE',  ( 7.249760686538667009, -0.7071067811865734409, 8.721381771256202953 ) ) ;
#12577 = CARTESIAN_POINT ( 'NONE',  ( 34.48223484310469900, 0.5000000000000000000, 2.482234843104950350 ) ) ;
#12578 = DIRECTION ( 'NONE',  ( 1.000000000000000000, -0.000000000000000000, 8.654346879536960414E-15 ) ) ;
#12579 = CARTESIAN_POINT ( 'NONE',  ( 5.885541806331895387, 7.076443837534019288, -4.514241479885472863 ) ) ;
#12580 = DIRECTION ( 'NONE',  ( 0.1027947991993887200, -0.9947025833170221043, 1.084202172485531452E-15 ) ) ;
#12581 = VERTEX_POINT ( 'NONE', #7549 ) ;
#12582 = FACE_OUTER_BOUND ( 'NONE', #25654, .T. ) ;
#12583 = FACE_OUTER_BOUND ( 'NONE', #28561, .T. ) ;
#12584 = CARTESIAN_POINT ( 'NONE',  ( -5.937550801365592434, -3.368539882008727115, -1.828967928396027842 ) ) ;
#12585 = EDGE_LOOP ( 'NONE', ( #28407, #15550, #16401 ) ) ;
#12586 = CARTESIAN_POINT ( 'NONE',  ( -5.362942409646513475, -3.366872799099910998E-15, -3.000000000000000000 ) ) ;
#12587 = CARTESIAN_POINT ( 'NONE',  ( 5.612974384376776982, 7.213266193303311979, -3.934067627273127865 ) ) ;
#12588 = CARTESIAN_POINT ( 'NONE',  ( 16.80274661516410006, -16.53680364986711737, -1.500000000000000444 ) ) ;
#12589 = EDGE_LOOP ( 'NONE', ( #5087, #24653, #3820, #7411 ) ) ;
#12590 = CARTESIAN_POINT ( 'NONE',  ( 8.770003503075953333, -11.01188172931930254, 1.000000000000000666 ) ) ;
#12591 = EDGE_LOOP ( 'NONE', ( #64, #26048, #29631, #27577, #17408 ) ) ;
#12592 = CARTESIAN_POINT ( 'NONE',  ( 0.3749742847181603556, -3.955024136976903470, -9.289351359934268970 ) ) ;
#12593 = ORIENTED_EDGE ( 'NONE', *, *, #15919, .F. ) ;
#12594 = CARTESIAN_POINT ( 'NONE',  ( -2.910169157841151488, 0.01692106641068897091, 0.9265120394742449861 ) ) ;
#12596 = VERTEX_POINT ( 'NONE', #5569 ) ;
#12595 = CARTESIAN_POINT ( 'NONE',  ( 3.499999999999999556, 8.265874651078044977, -1.981241088980699061 ) ) ;
#12597 = ORIENTED_EDGE ( 'NONE', *, *, #26446, .T. ) ;
#12598 = CARTESIAN_POINT ( 'NONE',  ( 6.356382399260309235, -4.790388219480510301, -7.150437133400980194 ) ) ;
#12599 = ORIENTED_EDGE ( 'NONE', *, *, #30993, .T. ) ;
#12600 = CARTESIAN_POINT ( 'NONE',  ( -7.000050800000001239, 0.000000000000000000, 3.499999999999999556 ) ) ;
#12601 = EDGE_CURVE ( 'NONE', #16746, #8190, #16209, .T. ) ;
#12603 = ORIENTED_EDGE ( 'NONE', *, *, #8514, .T. ) ;
#12602 = CARTESIAN_POINT ( 'NONE',  ( 0.5309851148689820333, -4.399114163800174282, -1.500000000000000000 ) ) ;
#12604 = DIRECTION ( 'NONE',  ( -0.1356223135424326209, 0.9907606108790346644, 0.000000000000000000 ) ) ;
#12605 = DIRECTION ( 'NONE',  ( 0.000000000000000000, -0.9961946980917446570, -0.08715574274766962892 ) ) ;
#12606 = ADVANCED_FACE ( 'NONE', ( #32411 ), #3815, .T. ) ;
#12607 = CARTESIAN_POINT ( 'NONE',  ( 7.249760686538667009, -5.151476664237435443, -6.139290821770307716 ) ) ;
#12608 =( BOUNDED_CURVE ( )  B_SPLINE_CURVE ( 2, ( #14450, #11312, #1606, #6286, #11795, #16470, #26677, #3789, #13958, #24179, #28025 ),
 .UNSPECIFIED., .F., .F. ) 
 B_SPLINE_CURVE_WITH_KNOTS ( ( 3, 2, 2, 2, 2, 3 ),
 ( 0.1853822619934377414, 0.1875000000000000000, 0.2031250000000000000, 0.2187500000000000000, 0.2343750000000000000, 0.2478822619934377414 ),
 .UNSPECIFIED. ) 
 CURVE ( )  GEOMETRIC_REPRESENTATION_ITEM ( )  RATIONAL_B_SPLINE_CURVE ( ( 0.9821626249036861100, 0.9896829947469993893, 1.000000000000000000, 0.9238795325112867385, 1.000000000000000000, 0.9238795325112867385, 1.000000000000000000, 0.9238795325112867385, 1.000000000000000000, 0.9341965377642873491, 0.9821626249036861100 ) ) 
 REPRESENTATION_ITEM ( '' )  );
#12609 = CARTESIAN_POINT ( 'NONE',  ( 107.9029849834811614, 20.48784698331989773, 2.211997423210143143 ) ) ;
#12610 = EDGE_CURVE ( 'NONE', #16442, #6099, #16493, .T. ) ;
#12611 = FACE_BOUND ( 'NONE', #29202, .T. ) ;
#12612 = CARTESIAN_POINT ( 'NONE',  ( 24.79284380061039883, -17.49144841392520888, 1.371632250994630153 ) ) ;
#12613 = CARTESIAN_POINT ( 'NONE',  ( -4.575445569744995389, -7.851872718544268714, 0.9788672205877712029 ) ) ;
#12614 = CARTESIAN_POINT ( 'NONE',  ( 23.58234648083524121, -8.048792613698569909, 0.02339150517593243869 ) ) ;
#12615 = CARTESIAN_POINT ( 'NONE',  ( 3.499999999999999556, 0.000000000000000000, 0.000000000000000000 ) ) ;
#12616 = CARTESIAN_POINT ( 'NONE',  ( 101.6022419886208610, -1.170867242066748304, -0.02339150518254430253 ) ) ;
#12617 = EDGE_CURVE ( 'NONE', #29383, #27172, #27042, .T. ) ;
#12618 = FACE_OUTER_BOUND ( 'NONE', #29677, .T. ) ;
#12619 = CARTESIAN_POINT ( 'NONE',  ( -3.650050802731187094, 2.331437884370912705, -1.887961173149511618 ) ) ;
#12620 = EDGE_LOOP ( 'NONE', ( #8890, #5306, #28253, #27131, #4473 ) ) ;
#12621 = CARTESIAN_POINT ( 'NONE',  ( -6.787550801365593856, -3.521866450007987037, -0.3701630799359323931 ) ) ;
#12622 = CARTESIAN_POINT ( 'NONE',  ( 3.063284526839887167, 0.000000000000000000, 0.000000000000000000 ) ) ;
#12623 = ORIENTED_EDGE ( 'NONE', *, *, #90, .F. ) ;
#12624 = CARTESIAN_POINT ( 'NONE',  ( 7.064632951172269415, -5.064320921489772864, -7.135485519862048598 ) ) ;
#12625 = CARTESIAN_POINT ( 'NONE',  ( 6.356382477965130562, -5.959271875177110545, -6.209963745178070482 ) ) ;
#12626 = VERTEX_POINT ( 'NONE', #23584 ) ;
#12627 = CARTESIAN_POINT ( 'NONE',  ( 34.31843563627105453, 19.51744974835125035, -1.977928362984231025 ) ) ;
#12628 = EDGE_CURVE ( 'NONE', #26246, #9383, #22202, .T. ) ;
#12629 = DATE_AND_TIME ( #30367, #801 ) ;
#12631 = ORIENTED_EDGE ( 'NONE', *, *, #19067, .T. ) ;
#12630 = DIRECTION ( 'NONE',  ( -1.000000000000000000, -0.000000000000000000, 0.000000000000000000 ) ) ;
#12632 = ORIENTED_EDGE ( 'NONE', *, *, #23778, .F. ) ;
#12633 = CARTESIAN_POINT ( 'NONE',  ( 2.453127662067800863, -16.55897530748908153, 1.747541902167318861 ) ) ;
#12634 = ORIENTED_EDGE ( 'NONE', *, *, #353, .T. ) ;
#12635 = CARTESIAN_POINT ( 'NONE',  ( -41.77414131929176477, -16.18685544166627821, 1.949999999999999956 ) ) ;
#12637 = ORIENTED_EDGE ( 'NONE', *, *, #8798, .F. ) ;
#12636 = DIRECTION ( 'NONE',  ( 0.000000000000000000, 0.000000000000000000, 1.000000000000000000 ) ) ;
#12638 = LINE ( 'NONE', #14806, #21930 ) ;
#12639 = CARTESIAN_POINT ( 'NONE',  ( 4.546085788309846232E-16, -9.884132761439026638, -4.709950686174718903 ) ) ;
#12640 = EDGE_CURVE ( 'NONE', #21250, #31676, #30677, .T. ) ;
#12641 = CARTESIAN_POINT ( 'NONE',  ( -31.09064165252238965, -25.43932300454937945, 1.500000000000000000 ) ) ;
#12642 = EDGE_CURVE ( 'NONE', #27103, #15924, #28535, .T. ) ;
#12643 = CARTESIAN_POINT ( 'NONE',  ( -29.35000000000000853, -10.96966150227469505, -11.00000000000000000 ) ) ;
#12644 = ORIENTED_EDGE ( 'NONE', *, *, #14113, .F. ) ;
#12645 = CARTESIAN_POINT ( 'NONE',  ( 6.037141879243262288, -6.194548269014922504, 5.783072176360625427 ) ) ;
#12646 = CARTESIAN_POINT ( 'NONE',  ( 85.38119660046028514, -6.034158634444421132, 4.522129901861162260 ) ) ;
#12647 = CARTESIAN_POINT ( 'NONE',  ( 110.2274383572228942, 17.36892446252421962, -4.612695725900422872 ) ) ;
#12648 = CARTESIAN_POINT ( 'NONE',  ( 47.99837860531643940, -3.577301031424836353, -2.713652344655540727 ) ) ;
#12649 = EDGE_CURVE ( 'NONE', #32461, #10785, #32791, .T. ) ;
#12650 = CARTESIAN_POINT ( 'NONE',  ( -15.54421513559356782, -25.44239456788696785, 1.499999999999999556 ) ) ;
#12651 = CARTESIAN_POINT ( 'NONE',  ( 24.13073845333403966, -17.43243825926018786, -1.517345177934828815 ) ) ;
#12652 = FACE_OUTER_BOUND ( 'NONE', #2506, .T. ) ;
#12653 = CARTESIAN_POINT ( 'NONE',  ( 10.56870887191539587, 1.625881193364696831, 4.467071865485476856 ) ) ;
#12654 = ORIENTED_EDGE ( 'NONE', *, *, #16956, .T. ) ;
#12655 = CARTESIAN_POINT ( 'NONE',  ( -6.162550801365593856, 2.228590825266444142, 2.752080473201636845 ) ) ;
#12656 = ORIENTED_EDGE ( 'NONE', *, *, #17169, .F. ) ;
#12657 = EDGE_CURVE ( 'NONE', #6174, #31510, #6467, .T. ) ;
#12658 = CARTESIAN_POINT ( 'NONE',  ( -6.304531657079157192, -2.975847129947406522, -0.3127741368606805072 ) ) ;
#12659 = CARTESIAN_POINT ( 'NONE',  ( 24.73500000136559507, 3.156283516753366047, 0.9349337715887203748 ) ) ;
#12660 = CARTESIAN_POINT ( 'NONE',  ( 107.5345041083672584, 18.40851707499601631, 5.126370027289036457 ) ) ;
#12661 = CARTESIAN_POINT ( 'NONE',  ( -29.73484230743789070, 0.000000000000000000, 11.09540449768827308 ) ) ;
#12662 = CARTESIAN_POINT ( 'NONE',  ( -10.00000000000000000, 0.000000000000000000, 0.000000000000000000 ) ) ;
#12663 = ORIENTED_EDGE ( 'NONE', *, *, #20313, .F. ) ;
#12664 = CARTESIAN_POINT ( 'NONE',  ( 3.063284526839887167, -3.174628368996133432, 8.152713396088751452 ) ) ;
#12665 = DIRECTION ( 'NONE',  ( -1.000000000000000000, 0.000000000000000000, -0.000000000000000000 ) ) ;
#12666 = EDGE_LOOP ( 'NONE', ( #16535, #6663, #25312, #26789 ) ) ;
#12667 = CARTESIAN_POINT ( 'NONE',  ( 5.377543748152548986, 1.391664247347228045, 7.892520144992438702 ) ) ;
#12668 = APPROVAL_ROLE ( '' ) ;
#12669 = CARTESIAN_POINT ( 'NONE',  ( 28.66479303568530312, -6.738141520292279196, 4.033870043683038809 ) ) ;
#12670 = ADVANCED_FACE ( 'NONE', ( #1823 ), #26700, .F. ) ;
#12671 = CARTESIAN_POINT ( 'NONE',  ( 6.883866601413089370, 4.949663153219632683, -7.193114723270757516 ) ) ;
#12673 = DIRECTION ( 'NONE',  ( -1.000000000000000000, -0.000000000000000000, -0.000000000000000000 ) ) ;
#12672 = CARTESIAN_POINT ( 'NONE',  ( 0.7632845268429988561, 7.360373001717848140, -4.729683950891435451 ) ) ;
#12674 = ORIENTED_EDGE ( 'NONE', *, *, #15755, .F. ) ;
#12675 = ADVANCED_FACE ( 'NONE', ( #8379 ), #3208, .F. ) ;
#12676 = CARTESIAN_POINT ( 'NONE',  ( -8.000050800000002127, -2.680285808942373560, 1.376672160408170198 ) ) ;
#12677 = CARTESIAN_POINT ( 'NONE',  ( 3.529825581556955655E-16, 4.116875700062116117, -2.376879293651021019 ) ) ;
#12678 = CARTESIAN_POINT ( 'NONE',  ( 25.23500000136559507, -3.156283516753370044, -0.9349337715887220401 ) ) ;
#12679 = DIRECTION ( 'NONE',  ( 0.4999999999999978906, 0.8660254037844397068, 9.233562054644581322E-18 ) ) ;
#12681 = ORIENTED_EDGE ( 'NONE', *, *, #32303, .T. ) ;
#12680 = CARTESIAN_POINT ( 'NONE',  ( 107.6243858517459699, 18.92535819529473073, 5.093136976256313453 ) ) ;
#12682 = CARTESIAN_POINT ( 'NONE',  ( -6.262550801365593500, 3.521866450007987037, 0.3701630799359328372 ) ) ;
#12683 = CARTESIAN_POINT ( 'NONE',  ( 3.250000000000001332, 0.000000000000000000, -7.000000000000000888 ) ) ;
#12684 = CARTESIAN_POINT ( 'NONE',  ( 3.499999999999999556, 5.241389472434724084, -4.711457988287002685 ) ) ;
#12685 = CARTESIAN_POINT ( 'NONE',  ( 22.10999999999999943, 1.942864903642424146, 1.573300977624592534 ) ) ;
#12686 = ORIENTED_EDGE ( 'NONE', *, *, #23933, .T. ) ;
#12688 = ORIENTED_EDGE ( 'NONE', *, *, #4583, .F. ) ;
#12687 = CARTESIAN_POINT ( 'NONE',  ( 0.3076689118679166723, 4.089891983576842804, -9.439351442243262724 ) ) ;
#12689 = FACE_OUTER_BOUND ( 'NONE', #30801, .T. ) ;
#12690 = LINE ( 'NONE', #23063, #16515 ) ;
#12691 = CARTESIAN_POINT ( 'NONE',  ( 21.67250000136559507, 3.024605502323846729, -0.3178988483021056854 ) ) ;
#12692 = EDGE_CURVE ( 'NONE', #32326, #3441, #6093, .T. ) ;
#12693 = LINE ( 'NONE', #22897, #8625 ) ;
#12694 = CARTESIAN_POINT ( 'NONE',  ( -1.112385557803971414, -13.84060711329839322, -1.744598689557885551 ) ) ;
#12695 = CC_DESIGN_PERSON_AND_ORGANIZATION_ASSIGNMENT ( #8504, #16211, ( #5017 ) ) ;
#12696 = CARTESIAN_POINT ( 'NONE',  ( 1.750000000000000222, 4.058600654062850310, 7.468451026206211374 ) ) ;
#12697 = LINE ( 'NONE', #18212, #30595 ) ;
#12698 = CARTESIAN_POINT ( 'NONE',  ( 0.7632845268398871230, 0.000000000000000000, 0.000000000000000000 ) ) ;
#12699 = ORIENTED_EDGE ( 'NONE', *, *, #3684, .T. ) ;
#12700 = DIRECTION ( 'NONE',  ( 0.000000000000000000, 0.9063077870366514910, -0.4226182617406961106 ) ) ;
#12701 = CALENDAR_DATE ( 2026, 6, 10 ) ;
#12702 = CARTESIAN_POINT ( 'NONE',  ( 3.830085165118310759E-16, 4.467071865485471527, 1.625881193364712596 ) ) ;
#12703 = ORIENTED_EDGE ( 'NONE', *, *, #21484, .T. ) ;
#12704 = EDGE_CURVE ( 'NONE', #30416, #17249, #21024, .T. ) ;
#12705 = DIRECTION ( 'NONE',  ( 0.000000000000000000, -1.000000000000000000, 0.000000000000000000 ) ) ;
#12706 = ORIENTED_EDGE ( 'NONE', *, *, #21871, .T. ) ;
#12707 = CARTESIAN_POINT ( 'NONE',  ( 0.000000000000000000, -10.82112760146734587, -1.975651141462354987 ) ) ;
#12708 = EDGE_CURVE ( 'NONE', #32155, #11936, #16672, .T. ) ;
#12710 = ORIENTED_EDGE ( 'NONE', *, *, #18975, .T. ) ;
#12709 = CARTESIAN_POINT ( 'NONE',  ( 28.69308027625054436, -5.635843304107821972, -4.023790193015413408 ) ) ;
#12711 = ORIENTED_EDGE ( 'NONE', *, *, #13816, .F. ) ;
#12712 = CARTESIAN_POINT ( 'NONE',  ( 3.566513200368869096, -17.47573827932033197, -1.500000000000000000 ) ) ;
#12713 = CARTESIAN_POINT ( 'NONE',  ( 10.00000000000000000, 2.376879293651121383, -4.116875700062057497 ) ) ;
#12714 = CARTESIAN_POINT ( 'NONE',  ( 5.377543748152549874, -2.741043480754877582, -7.530955069117540646 ) ) ;
#12715 = LINE ( 'NONE', #20913, #7573 ) ;
#12717 = ORIENTED_EDGE ( 'NONE', *, *, #16698, .F. ) ;
#12716 = DIRECTION ( 'NONE',  ( 1.000000000000000000, -8.574039729943018344E-17, -0.000000000000000000 ) ) ;
#12718 = PLANE ( 'NONE',  #10818 ) ;
#12719 = CARTESIAN_POINT ( 'NONE',  ( 10.56870887191539587, 1.625881193364696831, 4.467071865485476856 ) ) ;
#12720 = CARTESIAN_POINT ( 'NONE',  ( -4.037246935524632541, -8.274097571364565695, 1.744146417483311451 ) ) ;
#12721 = CARTESIAN_POINT ( 'NONE',  ( 2.632061376486628301, -0.5000000000000000000, 1.500000000000000000 ) ) ;
#12723 = ORIENTED_EDGE ( 'NONE', *, *, #18670, .F. ) ;
#12722 = CARTESIAN_POINT ( 'NONE',  ( 108.0283028386853061, -18.47691595282699240, -4.359892190393998668 ) ) ;
#12724 = DIRECTION ( 'NONE',  ( 0.03487826274237457863, -0.9987827659587182882, 0.03487826274237499496 ) ) ;
#12725 = CARTESIAN_POINT ( 'NONE',  ( 2.494102553062040428, 10.32114304930246540, 2.161619314007376058 ) ) ;
#12726 = CARTESIAN_POINT ( 'NONE',  ( 24.73500000273118715, -2.486304738420683780, 0.2613211581691335383 ) ) ;
#12727 = DIRECTION ( 'NONE',  ( -8.541412920197208721E-17, -0.9961946980917449901, -0.08715574274766461904 ) ) ;
#12728 = DIRECTION ( 'NONE',  ( 0.000000000000000000, 0.5877852522924684742, 0.8090169943749507819 ) ) ;
#12729 = FACE_OUTER_BOUND ( 'NONE', #29284, .T. ) ;
#12730 = ORIENTED_EDGE ( 'NONE', *, *, #837, .F. ) ;
#12731 = LINE ( 'NONE', #32344, #32717 ) ;
#12732 = DIRECTION ( 'NONE',  ( 1.000000000000000000, 0.000000000000000000, 0.000000000000000000 ) ) ;
#12733 = CARTESIAN_POINT ( 'NONE',  ( -6.237550801365593145, 1.088641768524161613, 3.675193018007246959 ) ) ;
#12734 = ORIENTED_EDGE ( 'NONE', *, *, #27156, .T. ) ;
#12735 = LINE ( 'NONE', #7753, #651 ) ;
#12736 = CARTESIAN_POINT ( 'NONE',  ( 5.377543748152548986, 6.940565734314653845, -4.007137495034738706 ) ) ;
#12737 = CARTESIAN_POINT ( 'NONE',  ( 0.2678094507063553675, -7.640026513854723866, -1.500000000000000444 ) ) ;
#12738 = CARTESIAN_POINT ( 'NONE',  ( 10.22928983298388772, -12.18097484234047201, 1.000000000000000000 ) ) ;
#12739 = ADVANCED_FACE ( 'NONE', ( #6654 ), #11823, .T. ) ;
#12740 = VERTEX_POINT ( 'NONE', #27193 ) ;
#12741 = EDGE_CURVE ( 'NONE', #7166, #6030, #21039, .T. ) ;
#12742 = CARTESIAN_POINT ( 'NONE',  ( 5.377543748152551650, 6.139290821770257089, 5.151476664237498504 ) ) ;
#12743 = ORIENTED_EDGE ( 'NONE', *, *, #12981, .F. ) ;
#12744 = CARTESIAN_POINT ( 'NONE',  ( 2.357329895872532610, 1.335530315079654917, -10.75444571268653249 ) ) ;
#12746 = VERTEX_POINT ( 'NONE', #30563 ) ;
#12745 = DIRECTION ( 'NONE',  ( -1.000000000000000000, 0.000000000000000000, 0.000000000000000000 ) ) ;
#12747 = ORIENTED_EDGE ( 'NONE', *, *, #14839, .T. ) ;
#12748 = FACE_OUTER_BOUND ( 'NONE', #15704, .T. ) ;
#12749 = ORIENTED_EDGE ( 'NONE', *, *, #25835, .F. ) ;
#12750 = CARTESIAN_POINT ( 'NONE',  ( 0.000000000000000000, -4.472189673936843413, 8.264486777890091673 ) ) ;
#12752 = VERTEX_POINT ( 'NONE', #20188 ) ;
#12751 = DIRECTION ( 'NONE',  ( -0.000000000000000000, 0.000000000000000000, 1.000000000000000000 ) ) ;
#12753 = CARTESIAN_POINT ( 'NONE',  ( 10.67617967751839458, -15.18094839191508960, -1.754323820777800025 ) ) ;
#12754 = CARTESIAN_POINT ( 'NONE',  ( 18.68312535291511267, -6.719245328341675538, 2.639238440967430321 ) ) ;
#12755 = CARTESIAN_POINT ( 'NONE',  ( 29.18953645666585217, -9.308308156628569918, 0.07017451552781736601 ) ) ;
#12756 = CARTESIAN_POINT ( 'NONE',  ( 0.000000000000000000, 0.000000000000000000, 0.000000000000000000 ) ) ;
#12757 = B_SPLINE_CURVE_WITH_KNOTS ( 'NONE', 3,
 ( #19543, #19383, #6667, #4322, #14499, #29740 ),
 .UNSPECIFIED., .F., .F.,
 ( 4, 2, 4 ),
 ( 0.000000000000000000, 0.0009761895971467555739, 0.001952379194293511148 ),
 .UNSPECIFIED. ) ;
#12758 = CARTESIAN_POINT ( 'NONE',  ( 1.302051718648536305, -9.310916516917917107, 1.499999999999999334 ) ) ;
#12759 = CARTESIAN_POINT ( 'NONE',  ( -3.687509558818933845E-13, 7.944914065997426889, -7.533794289458821680 ) ) ;
#12760 = DIRECTION ( 'NONE',  ( -1.000000000000000000, -5.361488761196502513E-16, 0.000000000000000000 ) ) ;
#12761 = FACE_OUTER_BOUND ( 'NONE', #23322, .T. ) ;
#12762 = CARTESIAN_POINT ( 'NONE',  ( 6.524595126109738352, 8.613374939462827840, 0.8869162863044809386 ) ) ;
#12763 = CARTESIAN_POINT ( 'NONE',  ( 0.000000000000000000, 1.459547570502368385, 6.894905428400277536 ) ) ;
#12764 = CARTESIAN_POINT ( 'NONE',  ( 23.84310522038115465, -4.329614468541457484, 4.522129901861162260 ) ) ;
#12765 = LINE ( 'NONE', #93, #29530 ) ;
#12766 = ORIENTED_EDGE ( 'NONE', *, *, #30380, .F. ) ;
#12767 = CARTESIAN_POINT ( 'NONE',  ( -6.337550801365593678, 3.368539882008727115, 1.828967928396026954 ) ) ;
#12768 = ADVANCED_FACE ( 'NONE', ( #14817 ), #2479, .T. ) ;
#12769 = DIRECTION ( 'NONE',  ( -1.000000000000000000, -0.000000000000000000, 0.000000000000000000 ) ) ;
#12770 = CARTESIAN_POINT ( 'NONE',  ( 20.55936702064902377, -21.63501724500277135, -1.474765012619939863 ) ) ;
#12771 = VERTEX_POINT ( 'NONE', #4493 ) ;
#12772 = CARTESIAN_POINT ( 'NONE',  ( 18.77131501682890757, -5.733461880277683775, -4.171847256157208861 ) ) ;
#12773 = CARTESIAN_POINT ( 'NONE',  ( 2.589202944057211742, 7.715757980413557426, 6.846250362091539365 ) ) ;
#12774 = AXIS2_PLACEMENT_3D ( 'NONE', #29997, #7089, #17294 ) ;
#12775 = VERTEX_POINT ( 'NONE', #17848 ) ;
#12776 = CARTESIAN_POINT ( 'NONE',  ( 0.000000000000000000, 0.000000000000000000, 0.000000000000000000 ) ) ;
#12778 = EDGE_LOOP ( 'NONE', ( #6669, #9009, #21572, #20425 ) ) ;
#12777 = CARTESIAN_POINT ( 'NONE',  ( 18.60402535543785518, -7.603424548862136589, 0.02339150517593243869 ) ) ;
#12779 = ORIENTED_EDGE ( 'NONE', *, *, #23951, .T. ) ;
#12780 = CARTESIAN_POINT ( 'NONE',  ( 6.353200070539462452, -18.33841314941795986, 1.748782779367867191 ) ) ;
#12781 = ORIENTED_EDGE ( 'NONE', *, *, #15421, .F. ) ;
#12782 = AXIS2_PLACEMENT_3D ( 'NONE', #6606, #4754, #30191 ) ;
#12783 =( BOUNDED_CURVE ( )  B_SPLINE_CURVE ( 2, ( #778, #11272, #3455, #29165, #28529, #10960, #13439, #6253, #23660, #592, #8436 ),
 .UNSPECIFIED., .F., .F. ) 
 B_SPLINE_CURVE_WITH_KNOTS ( ( 3, 2, 2, 2, 2, 3 ),
 ( 0.5966116191895003418, 0.5999999999999999778, 0.6250000000000000000, 0.6500000000000000222, 0.6750000000000000444, 0.6966116191895003196 ),
 .UNSPECIFIED. ) 
 CURVE ( )  GEOMETRIC_REPRESENTATION_ITEM ( )  RATIONAL_B_SPLINE_CURVE ( ( 0.9821626249036858880, 0.9896829947469992783, 1.000000000000000000, 0.9238795325112867385, 1.000000000000000000, 0.9238795325112867385, 1.000000000000000000, 0.9238795325112867385, 1.000000000000000000, 0.9341965377642874602, 0.9821626249036858880 ) ) 
 REPRESENTATION_ITEM ( '' )  );
#12784 = LINE ( 'NONE', #2115, #26715 ) ;
#12786 = EDGE_LOOP ( 'NONE', ( #8292, #26170, #8769, #30947 ) ) ;
#12785 = CARTESIAN_POINT ( 'NONE',  ( 0.5032040285305338090, -9.002252291025264697, -3.698073368203398825 ) ) ;
#12787 = CARTESIAN_POINT ( 'NONE',  ( 18.58227844715246135, -7.846511338401735536, 2.713652344655544724 ) ) ;
#12788 = DIRECTION ( 'NONE',  ( -1.000000000000000000, 0.000000000000000000, 0.000000000000000000 ) ) ;
#12789 = LINE ( 'NONE', #9623, #1282 ) ;
#12790 = CARTESIAN_POINT ( 'NONE',  ( 10.52034268205830259, -3.993798362933288271, -3.024842911000732215 ) ) ;
#12791 = ORIENTED_EDGE ( 'NONE', *, *, #16475, .F. ) ;
#12792 = CARTESIAN_POINT ( 'NONE',  ( 6.880159329304571081, -6.224287131858844191, 6.122988934091259772 ) ) ;
#12793 = CARTESIAN_POINT ( 'NONE',  ( -5.834205823644825095, 18.00000000000000355, -2.241549108841658366 ) ) ;
#12794 = EDGE_CURVE ( 'NONE', #8778, #26510, #32811, .T. ) ;
#12795 = PLANE ( 'NONE',  #20368 ) ;
#12796 = CARTESIAN_POINT ( 'NONE',  ( 101.6962914994147411, -2.525156800924736267, -3.393559278664259882 ) ) ;
#12797 = CARTESIAN_POINT ( 'NONE',  ( -8.000050800000009232, 0.3876333558353860509, 3.203076781024368547 ) ) ;
#12798 = CARTESIAN_POINT ( 'NONE',  ( -50.60000000000000142, -21.93932300454937945, 1.000000000000000000 ) ) ;
#12799 = DIRECTION ( 'NONE',  ( 0.000000000000000000, 0.000000000000000000, 1.000000000000000000 ) ) ;
#12800 = CARTESIAN_POINT ( 'NONE',  ( -29.24402871571405882, -25.93932300454937945, 11.50000000000000000 ) ) ;
#12801 = AXIS2_PLACEMENT_3D ( 'NONE', #32896, #23189, #12636 ) ;
#12802 = ORIENTED_EDGE ( 'NONE', *, *, #23011, .T. ) ;
#12803 = EDGE_CURVE ( 'NONE', #32781, #9763, #23009, .T. ) ;
#12804 = CARTESIAN_POINT ( 'NONE',  ( -6.512550801365594388, -1.088641768524163389, -3.675193018007246071 ) ) ;
#12805 = ORIENTED_EDGE ( 'NONE', *, *, #24551, .F. ) ;
#12806 = CARTESIAN_POINT ( 'NONE',  ( -8.050050799999999285, -1.549418761218565477, 2.853674364686380471 ) ) ;
#12807 = CIRCLE ( 'NONE', #5869, 7.000000000000000888 ) ;
#12808 = CARTESIAN_POINT ( 'NONE',  ( 107.9955289544189725, 18.15326337889181829, 5.055346619445248102 ) ) ;
#12809 = EDGE_CURVE ( 'NONE', #31932, #22762, #28048, .T. ) ;
#12810 = CARTESIAN_POINT ( 'NONE',  ( 2.838906197121284336, 0.000000000000000000, -1.380701634710809200 ) ) ;
#12811 = CARTESIAN_POINT ( 'NONE',  ( 7.650166298461252623, -9.403575860120110264, 1.500000000000000000 ) ) ;
#12812 = VERTEX_POINT ( 'NONE', #9634 ) ;
#12813 = CARTESIAN_POINT ( 'NONE',  ( 0.6424020794401417156, -8.982780240576513364, 2.300561732649537561 ) ) ;
#12814 = EDGE_CURVE ( 'NONE', #29340, #22752, #19439, .T. ) ;
#12815 = VERTEX_POINT ( 'NONE', #14668 ) ;
#12816 = CARTESIAN_POINT ( 'NONE',  ( -55.09999999999999432, -10.96966150227468972, 7.500000000000000000 ) ) ;
#12817 = CALENDAR_DATE ( 2026, 6, 10 ) ;
#12818 = CARTESIAN_POINT ( 'NONE',  ( 40.88384453718996525, -6.869468092516608060, 4.033869542149528087 ) ) ;
#12819 = ADVANCED_FACE ( 'NONE', ( #19858 ), #15319, .T. ) ;
#12820 = CIRCLE ( 'NONE', #12302, 10.94895958125474245 ) ;
#12821 = DIRECTION ( 'NONE',  ( -1.000000000000000000, -0.000000000000000000, -0.000000000000000000 ) ) ;
#12822 = AXIS2_PLACEMENT_3D ( 'NONE', #15235, #15386, #28262 ) ;
#12824 = CARTESIAN_POINT ( 'NONE',  ( 5.612974259723590542, 7.786824029658800939, -2.621729824970306044 ) ) ;
#12823 = FACE_OUTER_BOUND ( 'NONE', #26602, .T. ) ;
#12825 = ORIENTED_EDGE ( 'NONE', *, *, #7758, .F. ) ;
#12826 = AXIS2_PLACEMENT_3D ( 'NONE', #19676, #29869, #21009 ) ;
#12827 = CARTESIAN_POINT ( 'NONE',  ( -7.500050802731187183, 2.853674364686379583, 1.549418761218565921 ) ) ;
#12828 = LINE ( 'NONE', #22561, #15534 ) ;
#12829 = CARTESIAN_POINT ( 'NONE',  ( 23.48500000136559862, 0.9349337715887185984, -3.156283516753368268 ) ) ;
#12830 = EDGE_CURVE ( 'NONE', #26383, #17238, #5048, .T. ) ;
#12831 = CARTESIAN_POINT ( 'NONE',  ( 12.23116174109277310, -15.17372397490200875, -1.500000000000000000 ) ) ;
#12832 = VECTOR ( 'NONE', #13144, 1000.000000000000000 ) ;
#12834 = ORIENTED_EDGE ( 'NONE', *, *, #9062, .T. ) ;
#12833 = CARTESIAN_POINT ( 'NONE',  ( 108.6155529559672885, -15.79924867777639186, 1.500000000000000444 ) ) ;
#12835 = CARTESIAN_POINT ( 'NONE',  ( -5.362550801365593145, 2.228590825266444142, 2.752080473201636845 ) ) ;
#12836 = DIRECTION ( 'NONE',  ( -1.000000000000000000, 0.000000000000000000, -0.000000000000000000 ) ) ;
#12837 = CARTESIAN_POINT ( 'NONE',  ( 6.883866621640342132, -7.111352071735057123, 5.066432324612699212 ) ) ;
#12838 = CARTESIAN_POINT ( 'NONE',  ( 22.25111450864416085, -3.256483526998273983E-15, 2.499999999999998668 ) ) ;
#12839 = ORIENTED_EDGE ( 'NONE', *, *, #12642, .T. ) ;
#12840 = ORIENTED_EDGE ( 'NONE', *, *, #22432, .F. ) ;
#12841 = B_SPLINE_CURVE_WITH_KNOTS ( 'NONE', 3,
 ( #5633, #30732, #8296, #5779, #18636, #5459, #7804, #440, #28834, #26174 ),
 .UNSPECIFIED., .F., .F.,
 ( 4, 2, 2, 2, 4 ),
 ( 1.968338519010642687E-07, 0.0005467930078056964724, 0.001093389181759491739, 0.001639985355713287222, 0.002186581529667082704 ),
 .UNSPECIFIED. ) ;
#12842 = CARTESIAN_POINT ( 'NONE',  ( 108.5619817448483815, 15.65002148400668247, -0.7764623266635863885 ) ) ;
#12843 = CARTESIAN_POINT ( 'NONE',  ( 0.08034253656881387706, 5.242601083769395487, -9.429377841196931342 ) ) ;
#12844 = CIRCLE ( 'NONE', #4843, 302.4235430809786749 ) ;
#12845 = EDGE_CURVE ( 'NONE', #8184, #12626, #30703, .T. ) ;
#12846 = CARTESIAN_POINT ( 'NONE',  ( 22.98500000136559862, -0.9349337715887247047, 3.156283516753367824 ) ) ;
#12847 = AXIS2_PLACEMENT_3D ( 'NONE', #29072, #6159, #16491 ) ;
#12848 = VECTOR ( 'NONE', #30893, 1000.000000000000114 ) ;
#12849 = CARTESIAN_POINT ( 'NONE',  ( 68.99418471616174031, -4.594926857588857771, 3.390608975014814064 ) ) ;
#12850 = CARTESIAN_POINT ( 'NONE',  ( 0.000000000000000000, 19.51744974835125035, 0.000000000000000000 ) ) ;
#12851 = CARTESIAN_POINT ( 'NONE',  ( 18.75828436641558028, -5.879118399717575549, 3.993434336035622589 ) ) ;
#12852 = CIRCLE ( 'NONE', #18732, 3.000000000000000000 ) ;
#12853 = EDGE_CURVE ( 'NONE', #28913, #11008, #13054, .T. ) ;
#12854 = DIRECTION ( 'NONE',  ( -1.000000000000000000, 0.000000000000000000, 0.000000000000000000 ) ) ;
#12855 = CARTESIAN_POINT ( 'NONE',  ( 107.9808716746042592, -17.79391898944832207, 4.343976358958649975 ) ) ;
#12856 = ORIENTED_EDGE ( 'NONE', *, *, #21047, .T. ) ;
#12857 = CARTESIAN_POINT ( 'NONE',  ( 0.6903785682175527239, -7.668066208469608291, 4.901993410350687697 ) ) ;
#12858 = EDGE_CURVE ( 'NONE', #31776, #10511, #15167, .T. ) ;
#12859 = AXIS2_PLACEMENT_3D ( 'NONE', #21604, #1890, #6713 ) ;
#12860 = CALENDAR_DATE ( 2026, 6, 10 ) ;
#12861 = CARTESIAN_POINT ( 'NONE',  ( 47.99837860531645362, -3.577301031424839017, 2.713652344655542503 ) ) ;
#12862 = ORIENTED_EDGE ( 'NONE', *, *, #28673, .F. ) ;
#12863 = DIRECTION ( 'NONE',  ( 1.000000000000000000, 0.000000000000000000, 0.000000000000000000 ) ) ;
#12864 = ORIENTED_EDGE ( 'NONE', *, *, #6356, .T. ) ;
#12865 = CARTESIAN_POINT ( 'NONE',  ( -5.200050802731187360, 3.113457007523260156, -0.9222479816126439855 ) ) ;
#12867 = ORIENTED_EDGE ( 'NONE', *, *, #8760, .T. ) ;
#12866 = CARTESIAN_POINT ( 'NONE',  ( 69.01361805596027921, -4.978092444658805960, -4.006107570160923892 ) ) ;
#12868 = AXIS2_PLACEMENT_3D ( 'NONE', #17459, #7111, #27507 ) ;
#12869 = ORIENTED_EDGE ( 'NONE', *, *, #28566, .F. ) ;
#12870 = CARTESIAN_POINT ( 'NONE',  ( -3.889464452585704723, -3.181828567483031112, 1.500000000000000000 ) ) ;
#12871 = CARTESIAN_POINT ( 'NONE',  ( -6.912550801365593856, 1.088641768524161613, 3.675193018007246959 ) ) ;
#12872 = AXIS2_PLACEMENT_3D ( 'NONE', #22894, #25413, #2869 ) ;
#12873 = CARTESIAN_POINT ( 'NONE',  ( 25.75999999999999801, -2.208672634433321348E-15, 0.000000000000000000 ) ) ;
#12875 = EDGE_CURVE ( 'NONE', #10748, #30917, #4665, .T. ) ;
#12874 = VECTOR ( 'NONE', #7692, 1000.000000000000000 ) ;
#12876 = DIRECTION ( 'NONE',  ( -0.9975973382524639943, -0.06927878976713693071, 0.000000000000000000 ) ) ;
#12877 = APPROVAL ( #26907, 'UNSPECIFIED' ) ;
#12879 = VERTEX_POINT ( 'NONE', #24864 ) ;
#12878 = DIRECTION ( 'NONE',  ( -0.4999999999999982236, -0.8660254037844398178, 0.000000000000000000 ) ) ;
#12880 = CARTESIAN_POINT ( 'NONE',  ( 107.6540478345876579, -20.31198981111268864, 1.799433580832300761 ) ) ;
#12881 = DIRECTION ( 'NONE',  ( -1.000000000000000000, 0.000000000000000000, 0.000000000000000000 ) ) ;
#12882 = CARTESIAN_POINT ( 'NONE',  ( -1.898205096934858283, -13.58783804611283408, 1.500000000000000000 ) ) ;
#12883 = CARTESIAN_POINT ( 'NONE',  ( 21.29750000136559507, -2.363507492473152283, -1.913930629741525280 ) ) ;
#12884 = VECTOR ( 'NONE', #11565, 1000.000000000000000 ) ;
#12885 = CYLINDRICAL_SURFACE ( 'NONE', #26199, 5.010000000000000675 ) ;
#12887 = ORIENTED_EDGE ( 'NONE', *, *, #1304, .F. ) ;
#12886 = CARTESIAN_POINT ( 'NONE',  ( 18.60402535543785518, -7.603424548862136589, -0.07017451552783579571 ) ) ;
#12888 = DIRECTION ( 'NONE',  ( 0.4999999999999977796, 0.8660254037844398178, 0.000000000000000000 ) ) ;
#12889 = AXIS2_PLACEMENT_3D ( 'NONE', #13914, #23958, #21472 ) ;
#12890 = CARTESIAN_POINT ( 'NONE',  ( -31.18783180709124636, -25.44850941282521006, 1.500000000000000000 ) ) ;
#12891 = CARTESIAN_POINT ( 'NONE',  ( 21.86000000136559507, -0.9349337715887248157, 3.156283516753367824 ) ) ;
#12892 = B_SPLINE_CURVE_WITH_KNOTS ( 'NONE', 3,
 ( #12667, #4816, #10148, #20372, #14833, #14996, #6544, #32131, #21911, #30587 ),
 .UNSPECIFIED., .F., .F.,
 ( 4, 2, 2, 2, 4 ),
 ( 3.032460776719120378E-07, 0.0005479053915603968516, 0.001095507537043121900, 0.001643109682525846840, 0.002190711828008571564 ),
 .UNSPECIFIED. ) ;
#12893 = EDGE_CURVE ( 'NONE', #18598, #293, #27474, .T. ) ;
#12894 = CARTESIAN_POINT ( 'NONE',  ( 6.749760686538667009, 0.000000000000000000, 0.000000000000000000 ) ) ;
#12895 = FACE_OUTER_BOUND ( 'NONE', #25322, .T. ) ;
#12896 = CARTESIAN_POINT ( 'NONE',  ( -0.2059365608663963898, 0.000000000000000000, 1.000000000000000000 ) ) ;
#12897 = ORIENTED_EDGE ( 'NONE', *, *, #26113, .T. ) ;
#12898 = CARTESIAN_POINT ( 'NONE',  ( 108.0223665316818114, -18.39143460874491964, 4.509626086723559801 ) ) ;
#12899 = VECTOR ( 'NONE', #4220, 1000.000000000000114 ) ;
#12900 = CARTESIAN_POINT ( 'NONE',  ( -60.22964952008683781, -5.531562813905956055, 2.028141679950118625 ) ) ;
#12901 = CARTESIAN_POINT ( 'NONE',  ( 107.4997235041507793, -18.08180639291762404, -5.137882848214009535 ) ) ;
#12902 = ORIENTED_EDGE ( 'NONE', *, *, #23807, .F. ) ;
#12903 = VECTOR ( 'NONE', #9320, 1000.000000000000227 ) ;
#12904 = AXIS2_PLACEMENT_3D ( 'NONE', #12939, #10756, #18118 ) ;
#12905 = CIRCLE ( 'NONE', #12380, 2.999999999999999556 ) ;
#12906 = CARTESIAN_POINT ( 'NONE',  ( 25.46715431016588482, 2.408328468251813348, 1.329981640288168121 ) ) ;
#12907 = CARTESIAN_POINT ( 'NONE',  ( 7.064632940817592299, 7.906491560603718050, -3.748318449932210417 ) ) ;
#12908 = CARTESIAN_POINT ( 'NONE',  ( 0.000000000000000000, 0.000000000000000000, 0.000000000000000000 ) ) ;
#12910 = CARTESIAN_POINT ( 'NONE',  ( 7.249760686538667009, 2.210816291636326092, -8.466096581343458993 ) ) ;
#12909 = CIRCLE ( 'NONE', #25209, 2.999999999999999112 ) ;
#12911 = ORIENTED_EDGE ( 'NONE', *, *, #16167, .T. ) ;
#12912 = AXIS2_PLACEMENT_3D ( 'NONE', #5409, #20783, #30986 ) ;
#12913 = AXIS2_PLACEMENT_3D ( 'NONE', #28717, #30768, #7839 ) ;
#12914 = DIRECTION ( 'NONE',  ( 0.000000000000000000, -0.7071067811865442421, 0.7071067811865509034 ) ) ;
#12915 = ORIENTED_EDGE ( 'NONE', *, *, #1094, .F. ) ;
#12916 = CARTESIAN_POINT ( 'NONE',  ( 18.58227844715246135, -7.846511338401735536, 2.713652344655544724 ) ) ;
#12918 = ORIENTED_EDGE ( 'NONE', *, *, #3257, .T. ) ;
#12917 = DIRECTION ( 'NONE',  ( 0.000000000000000000, 1.000000000000000000, 0.000000000000000000 ) ) ;
#12919 = ORIENTED_EDGE ( 'NONE', *, *, #7749, .T. ) ;
#12920 = CARTESIAN_POINT ( 'NONE',  ( 10.56870887191539587, 4.467071865485470639, 1.625881193364712596 ) ) ;
#12921 = EDGE_CURVE ( 'NONE', #5699, #21989, #16602, .T. ) ;
#12922 = VERTEX_POINT ( 'NONE', #26033 ) ;
#12923 = CARTESIAN_POINT ( 'NONE',  ( -32.85000000000000142, -10.96966150227469328, -1.499999999999999556 ) ) ;
#12925 = ORIENTED_EDGE ( 'NONE', *, *, #24125, .T. ) ;
#12924 = CARTESIAN_POINT ( 'NONE',  ( 108.6155529559672885, -15.79924867777639186, 1.500000000000000000 ) ) ;
#12926 = AXIS2_PLACEMENT_3D ( 'NONE', #14215, #24572, #16897 ) ;
#12927 = VERTEX_POINT ( 'NONE', #23500 ) ;
#12928 = CARTESIAN_POINT ( 'NONE',  ( 8.787183276125896114, -14.57090831734663006, -1.754908492369190887 ) ) ;
#12929 = AXIS2_PLACEMENT_3D ( 'NONE', #30201, #14788, #20156 ) ;
#12930 = CARTESIAN_POINT ( 'NONE',  ( 18.67472101454464450, -6.813188964052660168, 2.487811220254955380 ) ) ;
#12931 = AXIS2_PLACEMENT_3D ( 'NONE', #31872, #24946, #27288 ) ;
#12932 = CARTESIAN_POINT ( 'NONE',  ( 3.499999999999999556, 3.771202944355708020, 4.982773259188384429 ) ) ;
#12933 = CARTESIAN_POINT ( 'NONE',  ( 10.55147673363119232, -2.285372942704923194, -4.458382051008217495 ) ) ;
#12934 = CARTESIAN_POINT ( 'NONE',  ( 0.2099939045493650069, -10.28101406640744209, 2.171920878037989056 ) ) ;
#12935 = AXIS2_PLACEMENT_3D ( 'NONE', #9940, #10277, #20154 ) ;
#12936 = VECTOR ( 'NONE', #15971, 1000.000000000000000 ) ;
#12937 = VECTOR ( 'NONE', #2630, 999.9999999999998863 ) ;
#12938 = DIRECTION ( 'NONE',  ( -0.000000000000000000, -0.000000000000000000, 1.000000000000000000 ) ) ;
#12939 = CARTESIAN_POINT ( 'NONE',  ( 10.56870887191539587, 4.467071865485470639, 1.625881193364712596 ) ) ;
#12940 = FACE_OUTER_BOUND ( 'NONE', #16426, .T. ) ;
#12941 = AXIS2_PLACEMENT_3D ( 'NONE', #27597, #4699, #12373 ) ;
#12942 = EDGE_CURVE ( 'NONE', #516, #11273, #22613, .T. ) ;
#12943 = EDGE_CURVE ( 'NONE', #16345, #31994, #5643, .T. ) ;
#12944 = AXIS2_PLACEMENT_3D ( 'NONE', #24537, #32432, #1660 ) ;
#12945 = CARTESIAN_POINT ( 'NONE',  ( 43.74661801760413482, -24.08792321988613594, 1.500000000000000000 ) ) ;
#12946 = CARTESIAN_POINT ( 'NONE',  ( 18.60402535543785518, -7.603424548862136589, -0.07017451552783579571 ) ) ;
#12947 = CARTESIAN_POINT ( 'NONE',  ( 0.4370649308509315101, 8.480516373469937363, 5.155378858006763210 ) ) ;
#12948 = CARTESIAN_POINT ( 'NONE',  ( 7.064632951172269415, -6.147671362329258926, 6.226446564517893911 ) ) ;
#12949 = EDGE_CURVE ( 'NONE', #18415, #429, #24747, .T. ) ;
#12950 = CARTESIAN_POINT ( 'NONE',  ( 4.749760686538667009, 2.741043480755029016, -7.530955069117485579 ) ) ;
#12951 = CARTESIAN_POINT ( 'NONE',  ( -34.98223484310472031, 0.5000000000000000000, -2.482234843104711430 ) ) ;
#12952 = VERTEX_POINT ( 'NONE', #28697 ) ;
#12953 = CARTESIAN_POINT ( 'NONE',  ( -4.987550801365594033, 0.3701630799359330593, -3.521866450007987037 ) ) ;
#12954 = CONICAL_SURFACE ( 'NONE', #8138, 2.499999999999996891, 1.029744258676653867 ) ;
#12955 = VECTOR ( 'NONE', #8242, 1000.000000000000000 ) ;
#12956 = CARTESIAN_POINT ( 'NONE',  ( 7.249760686538667009, 4.973063321323876629, 7.199384779417138169 ) ) ;
#12957 = CARTESIAN_POINT ( 'NONE',  ( 108.8138202772576903, 17.05235780320132122, 4.110854392070696584 ) ) ;
#12959 = ORIENTED_EDGE ( 'NONE', *, *, #26555, .T. ) ;
#12958 = AXIS2_PLACEMENT_3D ( 'NONE', #24068, #31950, #8529 ) ;
#12960 = DIRECTION ( 'NONE',  ( -1.000000000000000000, -0.000000000000000000, 0.000000000000000000 ) ) ;
#12961 = CIRCLE ( 'NONE', #25792, 297.4345239564032681 ) ;
#12962 = AXIS2_PLACEMENT_3D ( 'NONE', #20979, #5266, #25650 ) ;
#12963 = ORIENTED_EDGE ( 'NONE', *, *, #2190, .T. ) ;
#12964 = CARTESIAN_POINT ( 'NONE',  ( 23.95058674323829706, -2.449331254355760823, -0.07017451552781585333 ) ) ;
#12965 = DATE_AND_TIME ( #30537, #29065 ) ;
#12966 = AXIS2_PLACEMENT_3D ( 'NONE', #9467, #22348, #9629 ) ;
#12968 = EDGE_LOOP ( 'NONE', ( #8783, #18853, #31651, #30444 ) ) ;
#12967 = DIRECTION ( 'NONE',  ( 0.000000000000000000, 0.000000000000000000, -1.000000000000000000 ) ) ;
#12969 = VERTEX_POINT ( 'NONE', #16141 ) ;
#12970 = CARTESIAN_POINT ( 'NONE',  ( -4.062270432330101322, -5.105425442540494352, 1.745843391288832258 ) ) ;
#12971 = CONICAL_SURFACE ( 'NONE', #24177, 301.6269746700523342, 0.4915790642873871796 ) ;
#12972 = AXIS2_PLACEMENT_3D ( 'NONE', #30992, #18453, #7915 ) ;
#12973 = VERTEX_POINT ( 'NONE', #5790 ) ;
#12974 = CARTESIAN_POINT ( 'NONE',  ( 21.24290772321993970, 0.1310194482076003919, 2.499999999999998668 ) ) ;
#12976 = ORIENTED_EDGE ( 'NONE', *, *, #5515, .T. ) ;
#12975 = DIRECTION ( 'NONE',  ( -1.000000000000000000, -0.000000000000000000, -0.000000000000000000 ) ) ;
#12977 = CARTESIAN_POINT ( 'NONE',  ( 23.58793147791972444, -8.793627369988312736, 1.915219082070893863 ) ) ;
#12978 = CARTESIAN_POINT ( 'NONE',  ( 108.0379352182121835, -18.61561982177950725, 4.067192897739825952 ) ) ;
#12979 = DIRECTION ( 'NONE',  ( -1.000000000000000000, 0.000000000000000000, 0.000000000000000000 ) ) ;
#12980 = CARTESIAN_POINT ( 'NONE',  ( 10.00000000000000000, -1.745506336992504507E-14, 4.753758587302147731 ) ) ;
#12981 = EDGE_CURVE ( 'NONE', #13763, #22300, #17327, .T. ) ;
#12982 = VERTEX_POINT ( 'NONE', #800 ) ;
#12983 = AXIS2_PLACEMENT_3D ( 'NONE', #25367, #9464, #12490 ) ;
#12984 = AXIS2_PLACEMENT_3D ( 'NONE', #3355, #13679, #3667 ) ;
#12985 = LINE ( 'NONE', #10316, #563 ) ;
#12986 = CYLINDRICAL_SURFACE ( 'NONE', #15617, 5.010000000000000675 ) ;
#12987 = CARTESIAN_POINT ( 'NONE',  ( 102.5153059484011919, -5.316817625850402962, -1.873789182721711688 ) ) ;
#12988 = CARTESIAN_POINT ( 'NONE',  ( -6.900050802731187538, 1.549418761218566143, -2.853674364686379583 ) ) ;
#12989 = AXIS2_PLACEMENT_3D ( 'NONE', #11790, #11978, #21994 ) ;
#12990 = EDGE_CURVE ( 'NONE', #12106, #13240, #22663, .T. ) ;
#12991 = AXIS2_PLACEMENT_3D ( 'NONE', #21824, #26675, #32036 ) ;
#12993 = ADVANCED_FACE ( 'NONE', ( #10978 ), #28196, .F. ) ;
#12992 = AXIS2_PLACEMENT_3D ( 'NONE', #18254, #5579, #28629 ) ;
#12994 = CARTESIAN_POINT ( 'NONE',  ( 24.45151689496773173, -17.43764607375594977, 1.460555297092053895 ) ) ;
#12995 = DIRECTION ( 'NONE',  ( 1.000000000000000000, 0.000000000000000000, 0.000000000000000000 ) ) ;
#12996 = CARTESIAN_POINT ( 'NONE',  ( -56.32565245118806274, 0.3500057972172317955, -1.478456117012219462 ) ) ;
#12997 = CARTESIAN_POINT ( 'NONE',  ( -1.152183934781129714E-14, 21.49000000000002331, -1.050000000000000044 ) ) ;
#12998 = ORIENTED_EDGE ( 'NONE', *, *, #22927, .T. ) ;
#12999 = LOCAL_TIME ( 16, 7, 10.00000000000000000, #25261 ) ;
#13000 = CARTESIAN_POINT ( 'NONE',  ( -5.012550801365594388, -3.368539882008727115, -1.828967928396028064 ) ) ;
#13001 = ORIENTED_EDGE ( 'NONE', *, *, #5401, .T. ) ;
#13002 = CARTESIAN_POINT ( 'NONE',  ( -3.704531657079157103, 0.3127741368606810068, -2.975847129947406522 ) ) ;
#13003 = CARTESIAN_POINT ( 'NONE',  ( 3.499999999999999556, 1.106368468154430129, 8.427689411260576691 ) ) ;
#13004 = CARTESIAN_POINT ( 'NONE',  ( 2.893040194807178001, -11.59888121906014113, 1.759635999373791782 ) ) ;
#13005 = CARTESIAN_POINT ( 'NONE',  ( 24.38441422957166083, -17.22282062799744295, 1.000000000000000000 ) ) ;
#13006 = ORIENTED_EDGE ( 'NONE', *, *, #29854, .F. ) ;
#13007 = CARTESIAN_POINT ( 'NONE',  ( 54.94526044243337282, -5.359369332727098367, -3.993434333344310083 ) ) ;
#13008 =( BOUNDED_CURVE ( )  B_SPLINE_CURVE ( 3, ( #7614, #30869, #7789, #17982 ),
 .UNSPECIFIED., .F., .F. ) 
 B_SPLINE_CURVE_WITH_KNOTS ( ( 4, 4 ),
 ( 0.6009777071450013164, 1.570796326794896558 ),
 .UNSPECIFIED. ) 
 CURVE ( )  GEOMETRIC_REPRESENTATION_ITEM ( )  RATIONAL_B_SPLINE_CURVE ( ( 1.000000000000000000, 0.9231448173254019895, 0.9231448173254019895, 1.000000000000000000 ) ) 
 REPRESENTATION_ITEM ( '' )  );
#13009 = AXIS2_PLACEMENT_3D ( 'NONE', #5466, #15658, #13142 ) ;
#13010 = VERTEX_POINT ( 'NONE', #26368 ) ;
#13011 = CARTESIAN_POINT ( 'NONE',  ( 2.857987933995208785, -0.6743480930025086417, -9.536462466387789050 ) ) ;
#13012 = APPROVAL_ROLE ( '' ) ;
#13013 = CARTESIAN_POINT ( 'NONE',  ( 54.97462353180808492, -6.412592106988439511, 4.112224493134436720 ) ) ;
#13014 = AXIS2_PLACEMENT_3D ( 'NONE', #10773, #3444, #5765 ) ;
#13015 = CIRCLE ( 'NONE', #11945, 4.999999999999997335 ) ;
#13016 = DIRECTION ( 'NONE',  ( 8.541412920197216117E-17, 0.9961946980917455452, -0.08715574274765799934 ) ) ;
#13018 = LINE ( 'NONE', #18184, #31077 ) ;
#13017 = CARTESIAN_POINT ( 'NONE',  ( 0.3749743454410884302, -9.839947797887033332, -2.260462012960365197 ) ) ;
#13019 = EDGE_CURVE ( 'NONE', #4058, #24916, #31052, .T. ) ;
#13020 = ORIENTED_EDGE ( 'NONE', *, *, #423, .T. ) ;
#13021 = LOCAL_TIME ( 16, 7, 10.00000000000000000, #10339 ) ;
#13022 = DIRECTION ( 'NONE',  ( -1.000000000000000000, -0.000000000000000000, -0.000000000000000000 ) ) ;
#13023 = CARTESIAN_POINT ( 'NONE',  ( 2.592584512312225975, 0.9926283730735776523, 10.27797909968510126 ) ) ;
#13024 = CARTESIAN_POINT ( 'NONE',  ( 20.92250000136559507, 0.3178988483021036315, 3.024605502323848949 ) ) ;
#13025 = CARTESIAN_POINT ( 'NONE',  ( 15.99600675134221106, -15.99419002640760290, -1.499999999999999778 ) ) ;
#13026 = ADVANCED_FACE ( 'NONE', ( #2810 ), #13632, .F. ) ;
#13028 = ORIENTED_EDGE ( 'NONE', *, *, #30235, .F. ) ;
#13027 = LINE ( 'NONE', #11153, #29907 ) ;
#13029 = CARTESIAN_POINT ( 'NONE',  ( -7.662550801365593856, -0.3701630799359326152, 3.521866450007987037 ) ) ;
#13030 = DIRECTION ( 'NONE',  ( 0.000000000000000000, 0.9961946980917458783, -0.08715574274765383600 ) ) ;
#13032 = ADVANCED_FACE ( 'NONE', ( #31528 ), #13147, .T. ) ;
#13031 = CARTESIAN_POINT ( 'NONE',  ( -31.80940264096946635, 0.000000000000000000, 1.000000000000000000 ) ) ;
#13033 = ORIENTED_EDGE ( 'NONE', *, *, #32671, .T. ) ;
#13034 = ORIENTED_EDGE ( 'NONE', *, *, #13268, .T. ) ;
#13035 = EDGE_CURVE ( 'NONE', #3548, #280, #8245, .T. ) ;
#13036 = B_SPLINE_CURVE_WITH_KNOTS ( 'NONE', 3,
 ( #8392, #21118, #31316, #8541, #3222, #2928, #18588, #26291, #5729, #20941, #3402, #8248 ),
 .UNSPECIFIED., .F., .F.,
 ( 4, 2, 2, 2, 2, 4 ),
 ( 0.000000000000000000, 0.0002268479045755578691, 0.0004536958091511157382, 0.0005671197614388945102, 0.0006805437137266734989, 0.0009073916183022310428 ),
 .UNSPECIFIED. ) ;
#13037 = AXIS2_PLACEMENT_3D ( 'NONE', #17573, #27622, #29652 ) ;
#13038 = CARTESIAN_POINT ( 'NONE',  ( 24.35832023931450507, -17.33818253687174860, -1.317734466820339900 ) ) ;
#13039 = CARTESIAN_POINT ( 'NONE',  ( 3.063284526846072442, -8.461683424479964799, -2.223716399039827429 ) ) ;
#13040 = EDGE_CURVE ( 'NONE', #21301, #7656, #11455, .T. ) ;
#13041 = CARTESIAN_POINT ( 'NONE',  ( 23.23500000136559862, -3.156283516753370488, -0.9349337715887220401 ) ) ;
#13042 = CARTESIAN_POINT ( 'NONE',  ( 10.00000000000000000, 4.681538312723528605, -0.8254815157534769465 ) ) ;
#13043 = CARTESIAN_POINT ( 'NONE',  ( 5.377543748152549874, 2.741043480755029016, -7.530955069117485579 ) ) ;
#13044 = LOCAL_TIME ( 16, 7, 10.00000000000000000, #1077 ) ;
#13045 = DIRECTION ( 'NONE',  ( -0.000000000000000000, 0.000000000000000000, 1.000000000000000000 ) ) ;
#13046 = CARTESIAN_POINT ( 'NONE',  ( 35.27427105688962428, -8.145327135409177188, 1.529339875372225155 ) ) ;
#13047 = VERTEX_POINT ( 'NONE', #28546 ) ;
#13048 = DIRECTION ( 'NONE',  ( 0.000000000000000000, 0.000000000000000000, 1.000000000000000000 ) ) ;
#13049 = ADVANCED_FACE ( 'NONE', ( #5473 ), #3137, .F. ) ;
#13050 = PERSON_AND_ORGANIZATION_ROLE ( 'creator' ) ;
#13051 = CARTESIAN_POINT ( 'NONE',  ( 7.249760686538667009, -7.199384779417155045, 4.973063321323851760 ) ) ;
#13052 = ORIENTED_EDGE ( 'NONE', *, *, #16111, .T. ) ;
#13053 = ADVANCED_FACE ( 'NONE', ( #31715 ), #14432, .T. ) ;
#13054 = CIRCLE ( 'NONE', #29604, 0.9999999999999991118 ) ;
#13055 = DIRECTION ( 'NONE',  ( 1.000000000000000000, 0.000000000000000000, 0.000000000000000000 ) ) ;
#13056 = VERTEX_POINT ( 'NONE', #1439 ) ;
#13057 = CARTESIAN_POINT ( 'NONE',  ( -19.06947354093846059, 16.57130634721221440, 1.818690743637907836 ) ) ;
#13059 = ORIENTED_EDGE ( 'NONE', *, *, #23899, .T. ) ;
#13058 = CARTESIAN_POINT ( 'NONE',  ( 102.3749895180278884, -3.302517831782471269, -4.312042181581901445 ) ) ;
#13060 = ORIENTED_EDGE ( 'NONE', *, *, #30324, .F. ) ;
#13061 = DIRECTION ( 'NONE',  ( 0.000000000000000000, 0.000000000000000000, -1.000000000000000000 ) ) ;
#13062 = CARTESIAN_POINT ( 'NONE',  ( -6.112550801365593145, 1.088641768524161613, 3.675193018007246959 ) ) ;
#13063 = CARTESIAN_POINT ( 'NONE',  ( 9.836026323043101982, -12.51705112700722822, 1.500000000000000222 ) ) ;
#13064 = LINE ( 'NONE', #367, #32143 ) ;
#13066 = ORIENTED_EDGE ( 'NONE', *, *, #23946, .F. ) ;
#13065 = CARTESIAN_POINT ( 'NONE',  ( -47.55999999999999517, -10.96999999999998643, 5.700000000000000178 ) ) ;
#13067 = CARTESIAN_POINT ( 'NONE',  ( 14.23800746264082839, 22.11259878822725966, 1.508259000770582059 ) ) ;
#13068 = CARTESIAN_POINT ( 'NONE',  ( 23.59981322687704264, 18.33325850388178324, 1.500000000000000000 ) ) ;
#13069 = CARTESIAN_POINT ( 'NONE',  ( -2.574648304754633799, -12.71113778305264752, 1.500000000000000000 ) ) ;
#13071 = EDGE_CURVE ( 'NONE', #7539, #15957, #1330, .T. ) ;
#13070 = CARTESIAN_POINT ( 'NONE',  ( 23.17250000136559862, -2.363507492473152283, -1.913930629741525280 ) ) ;
#13072 = CARTESIAN_POINT ( 'NONE',  ( -42.46793790805479318, 24.51887538314362658, 1.500000000000000000 ) ) ;
#13074 = ORIENTED_EDGE ( 'NONE', *, *, #29017, .F. ) ;
#13073 = CARTESIAN_POINT ( 'NONE',  ( 108.0612411924935827, -18.95122005363461071, -4.517344619987845533 ) ) ;
#13075 = ADVANCED_FACE ( 'NONE', ( #3619 ), #28164, .T. ) ;
#13076 = CARTESIAN_POINT ( 'NONE',  ( 7.249760686538667009, 3.748318449932404484, -7.906491560603625679 ) ) ;
#13077 = CARTESIAN_POINT ( 'NONE',  ( -0.2059365608663963898, 0.5000000000000000000, 1.000000000000000000 ) ) ;
#13078 = CARTESIAN_POINT ( 'NONE',  ( 21.29750000136559507, -0.3178988483021076838, -3.024605502323848949 ) ) ;
#13079 = EDGE_CURVE ( 'NONE', #5270, #13793, #30168, .T. ) ;
#13080 = CARTESIAN_POINT ( 'NONE',  ( 1.147424988311415595, 0.5000000000000000000, -7.899334717979326292 ) ) ;
#13081 = DIRECTION ( 'NONE',  ( -1.000000000000000000, 0.000000000000000000, 0.000000000000000000 ) ) ;
#13082 = CARTESIAN_POINT ( 'NONE',  ( -3.226940125355887812, -1.840961572248389633E-05, -0.9957093966831331855 ) ) ;
#13083 = AXIS2_PLACEMENT_3D ( 'NONE', #14352, #9685, #14710 ) ;
#13084 = EDGE_LOOP ( 'NONE', ( #12710, #32350, #17522, #437, #17689, #3847 ) ) ;
#13085 = CARTESIAN_POINT ( 'NONE',  ( 4.749760686538667009, -2.741043480754977946, 7.530955069117504230 ) ) ;
#13086 = LINE ( 'NONE', #28471, #25254 ) ;
#13087 = ORIENTED_EDGE ( 'NONE', *, *, #2953, .T. ) ;
#13088 = EDGE_CURVE ( 'NONE', #24063, #19677, #12508, .T. ) ;
#13089 = DIRECTION ( 'NONE',  ( 0.000000000000000000, 0.000000000000000000, -1.000000000000000000 ) ) ;
#13090 = CARTESIAN_POINT ( 'NONE',  ( 84.62099044691944982, -6.357652361253733453, -2.184954680052196174 ) ) ;
#13091 = CARTESIAN_POINT ( 'NONE',  ( 0.5309851148689820333, -4.399114163800174282, -1.500000000000000444 ) ) ;
#13093 = CARTESIAN_POINT ( 'NONE',  ( 108.0130871940577748, -18.25781445536221526, 5.137726603835512940 ) ) ;
#13092 = CARTESIAN_POINT ( 'NONE',  ( 34.50075980479081039, -0.03048549489923639208, -2.568038078148737302 ) ) ;
#13094 = ORIENTED_EDGE ( 'NONE', *, *, #5006, .T. ) ;
#13095 = CARTESIAN_POINT ( 'NONE',  ( -40.70363404372887572, -12.74270274920393575, 5.547394276430027027 ) ) ;
#13096 = ORIENTED_EDGE ( 'NONE', *, *, #5441, .F. ) ;
#13097 = CARTESIAN_POINT ( 'NONE',  ( 107.5121035333901460, -18.26190534946589139, 5.137878862399732682 ) ) ;
#13099 = ORIENTED_EDGE ( 'NONE', *, *, #18600, .T. ) ;
#13098 = CARTESIAN_POINT ( 'NONE',  ( 10.56870887191539587, 4.787500056513365188, 1.476463073999653819 ) ) ;
#13100 = ORIENTED_EDGE ( 'NONE', *, *, #6525, .T. ) ;
#13101 = DIRECTION ( 'NONE',  ( 0.000000000000000000, 0.7071067811865495711, -0.7071067811865455743 ) ) ;
#13102 = CARTESIAN_POINT ( 'NONE',  ( 0.000000000000000000, -5.349675154362299345, -3.229702268444987645 ) ) ;
#13104 = ORIENTED_EDGE ( 'NONE', *, *, #10150, .T. ) ;
#13103 = CARTESIAN_POINT ( 'NONE',  ( 0.1962428234089072521, -6.885380501030516243, 1.500000000000000000 ) ) ;
#13105 = LINE ( 'NONE', #25596, #2828 ) ;
#13106 = CARTESIAN_POINT ( 'NONE',  ( -31.80959807272226669, -0.0003384977252881313063, 1.500000000000000000 ) ) ;
#13107 = CYLINDRICAL_SURFACE ( 'NONE', #633, 6.248999999999999666 ) ;
#13108 = EDGE_CURVE ( 'NONE', #7301, #14256, #29333, .T. ) ;
#13109 = DIRECTION ( 'NONE',  ( 0.000000000000000000, 0.000000000000000000, 1.000000000000000000 ) ) ;
#13110 = CARTESIAN_POINT ( 'NONE',  ( -50.60000000000000142, -0.5000000000000000000, 1.500000000000000000 ) ) ;
#13111 = SPHERICAL_SURFACE ( 'NONE', #18336, 0.4500000000000000111 ) ;
#13112 = DIRECTION ( 'NONE',  ( 0.000000000000000000, 0.4226182617406976094, -0.9063077870366508249 ) ) ;
#13113 = CARTESIAN_POINT ( 'NONE',  ( 1.998490341989216379, -1.623810759619012778, 1.499999999999999112 ) ) ;
#13114 = DIRECTION ( 'NONE',  ( 0.000000000000000000, -0.9063077870366448296, -0.4226182617407103770 ) ) ;
#13115 = CARTESIAN_POINT ( 'NONE',  ( 107.4500373638804120, -17.36019379023677089, -4.522129901861164036 ) ) ;
#13116 = CARTESIAN_POINT ( 'NONE',  ( 3.673334745432188075, 0.0007210401945645747868, 1.066984883846252341 ) ) ;
#13117 = DIRECTION ( 'NONE',  ( -0.000000000000000000, -0.3746065934159164001, 0.9271838545667856479 ) ) ;
#13118 = CARTESIAN_POINT ( 'NONE',  ( 102.7116376760607039, -2.711456868667909692, 5.695980980372492120 ) ) ;
#13119 = LINE ( 'NONE', #16102, #16175 ) ;
#13120 = ORIENTED_EDGE ( 'NONE', *, *, #917, .F. ) ;
#13121 = EDGE_CURVE ( 'NONE', #21706, #7070, #29183, .T. ) ;
#13122 = CARTESIAN_POINT ( 'NONE',  ( 25.38274187136685356, -2.592012193576345158, 0.5676849011231037689 ) ) ;
#13123 = DIRECTION ( 'NONE',  ( 1.000000000000000000, -8.574039729943018344E-17, -0.000000000000000000 ) ) ;
#13124 = ORIENTED_EDGE ( 'NONE', *, *, #27981, .F. ) ;
#13125 = CARTESIAN_POINT ( 'NONE',  ( 6.530491751506347420, -5.074604403564623389, -7.017944781892005324 ) ) ;
#13126 = ORIENTED_EDGE ( 'NONE', *, *, #27321, .F. ) ;
#13127 = CARTESIAN_POINT ( 'NONE',  ( 85.08949032934707191, -1.315411135598751668, -1.010822989962086416 ) ) ;
#13128 = CONTEXT_DEPENDENT_SHAPE_REPRESENTATION ( #3955, #30623 ) ;
#13130 = ORIENTED_EDGE ( 'NONE', *, *, #16167, .F. ) ;
#13129 = CARTESIAN_POINT ( 'NONE',  ( -4.365512850963738423, -6.230587388684557304, -1.499999999999999556 ) ) ;
#13131 = ORIENTED_EDGE ( 'NONE', *, *, #22622, .T. ) ;
#13132 = DIRECTION ( 'NONE',  ( 1.000000000000000000, -2.498001805406599692E-13, 0.000000000000000000 ) ) ;
#13133 = EDGE_CURVE ( 'NONE', #19939, #7714, #19316, .T. ) ;
#13134 = ORIENTED_EDGE ( 'NONE', *, *, #26052, .T. ) ;
#13135 = CARTESIAN_POINT ( 'NONE',  ( 21.23499999999999943, 0.2613211581691317065, 2.486304738420681559 ) ) ;
#13137 = ORIENTED_EDGE ( 'NONE', *, *, #24429, .T. ) ;
#13136 = LINE ( 'NONE', #28185, #1600 ) ;
#13138 = CARTESIAN_POINT ( 'NONE',  ( 18.51491971917342028, -8.599446730134175709, 1.010822989962089746 ) ) ;
#13139 = DIRECTION ( 'NONE',  ( -1.000000000000000000, 0.000000000000000000, -0.000000000000000000 ) ) ;
#13140 = ADVANCED_FACE ( 'NONE', ( #6425 ), #27155, .F. ) ;
#13141 = DIRECTION ( 'NONE',  ( 0.1437473352844943209, -6.136584296267958883E-14, -0.9896144216807913896 ) ) ;
#13142 = DIRECTION ( 'NONE',  ( 0.000000000000000000, 0.000000000000000000, -1.000000000000000000 ) ) ;
#13143 = VERTEX_POINT ( 'NONE', #22163 ) ;
#13144 = DIRECTION ( 'NONE',  ( -0.09975574163943222439, 0.1727820128662104771, -0.9798954883250904357 ) ) ;
#13145 = FACE_OUTER_BOUND ( 'NONE', #31697, .T. ) ;
#13146 = CARTESIAN_POINT ( 'NONE',  ( 69.12709522372691140, -7.241778149835380596, -2.184957268579761802 ) ) ;
#13147 = CYLINDRICAL_SURFACE ( 'NONE', #785, 11.00000000000000000 ) ;
#13148 = CARTESIAN_POINT ( 'NONE',  ( 23.09505357366878897, -21.93193652582860409, 1.086920924784747777 ) ) ;
#13149 = CARTESIAN_POINT ( 'NONE',  ( 0.000000000000000000, 0.005878491403456947983, 7.047692205288324629 ) ) ;
#13150 = LINE ( 'NONE', #10484, #138 ) ;
#13151 = DIRECTION ( 'NONE',  ( -1.000000000000000000, 0.000000000000000000, -0.000000000000000000 ) ) ;
#13152 = ORIENTED_EDGE ( 'NONE', *, *, #30275, .F. ) ;
#13153 = CARTESIAN_POINT ( 'NONE',  ( -3.212550801365593678, 1.828967928396027176, -3.368539882008727115 ) ) ;
#13154 = EDGE_LOOP ( 'NONE', ( #2185, #4222, #27605, #30121 ) ) ;
#13155 = CARTESIAN_POINT ( 'NONE',  ( -3.204531657079157547, -2.325406398514293205, 1.883076972206379818 ) ) ;
#13156 = CARTESIAN_POINT ( 'NONE',  ( 108.0732232521118590, 18.58589588515538082, 4.641033904584911163 ) ) ;
#13157 = CARTESIAN_POINT ( 'NONE',  ( -12.44989959798873791, 0.000000000000000000, -12.99999999999999645 ) ) ;
#13158 = CARTESIAN_POINT ( 'NONE',  ( 10.63777812034810566, -12.44241537516270490, 1.000000000000000000 ) ) ;
#13159 = VERTEX_POINT ( 'NONE', #6614 ) ;
#13160 = CARTESIAN_POINT ( 'NONE',  ( 18.89400067069844624, -4.362082497106836598, -3.390608483633292813 ) ) ;
#13161 = PERSON ( 'NAUO-PER3', 'UNSPECIFIED', 'UNSPECIFIED', ('UNSPECIFIED'), ('UNSPECIFIED'), ('UNSPECIFIED') ) ;
#13162 = EDGE_LOOP ( 'NONE', ( #26009, #5816, #10532, #11931, #1937 ) ) ;
#13163 = CYLINDRICAL_SURFACE ( 'NONE', #23037, 8.749000000000002331 ) ;
#13164 = CALENDAR_DATE ( 2026, 6, 10 ) ;
#13165 = CARTESIAN_POINT ( 'NONE',  ( 28.66518199730131755, -6.722860712036216491, 4.053847714221102905 ) ) ;
#13166 = EDGE_CURVE ( 'NONE', #25302, #10864, #21812, .T. ) ;
#13167 = ADVANCED_FACE ( 'NONE', ( #16626 ), #29689, .F. ) ;
#13168 = CARTESIAN_POINT ( 'NONE',  ( 9.282537329959909655, 0.2172754300399127037, 1.041239158277186938 ) ) ;
#13170 = CARTESIAN_POINT ( 'NONE',  ( 3.499999999999999556, 1.459547570502368385, 6.894905428400277536 ) ) ;
#13169 = CARTESIAN_POINT ( 'NONE',  ( 42.35322304605574573, -22.56891886512037360, 4.522129901861158707 ) ) ;
#13171 = ORIENTED_EDGE ( 'NONE', *, *, #14208, .F. ) ;
#13172 = DIRECTION ( 'NONE',  ( 0.000000000000000000, 0.8660254037844361541, 0.5000000000000041078 ) ) ;
#13173 = DIRECTION ( 'NONE',  ( 0.000000000000000000, 0.000000000000000000, -1.000000000000000000 ) ) ;
#13174 = CARTESIAN_POINT ( 'NONE',  ( 22.29750000136559507, -2.363507492473152283, -1.913930629741525280 ) ) ;
#13176 = ORIENTED_EDGE ( 'NONE', *, *, #19820, .T. ) ;
#13175 = CARTESIAN_POINT ( 'NONE',  ( 9.286001645569189833, 0.2223290027121335721, -1.044355983488527873 ) ) ;
#13177 = CARTESIAN_POINT ( 'NONE',  ( -6.612550801365593145, -3.368539882008727115, -1.828967928396028064 ) ) ;
#13178 = CARTESIAN_POINT ( 'NONE',  ( 10.57125986779756843, -4.681538312723512618, -0.8254815157535732029 ) ) ;
#13179 = CARTESIAN_POINT ( 'NONE',  ( 102.4497391607709886, -4.374320780254121743, -3.390608474985632448 ) ) ;
#13180 = ORIENTED_EDGE ( 'NONE', *, *, #6, .F. ) ;
#13181 = ORIENTED_EDGE ( 'NONE', *, *, #29229, .F. ) ;
#13182 = CARTESIAN_POINT ( 'NONE',  ( 108.5690947754410018, 15.68962964501444546, -1.099690591032340459 ) ) ;
#13183 = CARTESIAN_POINT ( 'NONE',  ( 108.1296380701673598, -19.93611807713457651, 1.386936492588066949 ) ) ;
#13184 = CARTESIAN_POINT ( 'NONE',  ( 23.79750000136559507, 2.363507492473148286, 1.913930629741525058 ) ) ;
#13185 = FACE_OUTER_BOUND ( 'NONE', #22100, .T. ) ;
#13186 = CARTESIAN_POINT ( 'NONE',  ( 10.00000000000000178, -8.574039729943018837E-16, 0.000000000000000000 ) ) ;
#13187 = DIRECTION ( 'NONE',  ( 0.000000000000000000, 0.000000000000000000, 1.000000000000000000 ) ) ;
#13188 = DIRECTION ( 'NONE',  ( -0.000000000000000000, -0.5735764363510502672, 0.8191520442889888010 ) ) ;
#13189 = ORIENTED_EDGE ( 'NONE', *, *, #1663, .T. ) ;
#13190 = DIRECTION ( 'NONE',  ( -1.000000000000000000, 0.000000000000000000, 0.000000000000000000 ) ) ;
#13191 = EDGE_CURVE ( 'NONE', #8159, #19057, #4526, .T. ) ;
#13192 = ORIENTED_EDGE ( 'NONE', *, *, #22289, .F. ) ;
#13193 = DATE_AND_TIME ( #26429, #15676 ) ;
#13194 = CARTESIAN_POINT ( 'NONE',  ( -31.80940264096946635, 0.000000000000000000, 1.000000000000000000 ) ) ;
#13195 = EDGE_LOOP ( 'NONE', ( #29088, #30425, #6717, #22858, #25962, #12925, #2287 ) ) ;
#13196 = LINE ( 'NONE', #31285, #5570 ) ;
#13197 = VERTEX_POINT ( 'NONE', #26838 ) ;
#13198 = CARTESIAN_POINT ( 'NONE',  ( -16.91521474802581437, 10.78976942541848594, 1.963924860182840515 ) ) ;
#13200 = ORIENTED_EDGE ( 'NONE', *, *, #10378, .F. ) ;
#13199 = CARTESIAN_POINT ( 'NONE',  ( 40.87951250946358783, -6.073635182903602825, -4.275175681028137831 ) ) ;
#13201 = EDGE_CURVE ( 'NONE', #24044, #508, #16310, .T. ) ;
#13202 = EDGE_LOOP ( 'NONE', ( #1545, #21013, #28681, #27582 ) ) ;
#13203 = CARTESIAN_POINT ( 'NONE',  ( -0.7739934281325309140, -8.972773999336983053, -4.522129901861164925 ) ) ;
#13204 = CARTESIAN_POINT ( 'NONE',  ( -7.712550801365593678, 1.088641768524161613, 3.675193018007246959 ) ) ;
#13205 = FACE_OUTER_BOUND ( 'NONE', #2255, .T. ) ;
#13206 = CARTESIAN_POINT ( 'NONE',  ( 18.53796472816966556, -8.341849780241110679, -1.915219082070897638 ) ) ;
#13208 = ORIENTED_EDGE ( 'NONE', *, *, #16494, .F. ) ;
#13207 = CARTESIAN_POINT ( 'NONE',  ( 10.00000000000000178, -4.208382051008173086, -2.718385644597221873 ) ) ;
#13209 = LINE ( 'NONE', #13362, #31126 ) ;
#13210 = CARTESIAN_POINT ( 'NONE',  ( 40.74410603220348293, -8.021703207543309233, 2.184955501613824236 ) ) ;
#13211 =( BOUNDED_SURFACE ( )  B_SPLINE_SURFACE ( 1, 3, ( 
 ( #29687, #19649, #22811, #25644 ),
 ( #4759, #15117, #5104, #22477 ) ),
 .UNSPECIFIED., .F., .F., .F. ) 
 B_SPLINE_SURFACE_WITH_KNOTS ( ( 2, 2 ),
 ( 4, 4 ),
 ( 0.000000000000000000, 1.000000000000000000 ),
 ( 0.000000000000000000, 1.000000000000000000 ),
 .UNSPECIFIED. ) 
 GEOMETRIC_REPRESENTATION_ITEM ( )  RATIONAL_B_SPLINE_SURFACE ( (
 ( 1.000000000000000000, 0.9917560313531952332, 0.9917560313531952332, 1.000000000000000000),
 ( 1.000000000000000000, 0.9917560313531952332, 0.9917560313531952332, 1.000000000000000000) ) ) 
 REPRESENTATION_ITEM ( '' )  SURFACE ( )  );
#13212 = EDGE_CURVE ( 'NONE', #11449, #30719, #1099, .T. ) ;
#13213 = CARTESIAN_POINT ( 'NONE',  ( -4.224498304150544392, -5.428959277710454501, 1.500000000000239808 ) ) ;
#13214 = CARTESIAN_POINT ( 'NONE',  ( 21.23500000136559507, -1.570731468192933633, -2.892927487894330074 ) ) ;
#13215 = CARTESIAN_POINT ( 'NONE',  ( 2.808958353948056264, -0.3589573147998340596, 1.483919649041820499 ) ) ;
#13217 = ORIENTED_EDGE ( 'NONE', *, *, #7722, .F. ) ;
#13216 = CARTESIAN_POINT ( 'NONE',  ( 4.075891499408641642E-16, 4.753758587302147731, 0.000000000000000000 ) ) ;
#13218 = CARTESIAN_POINT ( 'NONE',  ( 8.870145747188287189, 0.000000000000000000, 4.148259000770580407 ) ) ;
#13219 = B_SPLINE_CURVE_WITH_KNOTS ( 'NONE', 3,
 ( #1391, #18946, #13885, #11077, #29136, #29460 ),
 .UNSPECIFIED., .F., .F.,
 ( 4, 2, 4 ),
 ( 0.01682075285868000689, 0.5000000000000000000, 0.5131349204668804731 ),
 .UNSPECIFIED. ) ;
#13220 = CARTESIAN_POINT ( 'NONE',  ( -29.98627798296288915, 13.02091040240743602, 1.906846592315978528 ) ) ;
#13221 = CARTESIAN_POINT ( 'NONE',  ( 25.42250000273118360, 1.291182301015469047, 2.378061970571981654 ) ) ;
#13222 = ADVANCED_FACE ( 'NONE', ( #11296 ), #6271, .T. ) ;
#13223 = CARTESIAN_POINT ( 'NONE',  ( -3.122314033877883927E-16, -3.641590349731949505, 3.055657119358789142 ) ) ;
#13224 = CARTESIAN_POINT ( 'NONE',  ( 101.8278197859226708, -4.419131406518054916, -3.387719699150975927 ) ) ;
#13225 = CYLINDRICAL_SURFACE ( 'NONE', #16154, 3.000000000000000444 ) ;
#13226 = ORIENTED_EDGE ( 'NONE', *, *, #8134, .F. ) ;
#13227 = CARTESIAN_POINT ( 'NONE',  ( 107.9802527803230419, -17.78500706576073753, 4.325704939602341703 ) ) ;
#13228 = EDGE_CURVE ( 'NONE', #866, #7332, #2381, .T. ) ;
#13229 = LINE ( 'NONE', #17941, #18838 ) ;
#13230 = ORIENTED_EDGE ( 'NONE', *, *, #28690, .F. ) ;
#13231 = DIRECTION ( 'NONE',  ( 0.000000000000000000, 0.000000000000000000, -1.000000000000000000 ) ) ;
#13232 = DIRECTION ( 'NONE',  ( 0.000000000000000000, 0.7431448254773954654, -0.6691306063588569053 ) ) ;
#13233 = EDGE_CURVE ( 'NONE', #6857, #31196, #24794, .T. ) ;
#13234 = CARTESIAN_POINT ( 'NONE',  ( 0.8407900506754626413, -11.56055812333295130, -4.522129901861164925 ) ) ;
#13236 = CARTESIAN_POINT ( 'NONE',  ( 107.9811281649432289, -17.79761238652359978, 4.359937231691887405 ) ) ;
#13235 = CARTESIAN_POINT ( 'NONE',  ( 69.42401195566040428, -8.835509274236315491, -0.07017451552783579571 ) ) ;
#13237 = ADVANCED_FACE ( 'NONE', ( #30347 ), #30322, .F. ) ;
#13238 = EDGE_LOOP ( 'NONE', ( #16469, #14259, #24681, #25429 ) ) ;
#13239 = LINE ( 'NONE', #21428, #29403 ) ;
#13240 = VERTEX_POINT ( 'NONE', #2594 ) ;
#13241 = CARTESIAN_POINT ( 'NONE',  ( -3.105859910356985054, -0.009789559233381405975, 1.118159719381635497 ) ) ;
#13243 = ORIENTED_EDGE ( 'NONE', *, *, #20269, .F. ) ;
#13242 = CARTESIAN_POINT ( 'NONE',  ( 3.249999999999999556, 9.314797388894893615, 5.239665997526921082 ) ) ;
#13244 = ORIENTED_EDGE ( 'NONE', *, *, #3809, .F. ) ;
#13245 = CARTESIAN_POINT ( 'NONE',  ( 25.75999999999999801, -1.902510934646483477E-15, 2.499999999999997780 ) ) ;
#13246 = LINE ( 'NONE', #12923, #31074 ) ;
#13248 = ORIENTED_EDGE ( 'NONE', *, *, #25009, .T. ) ;
#13247 = CARTESIAN_POINT ( 'NONE',  ( 17.32050807568873552, 10.00000000000002309, -1.491740999229418829 ) ) ;
#13249 = ORIENTED_EDGE ( 'NONE', *, *, #13233, .T. ) ;
#13250 = CARTESIAN_POINT ( 'NONE',  ( 10.00000000000000178, -8.574039729943018837E-16, 0.000000000000000000 ) ) ;
#13251 = CARTESIAN_POINT ( 'NONE',  ( 18.70833836802739469, -6.437414421208801585, 3.093520103104856034 ) ) ;
#13252 = DIRECTION ( 'NONE',  ( -1.000000000000000000, -0.000000000000000000, -0.000000000000000000 ) ) ;
#13253 = LINE ( 'NONE', #28798, #13884 ) ;
#13254 = CARTESIAN_POINT ( 'NONE',  ( 101.6058569626687245, -1.222921969063083258, 0.8134928172057650508 ) ) ;
#13255 = ADVANCED_FACE ( 'NONE', ( #30516 ), #30018, .T. ) ;
#13256 = CARTESIAN_POINT ( 'NONE',  ( 4.290242492657217039E-16, 5.003758587302148619, 0.2500000000000008882 ) ) ;
#13257 = CARTESIAN_POINT ( 'NONE',  ( 3.326374039432143270, -11.41640325077553975, 1.499999999999999778 ) ) ;
#13258 = FACE_BOUND ( 'NONE', #29786, .T. ) ;
#13259 = DIRECTION ( 'NONE',  ( -1.000000000000000000, 0.000000000000000000, 0.000000000000000000 ) ) ;
#13260 = CARTESIAN_POINT ( 'NONE',  ( 10.00000000000000178, 4.458382051008225488, -2.285372942704905430 ) ) ;
#13261 = ORIENTED_EDGE ( 'NONE', *, *, #18046, .T. ) ;
#13262 = DIRECTION ( 'NONE',  ( 0.000000000000000000, 0.000000000000000000, 1.000000000000000000 ) ) ;
#13263 = CARTESIAN_POINT ( 'NONE',  ( 48.02957825751263243, -5.434743900606504141, 5.695980980372492120 ) ) ;
#13264 = EDGE_CURVE ( 'NONE', #979, #32109, #32557, .T. ) ;
#13265 = CARTESIAN_POINT ( 'NONE',  ( 7.249760686538667009, -8.014274990069656823, 8.669741416787380218E-17 ) ) ;
#13266 = ORIENTED_EDGE ( 'NONE', *, *, #17256, .F. ) ;
#13267 = CARTESIAN_POINT ( 'NONE',  ( 22.92250000136559862, 0.3178988483021036315, 3.024605502323848949 ) ) ;
#13268 = EDGE_CURVE ( 'NONE', #3200, #8276, #6922, .T. ) ;
#13269 = CARTESIAN_POINT ( 'NONE',  ( 0.6708088701982989344, 0.000000000000000000, -4.612695725900422872 ) ) ;
#13270 = ORIENTED_EDGE ( 'NONE', *, *, #28255, .T. ) ;
#13271 = CARTESIAN_POINT ( 'NONE',  ( 18.79913864311901861, -5.422449579812291809, -4.312036717478699543 ) ) ;
#13272 = EDGE_CURVE ( 'NONE', #31785, #7245, #4449, .T. ) ;
#13273 = ORIENTED_EDGE ( 'NONE', *, *, #2224, .T. ) ;
#13274 = CARTESIAN_POINT ( 'NONE',  ( 32.37020706055088937, 18.00000000000000355, 0.3702070605511125212 ) ) ;
#13275 = DATE_AND_TIME ( #15805, #31743 ) ;
#13277 = VERTEX_POINT ( 'NONE', #19808 ) ;
#13276 = CARTESIAN_POINT ( 'NONE',  ( 101.6441386174529384, -1.774168274679073454, -2.184956718804114573 ) ) ;
#13278 = ORIENTED_EDGE ( 'NONE', *, *, #26605, .F. ) ;
#13279 = CYLINDRICAL_SURFACE ( 'NONE', #2778, 0.4499999999999996225 ) ;
#13280 = ORIENTED_EDGE ( 'NONE', *, *, #25627, .T. ) ;
#13281 = DIRECTION ( 'NONE',  ( 7.472768010112066903E-18, 0.08715574274766894891, -0.9961946980917446570 ) ) ;
#13283 = ORIENTED_EDGE ( 'NONE', *, *, #23114, .T. ) ;
#13282 = CARTESIAN_POINT ( 'NONE',  ( 68.92628806523701712, -3.240579989648070036, -0.07017451552797518421 ) ) ;
#13284 = CARTESIAN_POINT ( 'NONE',  ( 69.38611993481310947, -8.080330187051606217, 2.713652344655544724 ) ) ;
#13285 = CARTESIAN_POINT ( 'NONE',  ( -42.46793790805478608, 24.51887538314362658, -1.500000000000000000 ) ) ;
#13286 = CYLINDRICAL_SURFACE ( 'NONE', #17837, 2.999999999999999112 ) ;
#13287 = DIRECTION ( 'NONE',  ( 0.7222222222222220989, 0.000000000000000000, -0.6916610887771519334 ) ) ;
#13288 = ADVANCED_FACE ( 'NONE', ( #14780 ), #4605, .F. ) ;
#13289 = ORIENTED_EDGE ( 'NONE', *, *, #11405, .F. ) ;
#13290 = APPROVAL ( #23854, 'UNSPECIFIED' ) ;
#13291 = CARTESIAN_POINT ( 'NONE',  ( -4.106376978575948300, -0.1572233378491262878, 2.999999999999999556 ) ) ;
#13292 = CARTESIAN_POINT ( 'NONE',  ( 0.9232102171129937807, 0.000000000000000000, -4.522129901861164925 ) ) ;
#13293 = CARTESIAN_POINT ( 'NONE',  ( 85.10567447696169552, -6.328783234401409885, -2.184955974440073501 ) ) ;
#13294 = CARTESIAN_POINT ( 'NONE',  ( 0.000000000000000000, 2.871924938129968741, -6.435996203144479288 ) ) ;
#13295 = PLANE ( 'NONE',  #28425 ) ;
#13296 = CARTESIAN_POINT ( 'NONE',  ( 0.000000000000000000, 7.008469740302802897, 0.7425307242148009301 ) ) ;
#13297 = CARTESIAN_POINT ( 'NONE',  ( 22.98500000273118715, -0.2613211581691358698, -2.486304738420681559 ) ) ;
#13298 = CARTESIAN_POINT ( 'NONE',  ( 21.65220420020007097, -21.84595744892845559, 1.292937544721791898 ) ) ;
#13299 = CARTESIAN_POINT ( 'NONE',  ( -7.550050802731187893, 2.983565686104819648, 0.3135853898029609677 ) ) ;
#13300 = ORIENTED_EDGE ( 'NONE', *, *, #10921, .T. ) ;
#13301 = ADVANCED_FACE ( 'NONE', ( #12940 ), #18465, .T. ) ;
#13302 = CARTESIAN_POINT ( 'NONE',  ( -3.154531657079157281, -3.105402419394638791, 0.9198621039125867149 ) ) ;
#13303 = CIRCLE ( 'NONE', #32010, 6.000000000000000000 ) ;
#13304 = FACE_OUTER_BOUND ( 'NONE', #10334, .T. ) ;
#13305 = CARTESIAN_POINT ( 'NONE',  ( -5.306376978575950254, 0.1572233378491222633, -3.000000000000000000 ) ) ;
#13306 = CARTESIAN_POINT ( 'NONE',  ( 11.72844749915270413, -13.05523934215238313, 1.500000000000280220 ) ) ;
#13307 = EDGE_LOOP ( 'NONE', ( #2640, #21163, #26723, #2393 ) ) ;
#13308 = CARTESIAN_POINT ( 'NONE',  ( 3.499999999999999556, 7.008469740302810891, -0.7425307242147067832 ) ) ;
#13309 = AXIS2_PLACEMENT_3D ( 'NONE', #19602, #29963, #6726 ) ;
#13310 = ORIENTED_EDGE ( 'NONE', *, *, #26025, .F. ) ;
#13311 = CARTESIAN_POINT ( 'NONE',  ( 0.7212197813471248331, 8.337493976377276184, 3.259817272365101104 ) ) ;
#13312 = PERSON_AND_ORGANIZATION ( #6766, #25292 ) ;
#13313 = CARTESIAN_POINT ( 'NONE',  ( 102.4180935425471972, -3.924747953286301438, 4.093303780333640951 ) ) ;
#13314 = LINE ( 'NONE', #18522, #23522 ) ;
#13315 = ORIENTED_EDGE ( 'NONE', *, *, #6890, .F. ) ;
#13316 = DIRECTION ( 'NONE',  ( 1.000000000000000000, -0.000000000000000000, 0.000000000000000000 ) ) ;
#13317 = ADVANCED_FACE ( 'NONE', ( #13258, #80 ), #10273, .T. ) ;
#13318 = DIRECTION ( 'NONE',  ( -1.000000000000000000, 0.000000000000000000, -0.000000000000000000 ) ) ;
#13319 = CARTESIAN_POINT ( 'NONE',  ( 9.295344188488364523, -0.03282880342717511835, 1.183647805826461674 ) ) ;
#13320 = CIRCLE ( 'NONE', #5861, 10.94895958125474245 ) ;
#13322 = EDGE_LOOP ( 'NONE', ( #19120, #26347 ) ) ;
#13321 = CARTESIAN_POINT ( 'NONE',  ( 0.4474568012433104425, -7.410208993127077370, 0.9788672205888330202 ) ) ;
#13323 = CARTESIAN_POINT ( 'NONE',  ( -4.062550801365593323, 0.3701630799359330593, -3.521866450007987037 ) ) ;
#13324 = AXIS2_PLACEMENT_3D ( 'NONE', #9266, #19488, #29680 ) ;
#13325 = CARTESIAN_POINT ( 'NONE',  ( -10.00000000000000000, 0.000000000000000000, 0.000000000000000000 ) ) ;
#13326 = DIRECTION ( 'NONE',  ( -0.000000000000000000, -0.9063077870366526012, 0.4226182617406936126 ) ) ;
#13327 = ORIENTED_EDGE ( 'NONE', *, *, #20135, .F. ) ;
#13328 = ORIENTED_EDGE ( 'NONE', *, *, #22489, .F. ) ;
#13329 = AXIS2_PLACEMENT_3D ( 'NONE', #29964, #22428, #32981 ) ;
#13330 = DIRECTION ( 'NONE',  ( -0.000000000000000000, 0.7071067811865466846, -0.7071067811865483499 ) ) ;
#13331 = DIRECTION ( 'NONE',  ( -0.000000000000000000, -0.000000000000000000, -1.000000000000000000 ) ) ;
#13332 = EDGE_CURVE ( 'NONE', #26019, #5620, #20974, .T. ) ;
#13333 = LINE ( 'NONE', #18393, #10287 ) ;
#13334 = EDGE_CURVE ( 'NONE', #9983, #27584, #31340, .T. ) ;
#13335 = CARTESIAN_POINT ( 'NONE',  ( 0.3076688774149766159, 2.239519426675734337, 10.04057401064416233 ) ) ;
#13336 = DIRECTION ( 'NONE',  ( 0.000000000000000000, 0.000000000000000000, 1.000000000000000000 ) ) ;
#13337 = EDGE_CURVE ( 'NONE', #18655, #5149, #273, .T. ) ;
#13338 = VECTOR ( 'NONE', #1659, 1000.000000000000000 ) ;
#13339 = CARTESIAN_POINT ( 'NONE',  ( 2.808958353948056708, -0.3589573147998343372, -1.483919649041820721 ) ) ;
#13340 = CARTESIAN_POINT ( 'NONE',  ( 41.35712849199997976, -8.497574858407940468, 0.07017451552782413837 ) ) ;
#13341 = VERTEX_POINT ( 'NONE', #23633 ) ;
#13342 = FACE_OUTER_BOUND ( 'NONE', #14021, .T. ) ;
#13343 = AXIS2_PLACEMENT_3D ( 'NONE', #24547, #1859, #32099 ) ;
#13344 = AXIS2_PLACEMENT_3D ( 'NONE', #30340, #27810, #15605 ) ;
#13345 = ORIENTED_EDGE ( 'NONE', *, *, #12169, .T. ) ;
#13346 = DATE_AND_TIME ( #21079, #8208 ) ;
#13347 = DIRECTION ( 'NONE',  ( 0.000000000000000000, 0.000000000000000000, -1.000000000000000000 ) ) ;
#13348 = ORIENTED_EDGE ( 'NONE', *, *, #526, .F. ) ;
#13349 = AXIS2_PLACEMENT_3D ( 'NONE', #26184, #21322, #2991 ) ;
#13350 = DIRECTION ( 'NONE',  ( -0.1027947991993877902, 0.9947025833170222153, 0.000000000000000000 ) ) ;
#13351 = ORIENTED_EDGE ( 'NONE', *, *, #18557, .F. ) ;
#13352 = LINE ( 'NONE', #10877, #3888 ) ;
#13354 = VERTEX_POINT ( 'NONE', #5426 ) ;
#13353 = CARTESIAN_POINT ( 'NONE',  ( 102.3504764446131645, -2.948660565431382885, -4.112224487563005404 ) ) ;
#13355 = ORIENTED_EDGE ( 'NONE', *, *, #4938, .F. ) ;
#13356 = DIRECTION ( 'NONE',  ( 0.000000000000000000, -0.9961946980917445460, -0.08715574274766962892 ) ) ;
#13357 = CARTESIAN_POINT ( 'NONE',  ( -3.412550801365592967, -3.368539882008727115, -1.828967928396027842 ) ) ;
#13358 = CARTESIAN_POINT ( 'NONE',  ( 7.565496255526879210, -10.23852490753181499, 1.500000000000000222 ) ) ;
#13359 = CARTESIAN_POINT ( 'NONE',  ( 0.000000000000000000, 7.003298780661427969, 4.817032923780590892 ) ) ;
#13361 = ORIENTED_EDGE ( 'NONE', *, *, #20031, .T. ) ;
#13360 = CARTESIAN_POINT ( 'NONE',  ( -29.24402871571405882, -27.93932300454937590, 11.00000000000000000 ) ) ;
#13362 = CARTESIAN_POINT ( 'NONE',  ( -41.86373177837819526, -16.13513036599590222, 5.128141679950118714 ) ) ;
#13363 = CARTESIAN_POINT ( 'NONE',  ( 16.54275606305774460, 11.79585867046270486, 1.050000000000000044 ) ) ;
#13364 = CARTESIAN_POINT ( 'NONE',  ( 6.212730774181275173, -18.25773092725300728, 1.748739615172814732 ) ) ;
#13365 = CARTESIAN_POINT ( 'NONE',  ( 17.33093461831547444, -21.43932300456618378, -1.500000000000000000 ) ) ;
#13366 = DIRECTION ( 'NONE',  ( 0.000000000000000000, 0.000000000000000000, -1.000000000000000000 ) ) ;
#13368 = VERTEX_POINT ( 'NONE', #5262 ) ;
#13367 = DIRECTION ( 'NONE',  ( 0.000000000000000000, -0.9271838545667856479, -0.3746065934159162891 ) ) ;
#13369 = DIRECTION ( 'NONE',  ( 0.000000000000000000, -1.865174681370262988E-14, 1.000000000000000000 ) ) ;
#13370 = AXIS2_PLACEMENT_3D ( 'NONE', #12135, #24491, #22008 ) ;
#13371 = EDGE_CURVE ( 'NONE', #3931, #8864, #10443, .T. ) ;
#13372 = DIRECTION ( 'NONE',  ( 0.000000000000000000, 0.000000000000000000, 1.000000000000000000 ) ) ;
#13373 = CARTESIAN_POINT ( 'NONE',  ( 20.92250000136559507, -1.913930629741527500, 2.363507492473149618 ) ) ;
#13374 = CARTESIAN_POINT ( 'NONE',  ( -19.95676506897142843, 4.491141813158487928, 1.500000000000000000 ) ) ;
#13375 = CARTESIAN_POINT ( 'NONE',  ( 102.9361373302715918, -5.944196040818415128, -2.713652344655542947 ) ) ;
#13376 = CARTESIAN_POINT ( 'NONE',  ( 10.55147673363119232, 4.458382051008223712, -2.285372942704906762 ) ) ;
#13377 = CARTESIAN_POINT ( 'NONE',  ( 10.00000000000000178, -8.574039729943018837E-16, 0.000000000000000000 ) ) ;
#13378 = FACE_OUTER_BOUND ( 'NONE', #4509, .T. ) ;
#13379 = ORIENTED_EDGE ( 'NONE', *, *, #15336, .T. ) ;
#13380 = CARTESIAN_POINT ( 'NONE',  ( 10.00000000000000000, 4.753758587302147731, 2.969445807578340325E-16 ) ) ;
#13381 = CIRCLE ( 'NONE', #14985, 0.4999999999999996669 ) ;
#13382 = DIRECTION ( 'NONE',  ( 0.9896144216807900573, -0.000000000000000000, 0.1437473352845036745 ) ) ;
#13383 = CIRCLE ( 'NONE', #6978, 299.4192503346018270 ) ;
#13384 = CARTESIAN_POINT ( 'NONE',  ( 3.020080181661099594, 8.342499971033895179, -3.262125172873930001 ) ) ;
#13386 = CARTESIAN_POINT ( 'NONE',  ( 108.0347112123201612, -18.56919493900439377, 5.017201665671134236 ) ) ;
#13385 = CYLINDRICAL_SURFACE ( 'NONE', #5947, 5.010000000000000675 ) ;
#13387 = ORIENTED_EDGE ( 'NONE', *, *, #29412, .T. ) ;
#13388 = AXIS2_PLACEMENT_3D ( 'NONE', #11878, #14708, #4356 ) ;
#13389 = VECTOR ( 'NONE', #23055, 1000.000000000000000 ) ;
#13390 = CARTESIAN_POINT ( 'NONE',  ( 2.274274201625327230, 0.000000000000000000, 0.000000000000000000 ) ) ;
#13391 = VERTEX_POINT ( 'NONE', #30706 ) ;
#13392 =( BOUNDED_CURVE ( )  B_SPLINE_CURVE ( 3, ( #13585, #903, #31820, #11081 ),
 .UNSPECIFIED., .F., .F. ) 
 B_SPLINE_CURVE_WITH_KNOTS ( ( 4, 4 ),
 ( 3.901433257974888047, 5.290220370840431841 ),
 .UNSPECIFIED. ) 
 CURVE ( )  GEOMETRIC_REPRESENTATION_ITEM ( )  RATIONAL_B_SPLINE_CURVE ( ( 1.000000000000000000, 0.8456279454424026065, 0.8456279454424026065, 1.000000000000000000 ) ) 
 REPRESENTATION_ITEM ( '' )  );
#13393 = CARTESIAN_POINT ( 'NONE',  ( 21.34939358370785101, -21.78237682584212465, -1.377397332511757444 ) ) ;
#13395 = ORIENTED_EDGE ( 'NONE', *, *, #28198, .F. ) ;
#13394 = DIRECTION ( 'NONE',  ( 1.000000000000000000, -8.574039729943018344E-17, -0.000000000000000000 ) ) ;
#13396 = B_SPLINE_CURVE_WITH_KNOTS ( 'NONE', 3,
 ( #5435, #576, #33023, #18304, #20980, #26152, #10766, #15442 ),
 .UNSPECIFIED., .F., .F.,
 ( 4, 2, 2, 4 ),
 ( 0.000000000000000000, 0.5000000000000000000, 0.7500000000000000000, 1.000000000000000000 ),
 .UNSPECIFIED. ) ;
#13397 = ORIENTED_EDGE ( 'NONE', *, *, #32526, .F. ) ;
#13398 = CARTESIAN_POINT ( 'NONE',  ( 84.48140976240925681, -4.087790770811431607, 3.993432235017919218 ) ) ;
#13399 = EDGE_CURVE ( 'NONE', #29918, #5334, #25646, .T. ) ;
#13400 = FACE_OUTER_BOUND ( 'NONE', #3422, .T. ) ;
#13402 = VERTEX_POINT ( 'NONE', #8419 ) ;
#13401 = CARTESIAN_POINT ( 'NONE',  ( 6.356382399260309235, -3.797266095948536258, 7.723816458760333958 ) ) ;
#13403 = ORIENTED_EDGE ( 'NONE', *, *, #6327, .F. ) ;
#13404 = CARTESIAN_POINT ( 'NONE',  ( 10.46141283585619242, -19.61934161334578519, -1.750340053724213973 ) ) ;
#13405 = EDGE_CURVE ( 'NONE', #13354, #13368, #2761, .T. ) ;
#13406 = CARTESIAN_POINT ( 'NONE',  ( 21.99035326630345466, -21.86692099231494879, -1.263015267642259243 ) ) ;
#13407 = CARTESIAN_POINT ( 'NONE',  ( 0.000000000000000000, 0.000000000000000000, 0.000000000000000000 ) ) ;
#13408 = CARTESIAN_POINT ( 'NONE',  ( 10.00000000000000000, 4.116875700062082366, 2.376879293651078751 ) ) ;
#13409 = CARTESIAN_POINT ( 'NONE',  ( 2.857987970437214198, 3.588272043371452114, 8.861329655870052946 ) ) ;
#13410 = CIRCLE ( 'NONE', #26792, 3.024999999999999911 ) ;
#13411 = DIRECTION ( 'NONE',  ( 1.000000000000000000, -0.000000000000000000, -0.000000000000000000 ) ) ;
#13412 = CARTESIAN_POINT ( 'NONE',  ( 0.5441968595407785658, -6.194664530687079562, 1.500000000000000666 ) ) ;
#13413 = CARTESIAN_POINT ( 'NONE',  ( 17.32050807568873552, 10.00000000000002309, 1.500000000000000000 ) ) ;
#13414 = EDGE_CURVE ( 'NONE', #5412, #15980, #30859, .T. ) ;
#13415 = ADVANCED_FACE ( 'NONE', ( #3252 ), #653, .F. ) ;
#13416 = VECTOR ( 'NONE', #14819, 1000.000000000000000 ) ;
#13417 = AXIS2_PLACEMENT_3D ( 'NONE', #18295, #31006, #30705 ) ;
#13418 = CARTESIAN_POINT ( 'NONE',  ( -4.365512850963738423, -6.230587388684557304, 1.500000000000000000 ) ) ;
#13419 = CARTESIAN_POINT ( 'NONE',  ( 6.524595623740805372, 5.074779492939383019, -7.015943501182343667 ) ) ;
#13420 = ORIENTED_EDGE ( 'NONE', *, *, #7566, .F. ) ;
#13421 = CARTESIAN_POINT ( 'NONE',  ( 108.0068349480237373, 18.21621961241920573, 4.414771370926589000 ) ) ;
#13422 = EDGE_CURVE ( 'NONE', #32470, #29481, #13742, .T. ) ;
#13423 = DIRECTION ( 'NONE',  ( -0.1908089953765452762, 0.000000000000000000, -0.9816271834476639757 ) ) ;
#13424 = EDGE_LOOP ( 'NONE', ( #12573, #7914, #13902, #6511 ) ) ;
#13425 = CARTESIAN_POINT ( 'NONE',  ( 23.17250000136559862, -3.024605502323851169, 0.3178988483021052969 ) ) ;
#13426 = CIRCLE ( 'NONE', #19850, 12.49867430706171767 ) ;
#13427 = VECTOR ( 'NONE', #11642, 1000.000000000000114 ) ;
#13428 = CARTESIAN_POINT ( 'NONE',  ( 109.4831014662948974, 20.77917954950586577, -0.4463807625373443777 ) ) ;
#13429 = CARTESIAN_POINT ( 'NONE',  ( -50.81000000000000227, -10.96999999999998643, 1.499999999999999556 ) ) ;
#13430 = VERTEX_POINT ( 'NONE', #24111 ) ;
#13431 = CARTESIAN_POINT ( 'NONE',  ( 1.302476151998225973, -9.311590272907336541, -1.500000000000000222 ) ) ;
#13432 = ORIENTED_EDGE ( 'NONE', *, *, #14781, .T. ) ;
#13433 = EDGE_CURVE ( 'NONE', #12626, #8184, #21083, .T. ) ;
#13434 = AXIS2_PLACEMENT_3D ( 'NONE', #8722, #31804, #18745 ) ;
#13435 = ORIENTED_EDGE ( 'NONE', *, *, #30202, .F. ) ;
#13436 = CARTESIAN_POINT ( 'NONE',  ( 23.93581954898842667, -2.707668749993698665, -1.915219082070890755 ) ) ;
#13437 = B_SPLINE_SURFACE_WITH_KNOTS ( 'NONE', 1, 3, ( 
 ( #9424, #10204, #2388, #15231 ),
 ( #20, #10539, #18228, #22914 ) ),
 .UNSPECIFIED., .F., .F., .F.,
 ( 2, 2 ),
 ( 4, 4 ),
 ( 0.000000000000000000, 1.000000000000000000 ),
 ( 0.0001138015799683909565, 0.0008863868760781655996 ),
 .UNSPECIFIED. ) ;
#13438 = DATE_TIME_ROLE ( 'classification_date' ) ;
#13440 = ORIENTED_EDGE ( 'NONE', *, *, #29044, .F. ) ;
#13439 = CARTESIAN_POINT ( 'NONE',  ( 22.98500000000000298, 2.486304738420679783, -0.2613211581691337604 ) ) ;
#13441 = ORIENTED_EDGE ( 'NONE', *, *, #29807, .F. ) ;
#13442 = CARTESIAN_POINT ( 'NONE',  ( 25.61000000136559507, 3.156283516753366047, 0.9349337715887203748 ) ) ;
#13443 = AXIS2_PLACEMENT_3D ( 'NONE', #5710, #15891, #3204 ) ;
#13444 = CIRCLE ( 'NONE', #32163, 0.7999999999999800604 ) ;
#13445 = AXIS2_PLACEMENT_3D ( 'NONE', #14438, #29336, #29848 ) ;
#13446 = EDGE_LOOP ( 'NONE', ( #9032, #9380, #8600, #3571 ) ) ;
#13447 = DIRECTION ( 'NONE',  ( -1.000000000000000000, -0.000000000000000000, 0.000000000000000000 ) ) ;
#13449 = ORIENTED_EDGE ( 'NONE', *, *, #12047, .T. ) ;
#13448 = CARTESIAN_POINT ( 'NONE',  ( 47.88345462391697538, -3.874360026377135391, -0.8105615593670084662 ) ) ;
#13450 = CONICAL_SURFACE ( 'NONE', #2796, 298.4532556727467068, 0.4915790642873356098 ) ;
#13451 = CARTESIAN_POINT ( 'NONE',  ( 17.80111248010111424, 13.30892117176750666, 1.049999999999999822 ) ) ;
#13452 = DIRECTION ( 'NONE',  ( 1.000000000000000000, -4.930380657631322689E-32, 8.654346879536960414E-15 ) ) ;
#13453 = B_SPLINE_CURVE_WITH_KNOTS ( 'NONE', 3,
 ( #23280, #382, #10556, #30968, #20930, #15074 ),
 .UNSPECIFIED., .F., .F.,
 ( 4, 2, 4 ),
 ( 0.4834212463832757156, 0.4917106231916378856, 0.5000000000000000000 ),
 .UNSPECIFIED. ) ;
#13454 = AXIS2_PLACEMENT_3D ( 'NONE', #20055, #22366, #32582 ) ;
#13455 = DIRECTION ( 'NONE',  ( 0.000000000000000000, 1.000000000000000000, 0.000000000000000000 ) ) ;
#13456 = DIRECTION ( 'NONE',  ( 1.000000000000000000, 0.000000000000000000, 0.000000000000000000 ) ) ;
#13457 = CYLINDRICAL_SURFACE ( 'NONE', #13904, 8.500000000000000000 ) ;
#13458 = VERTEX_POINT ( 'NONE', #19460 ) ;
#13459 = FACE_OUTER_BOUND ( 'NONE', #2429, .T. ) ;
#13460 = LINE ( 'NONE', #31228, #24666 ) ;
#13461 = CARTESIAN_POINT ( 'NONE',  ( 85.13336101766863351, -6.778540831288875523, -1.169950242242265848 ) ) ;
#13462 = CARTESIAN_POINT ( 'NONE',  ( -6.650050802731187538, 1.887961173149511618, 2.331437884370912705 ) ) ;
#13463 = EDGE_CURVE ( 'NONE', #29021, #30219, #10936, .T. ) ;
#13464 = EDGE_CURVE ( 'NONE', #4033, #2323, #1239, .T. ) ;
#13465 = DIRECTION ( 'NONE',  ( 3.623545766764298439E-17, 0.4226182617407088782, -0.9063077870366454958 ) ) ;
#13466 = CARTESIAN_POINT ( 'NONE',  ( 22.46520412490106722, -21.85309540019774843, 1.407654271148356395 ) ) ;
#13467 = FACE_OUTER_BOUND ( 'NONE', #21928, .T. ) ;
#13468 = CARTESIAN_POINT ( 'NONE',  ( 21.67755997557343406, -21.76174915994640102, 1.411535641067431124 ) ) ;
#13469 = AXIS2_PLACEMENT_3D ( 'NONE', #28241, #30435, #15535 ) ;
#13470 = CIRCLE ( 'NONE', #12404, 7.144028715714068056 ) ;
#13471 = CARTESIAN_POINT ( 'NONE',  ( 68.97545755171020687, -4.219822329617093359, 2.787783122621469989 ) ) ;
#13472 = ADVANCED_FACE ( 'NONE', ( #21452 ), #1884, .F. ) ;
#13473 = CARTESIAN_POINT ( 'NONE',  ( -2.362550801365593589, 2.752080473201636845, -2.228590825266444142 ) ) ;
#13474 = ORIENTED_EDGE ( 'NONE', *, *, #22237, .T. ) ;
#13475 = CONICAL_SURFACE ( 'NONE', #7620, 8.000000000000000000, 0.03490658503988666728 ) ;
#13476 = VECTOR ( 'NONE', #26150, 1000.000000000000000 ) ;
#13477 = CARTESIAN_POINT ( 'NONE',  ( -6.050050800000001061, 1.549418761218566143, -2.853674364686379583 ) ) ;
#13478 = SHAPE_REPRESENTATION ( 'Part4_Gear', ( #2865 ), #32200 ) ;
#13479 = CLOSED_SHELL ( 'NONE', ( #19164, #24832, #16483, #3568, #1131, #11848, #3909, #17850, #31379, #18029, #6535, #30831, #6281, #8244, #28349, #4579, #27194, #1794, #27588, #27747, #7755, #700, #5113, #23433, #20133, #28197, #6823, #18956, #15748, #21820, #820, #28638, #3117, #23275, #31627, #10031, #8446, #28951, #28475, #22032, #21858, #16087, #30352, #32902, #16764, #29113, #7795, #22684, #7711, #8376, #15497, #31119, #27380, #9740, #14782, #5748, #26333, #4224, #27772, #2509, #32649, #23301, #32475, #10136, #8637, #3923, #15900, #14177, #32860, #14606, #16756, #14958, #19141, #11802, #22975, #11655, #5611, #17391, #17291, #29712, #5715, #7911, #17216, #27280, #17685, #8451, #21898, #28625, #18865, #10372, #3671, #4789, #23728, #31845, #11789, #5151, #15631, #11584, #16365, #24369, #23845, #25819, #29773, #8721, #81, #18746, #10603, #8337, #13049, #31021, #13576, #24023, #8571, #23157, #31762, #28021, #3740, #7350, #15389, #26162, #19988, #2871, #21850, #27485, #24104, #5645, #3590, #21788, #27831, #11824, #19004, #23052, #25058, #1950, #4307, #28122, #20701, #31896, #26325, #22412, #23064, #14233, #14998, #7861, #32046, #12993, #6643, #26726, #27599, #3296, #16261, #31498, #8172, #3861, #9898, #9526, #22406, #18419, #21840, #12675, #31433, #14105, #26871, #9813, #25163, #362, #18503, #27329, #1701 ) ) ;
#13480 = CARTESIAN_POINT ( 'NONE',  ( 13.04731869766886554, 19.33256796700939262, -5.396302277755719246 ) ) ;
#13481 = CARTESIAN_POINT ( 'NONE',  ( -5.100050799999999995, 2.983565686104819648, 0.3135853898029609677 ) ) ;
#13482 = CARTESIAN_POINT ( 'NONE',  ( 9.851448551970788614, -11.91728849095426135, 1.499999999999785283 ) ) ;
#13483 = AXIS2_PLACEMENT_3D ( 'NONE', #32715, #22829, #25501 ) ;
#13484 = VERTEX_POINT ( 'NONE', #21288 ) ;
#13485 = DIRECTION ( 'NONE',  ( -1.000000000000000000, 0.000000000000000000, 0.000000000000000000 ) ) ;
#13486 = AXIS2_PLACEMENT_3D ( 'NONE', #12211, #4056, #14222 ) ;
#13487 = EDGE_CURVE ( 'NONE', #29313, #28440, #1404, .T. ) ;
#13488 = ORIENTED_EDGE ( 'NONE', *, *, #13201, .F. ) ;
#13489 = DIRECTION ( 'NONE',  ( 0.000000000000000000, -0.9961946980917465444, 0.08715574274764703588 ) ) ;
#13490 = DATE_TIME_ROLE ( 'creation_date' ) ;
#13491 = CARTESIAN_POINT ( 'NONE',  ( 28.69228937106727528, -5.666394676789348495, 4.074610069494389641 ) ) ;
#13492 = FACE_OUTER_BOUND ( 'NONE', #21225, .T. ) ;
#13493 = VECTOR ( 'NONE', #22699, 1000.000000000000114 ) ;
#13494 = CARTESIAN_POINT ( 'NONE',  ( 5.377543748152551650, 6.139290821770257089, 5.151476664237498504 ) ) ;
#13495 = CIRCLE ( 'NONE', #23646, 10.51776515689528502 ) ;
#13496 = ORIENTED_EDGE ( 'NONE', *, *, #16890, .F. ) ;
#13497 = VECTOR ( 'NONE', #18126, 1000.000000000000114 ) ;
#13498 = PLANE ( 'NONE',  #17309 ) ;
#13499 = DIRECTION ( 'NONE',  ( 0.000000000000000000, -0.2588190451025066396, -0.9659258262890719759 ) ) ;
#13500 = VECTOR ( 'NONE', #13188, 1000.000000000000114 ) ;
#13501 = CARTESIAN_POINT ( 'NONE',  ( 21.92250000136559507, 0.3178988483021036315, 3.024605502323848949 ) ) ;
#13502 = CIRCLE ( 'NONE', #17790, 2.999999999999999112 ) ;
#13504 = ORIENTED_EDGE ( 'NONE', *, *, #9068, .F. ) ;
#13503 = CARTESIAN_POINT ( 'NONE',  ( 108.1834173863008886, 19.19950030484896786, -3.592082168559364241 ) ) ;
#13505 = CARTESIAN_POINT ( 'NONE',  ( -3.962550801365593234, 2.752080473201636845, -2.228590825266444142 ) ) ;
#13506 = CARTESIAN_POINT ( 'NONE',  ( 18.64036474502219320, -7.197223105236783880, 1.868788737059465799 ) ) ;
#13507 = CARTESIAN_POINT ( 'NONE',  ( 47.94319819119471049, -7.452467522295798119, -2.787782382176030360 ) ) ;
#13508 = EDGE_CURVE ( 'NONE', #115, #12922, #28026, .T. ) ;
#13509 =( GEOMETRIC_REPRESENTATION_CONTEXT ( 3 ) GLOBAL_UNCERTAINTY_ASSIGNED_CONTEXT ( ( #8900 ) ) GLOBAL_UNIT_ASSIGNED_CONTEXT ( ( #18799, #32315, #4550 ) ) REPRESENTATION_CONTEXT ( 'NONE', 'WORKASPACE' ) );
#13510 = VERTEX_POINT ( 'NONE', #6734 ) ;
#13511 = ORIENTED_EDGE ( 'NONE', *, *, #11632, .F. ) ;
#13512 = DIRECTION ( 'NONE',  ( -3.623545766764303986E-17, -0.4226182617407096553, 0.9063077870366452737 ) ) ;
#13513 = CARTESIAN_POINT ( 'NONE',  ( 107.6648144168582348, -20.46701934092476449, -1.481717219551038411 ) ) ;
#13514 = CARTESIAN_POINT ( 'NONE',  ( -1.671916146696592831, -10.12145986844939927, 5.485967528433935314 ) ) ;
#13515 = CARTESIAN_POINT ( 'NONE',  ( -30.51827900900860158, 4.402097243136377180, 5.049999999999999822 ) ) ;
#13516 = CARTESIAN_POINT ( 'NONE',  ( 0.5032039771612126788, 2.299586922890515694, 9.456648240374278203 ) ) ;
#13517 = CIRCLE ( 'NONE', #32764, 1.676012832569465205 ) ;
#13518 = CARTESIAN_POINT ( 'NONE',  ( -59.40911793129208007, -5.269765563131745267, 5.315798354995362018 ) ) ;
#13519 = AXIS2_PLACEMENT_3D ( 'NONE', #17405, #24208, #21215 ) ;
#13520 = CARTESIAN_POINT ( 'NONE',  ( -3.637550801365593944, -3.675193018007245627, 1.088641768524163389 ) ) ;
#13521 = CARTESIAN_POINT ( 'NONE',  ( 12.44989959798878232, 19.51744974835124680, 2.318435636271098943 ) ) ;
#13522 = CARTESIAN_POINT ( 'NONE',  ( 55.02542983044659763, -8.237060396196271839, 0.4367666027049950661 ) ) ;
#13523 = ORIENTED_EDGE ( 'NONE', *, *, #21609, .F. ) ;
#13524 = CARTESIAN_POINT ( 'NONE',  ( -2.767073886773233848, -0.6621507858625358400, 1.748408842879327851 ) ) ;
#13525 = VECTOR ( 'NONE', #11402, 1000.000000000000000 ) ;
#13526 = AXIS2_PLACEMENT_3D ( 'NONE', #19194, #16356, #31764 ) ;
#13527 = EDGE_CURVE ( 'NONE', #6094, #30847, #29093, .T. ) ;
#13528 = ORIENTED_EDGE ( 'NONE', *, *, #16885, .T. ) ;
#13529 = SHAPE_DEFINITION_REPRESENTATION ( #14545, #3460 ) ;
#13531 = CARTESIAN_POINT ( 'NONE',  ( 40.88398618353106428, -6.895614549178633368, 3.995006151606554479 ) ) ;
#13530 = LOCAL_TIME ( 16, 7, 10.00000000000000000, #5354 ) ;
#13532 = CARTESIAN_POINT ( 'NONE',  ( -3.135269660805080516, -0.5000000000000000000, 1.500000000000000000 ) ) ;
#13533 = ORIENTED_EDGE ( 'NONE', *, *, #20041, .F. ) ;
#13534 = DIRECTION ( 'NONE',  ( 0.000000000000000000, 0.000000000000000000, 1.000000000000000000 ) ) ;
#13535 = ORIENTED_EDGE ( 'NONE', *, *, #5693, .T. ) ;
#13536 = ORIENTED_EDGE ( 'NONE', *, *, #12269, .F. ) ;
#13537 = CARTESIAN_POINT ( 'NONE',  ( -15.26206363037219838, -21.68942756709465769, 1.499999999999998668 ) ) ;
#13538 = CARTESIAN_POINT ( 'NONE',  ( -4.712550801365592790, 3.675193018007246959, -1.088641768524161391 ) ) ;
#13539 = EDGE_CURVE ( 'NONE', #429, #18469, #6385, .T. ) ;
#13540 = CARTESIAN_POINT ( 'NONE',  ( 14.08105513877605652, -14.60666186089171603, 1.499999999999999556 ) ) ;
#13541 = CARTESIAN_POINT ( 'NONE',  ( 10.57125986779756843, -0.6226916219172400346, 4.971152295393299170 ) ) ;
#13543 = ORIENTED_EDGE ( 'NONE', *, *, #11006, .F. ) ;
#13542 = CARTESIAN_POINT ( 'NONE',  ( 0.000000000000000000, -8.264486777890139635, 4.472189673936756371 ) ) ;
#13544 = AXIS2_PLACEMENT_3D ( 'NONE', #12398, #14385, #32647 ) ;
#13545 = CARTESIAN_POINT ( 'NONE',  ( -5.537550801365594744, 3.368539882008727115, 1.828967928396026954 ) ) ;
#13546 = CARTESIAN_POINT ( 'NONE',  ( 14.99916604845051360, 9.584522669134234008, 1.500000000000000000 ) ) ;
#13547 = ADVANCED_FACE ( 'NONE', ( #14089, #6234 ), #16581, .T. ) ;
#13548 = CARTESIAN_POINT ( 'NONE',  ( 15.97646010100271496, -20.81270992525872288, 1.751026346556933344 ) ) ;
#13549 = CARTESIAN_POINT ( 'NONE',  ( 21.61000000136559507, 3.156283516753366047, 0.9349337715887203748 ) ) ;
#13550 = AXIS2_PLACEMENT_3D ( 'NONE', #23472, #11263, #31683 ) ;
#13552 = ORIENTED_EDGE ( 'NONE', *, *, #22410, .F. ) ;
#13551 = CARTESIAN_POINT ( 'NONE',  ( 24.39659513448239991, -17.41072360183627055, 1.416990234759656575 ) ) ;
#13553 = B_SPLINE_CURVE_WITH_KNOTS ( 'NONE', 3,
 ( #30691, #10581, #25319, #20787, #30990, #12598, #22802, #7584, #7766, #17957 ),
 .UNSPECIFIED., .F., .F.,
 ( 4, 2, 2, 2, 4 ),
 ( 2.571685856645629606E-07, 0.0005478592107668799017, 0.001095461252948095243, 0.001643063295129310476, 0.002190665337310525925 ),
 .UNSPECIFIED. ) ;
#13554 = LINE ( 'NONE', #4149, #2825 ) ;
#13555 = CARTESIAN_POINT ( 'NONE',  ( 21.29750000273119070, 2.594547506269380133, 0.7685399846772031918 ) ) ;
#13556 = LOCAL_TIME ( 16, 7, 10.00000000000000000, #22007 ) ;
#13557 = CARTESIAN_POINT ( 'NONE',  ( 25.52557118915448342, -17.56218954043521663, 1.078818518451832409 ) ) ;
#13558 = CARTESIAN_POINT ( 'NONE',  ( 110.2274383572228942, 17.36892446252421962, 4.629213727441584325 ) ) ;
#13559 = DIRECTION ( 'NONE',  ( -0.1908089953765453595, -4.729706814396277527E-15, 0.9816271834476638647 ) ) ;
#13560 = DIRECTION ( 'NONE',  ( -1.000000000000000000, 0.000000000000000000, 0.000000000000000000 ) ) ;
#13561 = DIRECTION ( 'NONE',  ( 0.1027947991993880122, -0.9947025833170222153, 0.000000000000000000 ) ) ;
#13562 = CARTESIAN_POINT ( 'NONE',  ( -4.687550801365594211, 2.228590825266444142, 2.752080473201636845 ) ) ;
#13563 = ORIENTED_EDGE ( 'NONE', *, *, #21502, .F. ) ;
#13564 = FACE_OUTER_BOUND ( 'NONE', #26227, .T. ) ;
#13565 = CARTESIAN_POINT ( 'NONE',  ( 18.65791233782715963, -7.001076235476726417, -2.184956778830003277 ) ) ;
#13566 = LINE ( 'NONE', #14059, #17815 ) ;
#13568 = CARTESIAN_POINT ( 'NONE',  ( 107.4502445245915254, -17.36287206927810089, 4.529451243851331910 ) ) ;
#13567 = LINE ( 'NONE', #26120, #25718 ) ;
#13569 = ORIENTED_EDGE ( 'NONE', *, *, #20385, .F. ) ;
#13570 = DIRECTION ( 'NONE',  ( -0.7849335118354594520, -0.6195800045172962234, -0.000000000000000000 ) ) ;
#13571 = ORIENTED_EDGE ( 'NONE', *, *, #3964, .F. ) ;
#13572 = DIRECTION ( 'NONE',  ( -1.000000000000000000, 0.000000000000000000, 0.000000000000000000 ) ) ;
#13574 = ORIENTED_EDGE ( 'NONE', *, *, #22535, .T. ) ;
#13573 = CARTESIAN_POINT ( 'NONE',  ( 19.01480233880806381, -3.011762293215139330, 0.07017451552781951707 ) ) ;
#13575 = ORIENTED_EDGE ( 'NONE', *, *, #27526, .F. ) ;
#13576 = ADVANCED_FACE ( 'NONE', ( #21774 ), #31983, .F. ) ;
#13577 = FACE_OUTER_BOUND ( 'NONE', #4918, .T. ) ;
#13578 = LOCAL_TIME ( 16, 7, 10.00000000000000000, #30876 ) ;
#13579 = ADVANCED_FACE ( 'NONE', ( #27119 ), #3486, .T. ) ;
#13580 = EDGE_CURVE ( 'NONE', #26388, #7529, #31489, .T. ) ;
#13581 = CARTESIAN_POINT ( 'NONE',  ( -50.60000000000000142, -10.96966150227468972, 7.500000000000000000 ) ) ;
#13583 = ORIENTED_EDGE ( 'NONE', *, *, #29897, .F. ) ;
#13582 = CARTESIAN_POINT ( 'NONE',  ( 0.000000000000000000, -0.5000000000000000000, -1.000000000000000000 ) ) ;
#13584 = CARTESIAN_POINT ( 'NONE',  ( 13.48264087563610580, 7.964219514463561467, -1.500000000000000000 ) ) ;
#13585 = CARTESIAN_POINT ( 'NONE',  ( -3.064492245890347188, 0.000000000000000000, -1.000000000000000222 ) ) ;
#13586 = DIRECTION ( 'NONE',  ( 0.000000000000000000, 0.9063077870366492705, 0.4226182617407007180 ) ) ;
#13587 = CARTESIAN_POINT ( 'NONE',  ( 19.32480846800323349, -16.28061487828787790, -1.500000000000000000 ) ) ;
#13588 = CARTESIAN_POINT ( 'NONE',  ( 107.4498871846200814, -17.35770398095254663, -4.515330059624638182 ) ) ;
#13589 = CARTESIAN_POINT ( 'NONE',  ( 0.000000000000000000, -2.652816298622461932, 5.657964889053573643 ) ) ;
#13590 = CIRCLE ( 'NONE', #10410, 6.248999999999999666 ) ;
#13591 = LINE ( 'NONE', #28313, #20367 ) ;
#13592 = CARTESIAN_POINT ( 'NONE',  ( 25.00111451137534146, -4.139597703811366476E-17, -2.499999999999998668 ) ) ;
#13593 = DIRECTION ( 'NONE',  ( 1.000000000000000000, -0.000000000000000000, -0.000000000000000000 ) ) ;
#13594 = CARTESIAN_POINT ( 'NONE',  ( 13.65718777918027271, -19.09288791508984673, 4.522129901861158707 ) ) ;
#13595 = CARTESIAN_POINT ( 'NONE',  ( 2.281627749324421917, -0.2935656086769610207, 1.757435426329174488 ) ) ;
#13596 = ORIENTED_EDGE ( 'NONE', *, *, #4534, .F. ) ;
#13597 = CARTESIAN_POINT ( 'NONE',  ( 6.037141848526921706, -3.315649934461669002, -7.798898458906313280 ) ) ;
#13598 = CARTESIAN_POINT ( 'NONE',  ( 107.3983896896722570, -16.61650204647006390, -2.997325617849243784 ) ) ;
#13599 = PLANE ( 'NONE',  #711 ) ;
#13600 = EDGE_LOOP ( 'NONE', ( #8586, #23442, #29004, #21969, #3492, #17146 ) ) ;
#13601 = CARTESIAN_POINT ( 'NONE',  ( 22.29750000136559507, -2.363507492473152283, -1.913930629741525280 ) ) ;
#13602 = CARTESIAN_POINT ( 'NONE',  ( 25.55028516831285756, -0.3470411663994143470, -2.799286153339490379 ) ) ;
#13603 = CARTESIAN_POINT ( 'NONE',  ( -23.35000000000000142, -10.96966150227469505, 4.000000000000000000 ) ) ;
#13604 = ORIENTED_EDGE ( 'NONE', *, *, #3841, .T. ) ;
#13605 = CARTESIAN_POINT ( 'NONE',  ( 0.6160563202711623054, -5.544449031061736477, -1.499999999999999556 ) ) ;
#13606 =( NAMED_UNIT ( * ) SI_UNIT ( $, .STERADIAN. ) SOLID_ANGLE_UNIT ( ) );
#13607 = ORIENTED_EDGE ( 'NONE', *, *, #12569, .F. ) ;
#13608 = ADVANCED_FACE ( 'NONE', ( #32339 ), #4572, .T. ) ;
#13609 = ORIENTED_EDGE ( 'NONE', *, *, #32581, .T. ) ;
#13610 = FACE_OUTER_BOUND ( 'NONE', #25706, .T. ) ;
#13611 = APPROVAL_ROLE ( '' ) ;
#13613 = ORIENTED_EDGE ( 'NONE', *, *, #7159, .F. ) ;
#13612 = DIRECTION ( 'NONE',  ( -1.000000000000000000, 8.574039729943018344E-17, -0.000000000000000000 ) ) ;
#13614 = ORIENTED_EDGE ( 'NONE', *, *, #18107, .F. ) ;
#13615 = CARTESIAN_POINT ( 'NONE',  ( 2.866494652514124830, 9.241976615262203154, 2.300561732649596181 ) ) ;
#13616 = EDGE_CURVE ( 'NONE', #32155, #30480, #29971, .T. ) ;
#13617 = B_SPLINE_CURVE_WITH_KNOTS ( 'NONE', 3,
 ( #11488, #4286, #1802, #31739, #19517, #32395, #9456, #29713, #16478, #16331, #19673, #21684, #1463, #11639, #6793, #6149, #8815, #21834, #32047, #19020 ),
 .UNSPECIFIED., .F., .F.,
 ( 4, 2, 2, 2, 2, 2, 2, 2, 2, 4 ),
 ( 0.0002980439675631849604, 0.003522811531434848643, 0.006747579095306512759, 0.009972346659178177308, 0.01319711422304984012, 0.01642188178692150294, 0.01964664935079316749, 0.02125903313272899456, 0.02287141691466482163, 0.02609618447853648271 ),
 .UNSPECIFIED. ) ;
#13618 = ORIENTED_EDGE ( 'NONE', *, *, #29243, .F. ) ;
#13619 = CARTESIAN_POINT ( 'NONE',  ( -35.00000000000000000, -0.06979899340500209104, -1.001218345961804257 ) ) ;
#13621 = ORIENTED_EDGE ( 'NONE', *, *, #26518, .T. ) ;
#13620 = CARTESIAN_POINT ( 'NONE',  ( 102.2268587688198664, -1.179183864763411416, -0.8105616763788804358 ) ) ;
#13622 = DIRECTION ( 'NONE',  ( 1.000000000000000000, -0.000000000000000000, -0.000000000000000000 ) ) ;
#13623 = LINE ( 'NONE', #19307, #21860 ) ;
#13624 = EDGE_CURVE ( 'NONE', #24971, #14880, #5074, .T. ) ;
#13625 = LINE ( 'NONE', #29024, #23997 ) ;
#13626 = DIRECTION ( 'NONE',  ( 0.06927878976713386372, -0.9975973382524639943, 0.000000000000000000 ) ) ;
#13627 = CARTESIAN_POINT ( 'NONE',  ( 108.0616230038786796, -18.95671804260016913, 4.502323035491692771 ) ) ;
#13628 = CARTESIAN_POINT ( 'NONE',  ( 3.063284526845909017, -8.734705317652711187, 0.4999240074859884198 ) ) ;
#13629 = FACE_OUTER_BOUND ( 'NONE', #24484, .T. ) ;
#13630 = ADVANCED_FACE ( 'NONE', ( #1727 ), #9810, .T. ) ;
#13631 = CARTESIAN_POINT ( 'NONE',  ( 47.95270804829431910, -8.021719045402210924, -1.873788950395596897 ) ) ;
#13632 = PLANE ( 'NONE',  #24262 ) ;
#13633 = CARTESIAN_POINT ( 'NONE',  ( -3.688478485700421711E-13, 5.227991826304162259, -9.620177616658798669 ) ) ;
#13634 = CARTESIAN_POINT ( 'NONE',  ( 26.20274081918672593, 20.47280333234597194, -4.999054092451830300 ) ) ;
#13635 = CARTESIAN_POINT ( 'NONE',  ( 22.67250000273118715, -2.378061970571983430, 1.291182301015471490 ) ) ;
#13636 = FACE_OUTER_BOUND ( 'NONE', #24427, .T. ) ;
#13637 = EDGE_CURVE ( 'NONE', #10538, #10650, #21252, .T. ) ;
#13638 = CARTESIAN_POINT ( 'NONE',  ( 3.148734258548822534E-16, 3.672404558090086368, -3.407865132560142563 ) ) ;
#13639 = CARTESIAN_POINT ( 'NONE',  ( -2.412550801365592967, 1.828967928396027176, -3.368539882008727115 ) ) ;
#13640 = ORIENTED_EDGE ( 'NONE', *, *, #17437, .T. ) ;
#13641 = CARTESIAN_POINT ( 'NONE',  ( -6.350050800000000883, -3.113457007523259268, 0.9222479816126455399 ) ) ;
#13642 = EDGE_CURVE ( 'NONE', #15020, #19834, #13590, .T. ) ;
#13643 = CARTESIAN_POINT ( 'NONE',  ( 107.9719557256307354, -17.66553154178031093, 4.376786827539821623 ) ) ;
#13644 = CARTESIAN_POINT ( 'NONE',  ( 25.24521618911088794, -7.644457093038323125E-15, 2.510216189110891172 ) ) ;
#13645 = CARTESIAN_POINT ( 'NONE',  ( 9.283830569141708011, -0.1241467202049961749, 1.000000000000000000 ) ) ;
#13646 = ORIENTED_EDGE ( 'NONE', *, *, #7148, .F. ) ;
#13647 = CARTESIAN_POINT ( 'NONE',  ( 40.87351160866354149, -4.997573076401069514, -2.787782134466627149 ) ) ;
#13648 = VERTEX_POINT ( 'NONE', #1520 ) ;
#13649 = CARTESIAN_POINT ( 'NONE',  ( 4.969883781861252459, -12.47903377700913907, 1.500000000000000000 ) ) ;
#13650 = APPROVAL_ROLE ( '' ) ;
#13651 = EDGE_CURVE ( 'NONE', #10864, #18045, #6042, .T. ) ;
#13652 = CARTESIAN_POINT ( 'NONE',  ( 102.4008411508974064, -3.675699656476595578, 4.275175836083139558 ) ) ;
#13653 = EDGE_CURVE ( 'NONE', #28345, #28296, #26594, .T. ) ;
#13654 = CARTESIAN_POINT ( 'NONE',  ( 8.930755659321954809, 0.4999999999534671113, 1.500000000000000000 ) ) ;
#13655 = CARTESIAN_POINT ( 'NONE',  ( 23.86874014608191175, -17.38228585591196307, -1.471223822905572076 ) ) ;
#13656 = CARTESIAN_POINT ( 'NONE',  ( -35.00000000000000000, 0.000000000000000000, -0.9987809114023521451 ) ) ;
#13657 = ORIENTED_EDGE ( 'NONE', *, *, #692, .F. ) ;
#13658 = ADVANCED_FACE ( 'NONE', ( #6696 ), #1683, .F. ) ;
#13659 = CARTESIAN_POINT ( 'NONE',  ( 18.77131732058334279, -5.733436128961898248, 4.171867820445585018 ) ) ;
#13660 = CARTESIAN_POINT ( 'NONE',  ( 0.3045634671934228099, 10.22982953726899780, -0.9829946734957932808 ) ) ;
#13661 = CARTESIAN_POINT ( 'NONE',  ( 21.61000000136559507, 2.892927487894327410, -1.570731468192931635 ) ) ;
#13663 = ORIENTED_EDGE ( 'NONE', *, *, #22773, .F. ) ;
#13662 = CARTESIAN_POINT ( 'NONE',  ( 3.249999999999999556, 0.000000000000000000, -6.999999999999998224 ) ) ;
#13664 = CARTESIAN_POINT ( 'NONE',  ( -2.212550801365593234, 3.368539882008727115, 1.828967928396026954 ) ) ;
#13665 = CARTESIAN_POINT ( 'NONE',  ( 108.1834172094735749, 19.19949932020479366, 3.608602272731602500 ) ) ;
#13666 = CARTESIAN_POINT ( 'NONE',  ( 18.65791233782715963, -7.001076235476726417, -2.184956778830005053 ) ) ;
#13667 = ORIENTED_EDGE ( 'NONE', *, *, #25378, .T. ) ;
#13668 = ORIENTED_EDGE ( 'NONE', *, *, #29969, .F. ) ;
#13669 = ADVANCED_FACE ( 'NONE', ( #12046 ), #27496, .T. ) ;
#13670 = CARTESIAN_POINT ( 'NONE',  ( 107.8192872773860245, -18.91580487786033515, 4.500888494199039691 ) ) ;
#13671 =( BOUNDED_SURFACE ( )  B_SPLINE_SURFACE ( 3, 2, ( 
 ( #1420, #21792, #1076 ),
 ( #5923, #18804, #31506 ),
 ( #21160, #18629, #21477 ),
 ( #3601, #26813, #6406 ),
 ( #24453, #11447, #16115 ),
 ( #31999, #24135, #18977 ),
 ( #6251, #28825, #26500 ),
 ( #16604, #8591, #24308 ),
 ( #16437, #1263, #21641 ),
 ( #29010, #11106, #6108 ) ),
 .UNSPECIFIED., .F., .F., .F. ) 
 B_SPLINE_SURFACE_WITH_KNOTS ( ( 4, 2, 2, 2, 4 ),
 ( 3, 3 ),
 ( 0.01348603581696579921, 0.01365687529134765321, 0.01382771476572950548, 0.01416939371449321000, 0.01485275161202062079 ),
 ( 0.000000000000000000, 1.000000000000000000 ),
 .UNSPECIFIED. ) 
 GEOMETRIC_REPRESENTATION_ITEM ( )  RATIONAL_B_SPLINE_SURFACE ( (
 ( 1.000000000000000000, 0.9948736491435667961, 1.000000000000000000),
 ( 1.000000000000000000, 0.9948794564610742297, 1.000000000000000000),
 ( 1.000000000000000000, 0.9935082075948258318, 1.000000000000000000),
 ( 1.000000000000000000, 0.9898246045860391584, 1.000000000000000000),
 ( 1.000000000000000000, 0.9875779995959506063, 1.000000000000000000),
 ( 1.000000000000000000, 0.9804235948790372968, 1.000000000000000000),
 ( 1.000000000000000000, 0.9752522326728655377, 1.000000000000000000),
 ( 1.000000000000000000, 0.9593679678191086024, 1.000000000000000000),
 ( 1.000000000000000000, 0.9482314950096560890, 1.000000000000000000),
 ( 1.000000000000000000, 0.9372872368324044468, 1.000000000000000000) ) ) 
 REPRESENTATION_ITEM ( '' )  SURFACE ( )  );
#13672 = LINE ( 'NONE', #982, #31066 ) ;
#13673 = CARTESIAN_POINT ( 'NONE',  ( 5.377543748152549874, -5.151476664237518044, 6.139290821770238438 ) ) ;
#13674 = FACE_OUTER_BOUND ( 'NONE', #2459, .T. ) ;
#13675 = DIRECTION ( 'NONE',  ( -0.000000000000000000, 0.000000000000000000, 1.000000000000000000 ) ) ;
#13676 = CARTESIAN_POINT ( 'NONE',  ( -15.51216819290874227, -25.44850941282521006, 1.500000000000000000 ) ) ;
#13677 = DIRECTION ( 'NONE',  ( 1.000000000000000000, -8.574039729943018344E-17, -0.000000000000000000 ) ) ;
#13678 = CARTESIAN_POINT ( 'NONE',  ( -4.787550801365593856, 3.521866450007987037, 0.3701630799359328372 ) ) ;
#13679 = DIRECTION ( 'NONE',  ( -0.4999999999999960032, -0.8660254037844409281, -0.000000000000000000 ) ) ;
#13680 = CARTESIAN_POINT ( 'NONE',  ( 69.14957877370534334, -7.691922716132707727, 1.169951105759795329 ) ) ;
#13681 = VERTEX_POINT ( 'NONE', #9362 ) ;
#13682 = DIRECTION ( 'NONE',  ( 0.000000000000000000, 0.000000000000000000, 1.000000000000000000 ) ) ;
#13683 = EDGE_CURVE ( 'NONE', #10415, #14000, #25884, .T. ) ;
#13684 = ORIENTED_EDGE ( 'NONE', *, *, #21448, .F. ) ;
#13685 = PERSON_AND_ORGANIZATION_ROLE ( 'creator' ) ;
#13686 = EDGE_CURVE ( 'NONE', #3747, #2818, #22153, .T. ) ;
#13687 = CARTESIAN_POINT ( 'NONE',  ( 18.75837163099988558, -5.878142956378915152, 3.995006647689397283 ) ) ;
#13688 = EDGE_CURVE ( 'NONE', #7632, #13010, #7746, .T. ) ;
#13689 = DIRECTION ( 'NONE',  ( -1.000000000000000000, -0.000000000000000000, -0.000000000000000000 ) ) ;
#13690 = ORIENTED_EDGE ( 'NONE', *, *, #14657, .T. ) ;
#13691 = CARTESIAN_POINT ( 'NONE',  ( -2.681117189733320139, -7.739668020571214980E-17, -1.353799989032657303 ) ) ;
#13692 = ORIENTED_EDGE ( 'NONE', *, *, #1917, .F. ) ;
#13693 = ORIENTED_EDGE ( 'NONE', *, *, #9825, .T. ) ;
#13694 = CARTESIAN_POINT ( 'NONE',  ( 6.220890055307039646, -15.20372210278347680, -4.522129901861164925 ) ) ;
#13695 = CARTESIAN_POINT ( 'NONE',  ( -3.212550801365593678, 1.828967928396027398, -3.368539882008727115 ) ) ;
#13696 = LINE ( 'NONE', #15883, #25786 ) ;
#13697 = B_SPLINE_CURVE_WITH_KNOTS ( 'NONE', 3,
 ( #13805, #3649, #16838, #19175, #29367, #4137, #22022, #24198 ),
 .UNSPECIFIED., .F., .F.,
 ( 4, 2, 2, 4 ),
 ( 2.304311362615608600E-07, 0.001261163669367360842, 0.001891630288482910351, 0.002522096907598460076 ),
 .UNSPECIFIED. ) ;
#13698 = CARTESIAN_POINT ( 'NONE',  ( 0.1307775883147231089, -6.173461807542353519, -1.772482830384789265 ) ) ;
#13700 = ORIENTED_EDGE ( 'NONE', *, *, #15105, .F. ) ;
#13699 = CARTESIAN_POINT ( 'NONE',  ( -23.54713438637982748, 8.434582260019382716, 8.205946861809124471 ) ) ;
#13701 = CARTESIAN_POINT ( 'NONE',  ( -8.087550801365594566, 2.752080473201636845, -2.228590825266444142 ) ) ;
#13702 = CARTESIAN_POINT ( 'NONE',  ( 18.72918216980634298, 14.91508072752954739, 1.500000000000000222 ) ) ;
#13703 = B_SPLINE_CURVE_WITH_KNOTS ( 'NONE', 3,
 ( #3020, #23534, #13175, #18193, #26221, #23376, #10663 ),
 .UNSPECIFIED., .F., .F.,
 ( 4, 3, 4 ),
 ( 0.000000000000000000, 1.028838076071613430E-05, 3.621257616738532545E-05 ),
 .UNSPECIFIED. ) ;
#13704 = CARTESIAN_POINT ( 'NONE',  ( -33.81874022276151948, 19.51744974835125035, -2.318435636271050537 ) ) ;
#13705 = CARTESIAN_POINT ( 'NONE',  ( 21.86000000136559507, -0.9349337715887248157, 3.156283516753367824 ) ) ;
#13707 = EDGE_LOOP ( 'NONE', ( #31704, #15601, #12159 ) ) ;
#13706 = CARTESIAN_POINT ( 'NONE',  ( 23.71271855738436329, -17.43088677775550011, 1.604577790254628100 ) ) ;
#13708 = ADVANCED_FACE ( 'NONE', ( #19915 ), #27430, .T. ) ;
#13709 = CARTESIAN_POINT ( 'NONE',  ( 101.9216173105994443, -5.769792427975438009, 0.07017451552781736601 ) ) ;
#13710 = CARTESIAN_POINT ( 'NONE',  ( 23.48500000273119070, 0.2613211581691317065, 2.486304738420681559 ) ) ;
#13711 = CARTESIAN_POINT ( 'NONE',  ( -17.84619894073314583, 6.485688093852441050, 1.500000000000000000 ) ) ;
#13712 = FACE_OUTER_BOUND ( 'NONE', #2849, .T. ) ;
#13713 = CARTESIAN_POINT ( 'NONE',  ( -3.349888966845140370, -1.984772134521467502, -1.747784021618837835 ) ) ;
#13714 = CARTESIAN_POINT ( 'NONE',  ( 2.970200414851740245, -2.288523046050797038, 8.870914041964226726 ) ) ;
#13715 = B_SPLINE_SURFACE_WITH_KNOTS ( 'NONE', 3, 3, ( 
 ( #10922, #13880, #4382, #4201, #14371, #6866, #14068 ),
 ( #16404, #21920, #26953, #4057, #1217, #32140, #24273 ),
 ( #9035, #1387, #11562, #11906, #6368, #1708, #22110 ),
 ( #24579, #16560, #9214, #32324, #21759, #31966, #27263 ),
 ( #32472, #26612, #3716, #12068, #17056, #22263, #9382 ),
 ( #19443, #29635, #14568, #19592, #19252, #27100, #24773 ),
 ( #6716, #11717, #16907, #29282, #26774, #1893, #29454 ),
 ( #29791, #9534, #24090, #6554, #16752, #19748, #14223 ),
 ( #24421, #3892, #6217, #1538, #11410, #21607, #31812 ),
 ( #8883, #19092, #27454, #25268, #28104, #22760, #7222 ),
 ( #7528, #24927, #5202, #2385, #15377, #2040, #10037 ),
 ( #2195, #14729, #12866, #2539, #30641, #12212, #15228 ),
 ( #25585, #22418, #20424, #30293, #32630, #2696, #9886 ),
 ( #23089, #7040, #4710, #4556, #210, #27943, #5051 ),
 ( #14879, #17412, #17251, #12557, #17558, #27756, #9711 ),
 ( #25081, #25431, #32815, #12383, #22603, #12709, #30145 ),
 ( #22911, #20102, #17, #27607, #32969, #10200, #7368 ),
 ( #17913, #4864, #10385, #19938, #15048, #29949, #7720 ),
 ( #20248, #30450, #17734, #23563, #29360, #26685, #25937 ),
 ( #6450, #15732, #5549, #16656, #1464, #7871, #15876 ),
 ( #10692, #21685, #3191, #19168, #5363, #20902, #23402 ),
 ( #13353, #24350, #23257, #687, #13969, #26865, #29205 ),
 ( #3983, #20594, #19021, #28604, #14152, #31125, #30803 ),
 ( #10879, #21087, #8214, #26086, #18413, #31288, #5698 ),
 ( #8816, #18063, #20747, #6295, #28252, #16479, #15547 ),
 ( #3800, #25764, #507, #18224, #13199, #11489, #24189 ),
 ( #13058, #1314, #8957, #31891, #2893, #360, #10536 ),
 ( #30946, #8025, #28437, #3044, #11808, #9119, #12296 ),
 ( #11989, #1968, #27362, #32238, #17152, #7293, #9618 ),
 ( #1804, #14962, #1615, #9302, #29867, #27181, #11640 ),
 ( #19518, #16981, #9806, #22016, #32551, #12139, #4479 ),
 ( #6794, #29714, #20027, #25176, #32048, #6950, #22509 ),
 ( #9457, #14653, #4786, #19349, #22339, #27531, #24496 ),
 ( #4287, #19674, #14462, #24850, #24678, #22187, #19843 ) ),
 .UNSPECIFIED., .F., .F., .F.,
 ( 4, 3, 3, 3, 3, 3, 3, 3, 3, 3, 3, 4 ),
 ( 4, 3, 4 ),
 ( -1.834560091635544504E-11, 0.001953124981690232886, 0.003906249981726066852, 0.007812499981797734784, 0.01562499998194107065, 0.03124999998222774064, 0.06249999998280108410, 0.1249999999839477710, 0.2499999999862411448, 0.4999999999908278925, 0.7499999999954145569, 1.000000000000001332 ),
 ( 0.003589107913150553671, 0.5017945539565752400, 1.000000000000000000 ),
 .UNSPECIFIED. ) ;
#13716 = CARTESIAN_POINT ( 'NONE',  ( 3.499999999999999556, -6.700937042937042065, -2.183447440113257976 ) ) ;
#13717 = CARTESIAN_POINT ( 'NONE',  ( -6.637550801365594388, -1.088641768524163389, -3.675193018007246071 ) ) ;
#13718 = ORIENTED_EDGE ( 'NONE', *, *, #1799, .F. ) ;
#13719 = EDGE_CURVE ( 'NONE', #9887, #2902, #24907, .T. ) ;
#13720 = CARTESIAN_POINT ( 'NONE',  ( 3.499999999999999556, 0.000000000000000000, 0.000000000000000000 ) ) ;
#13721 = EDGE_CURVE ( 'NONE', #23931, #24941, #2970, .T. ) ;
#13722 = CARTESIAN_POINT ( 'NONE',  ( 2.970200448035948959, 8.521880193026294847, -3.362738345043123633 ) ) ;
#13724 = CARTESIAN_POINT ( 'NONE',  ( 107.9478747612858882, -17.31877164626198251, 4.502019023796631103 ) ) ;
#13723 = DIRECTION ( 'NONE',  ( -1.000000000000000000, 8.574039729943019576E-17, -0.000000000000000000 ) ) ;
#13725 = EDGE_LOOP ( 'NONE', ( #29305, #14348, #13310, #8210 ) ) ;
#13726 = CARTESIAN_POINT ( 'NONE',  ( 26.08945412691625521, 19.05746434167071612, 1.050000000000000044 ) ) ;
#13727 = VERTEX_POINT ( 'NONE', #6847 ) ;
#13728 = CARTESIAN_POINT ( 'NONE',  ( 10.57125986779756843, -4.681538312723512618, -0.8254815157535732029 ) ) ;
#13730 = ORIENTED_EDGE ( 'NONE', *, *, #7486, .T. ) ;
#13729 = CARTESIAN_POINT ( 'NONE',  ( 24.35832023931602208, -17.33818253687209676, 1.317734466820223549 ) ) ;
#13731 = ORIENTED_EDGE ( 'NONE', *, *, #9329, .F. ) ;
#13732 = CARTESIAN_POINT ( 'NONE',  ( 0.000000000000000000, 0.000000000000000000, 0.000000000000000000 ) ) ;
#13733 = DIRECTION ( 'NONE',  ( 0.000000000000000000, 0.000000000000000000, 1.000000000000000000 ) ) ;
#13735 = ORIENTED_EDGE ( 'NONE', *, *, #25283, .F. ) ;
#13734 = CARTESIAN_POINT ( 'NONE',  ( 107.8265053079015559, 17.21207302154092389, 2.264765925274638825 ) ) ;
#13736 = FACE_OUTER_BOUND ( 'NONE', #28305, .T. ) ;
#13737 = CARTESIAN_POINT ( 'NONE',  ( -56.28351068136514357, 0.000000000000000000, -1.000000000000000000 ) ) ;
#13738 = CYLINDRICAL_SURFACE ( 'NONE', #4903, 11.00000000000000000 ) ;
#13739 = CARTESIAN_POINT ( 'NONE',  ( 13.44509804349893933, -13.81913516303328393, -1.000000000000000000 ) ) ;
#13740 = CARTESIAN_POINT ( 'NONE',  ( 107.9809898003504003, -17.79561997080629254, -4.354661406389237044 ) ) ;
#13741 = DIRECTION ( 'NONE',  ( 0.000000000000000000, 0.000000000000000000, 1.000000000000000000 ) ) ;
#13742 = LINE ( 'NONE', #11088, #16270 ) ;
#13743 = DIRECTION ( 'NONE',  ( 1.000000000000000000, -0.000000000000000000, -0.000000000000000000 ) ) ;
#13744 = CARTESIAN_POINT ( 'NONE',  ( 3.238981242682539285, 0.6371288015966363183, 1.059614580210928025 ) ) ;
#13745 = ORIENTED_EDGE ( 'NONE', *, *, #26538, .T. ) ;
#13746 = CARTESIAN_POINT ( 'NONE',  ( 18.80941384712784981, -5.307593421039076276, 3.636029349014984202 ) ) ;
#13747 = CARTESIAN_POINT ( 'NONE',  ( -41.77414131929176477, -16.18685544166627821, 1.500000000000000000 ) ) ;
#13748 = EDGE_CURVE ( 'NONE', #545, #17553, #4358, .T. ) ;
#13749 = CARTESIAN_POINT ( 'NONE',  ( 13.62547635268492385, 21.94000000000003681, -1.081064828084696394 ) ) ;
#13750 = VERTEX_POINT ( 'NONE', #20083 ) ;
#13751 = EDGE_CURVE ( 'NONE', #27641, #3086, #22243, .T. ) ;
#13752 = EDGE_CURVE ( 'NONE', #24941, #32892, #26431, .T. ) ;
#13753 = CARTESIAN_POINT ( 'NONE',  ( -15.02135460118491217, -25.93932300454937945, 1.095404497688272638 ) ) ;
#13754 = CARTESIAN_POINT ( 'NONE',  ( 21.39621122230721539, -21.77804412735442696, -1.397661460514420195 ) ) ;
#13755 = ORIENTED_EDGE ( 'NONE', *, *, #22697, .F. ) ;
#13756 = CARTESIAN_POINT ( 'NONE',  ( 14.72442999747527637, -15.74550703336688784, -1.499999999999999334 ) ) ;
#13757 =( NAMED_UNIT ( * ) PLANE_ANGLE_UNIT ( ) SI_UNIT ( $, .RADIAN. ) );
#13758 = ORIENTED_EDGE ( 'NONE', *, *, #4240, .F. ) ;
#13759 = VERTEX_POINT ( 'NONE', #22394 ) ;
#13760 = LINE ( 'NONE', #31847, #31103 ) ;
#13761 = CALENDAR_DATE ( 2026, 6, 10 ) ;
#13763 = VERTEX_POINT ( 'NONE', #24558 ) ;
#13762 = DIRECTION ( 'NONE',  ( 0.000000000000000000, 1.000000000000000000, 0.000000000000000000 ) ) ;
#13764 = ORIENTED_EDGE ( 'NONE', *, *, #3502, .F. ) ;
#13765 = DIRECTION ( 'NONE',  ( 0.000000000000000000, -0.000000000000000000, -1.000000000000000000 ) ) ;
#13767 = ORIENTED_EDGE ( 'NONE', *, *, #27535, .F. ) ;
#13766 = B_SPLINE_CURVE_WITH_KNOTS ( 'NONE', 3,
 ( #23326, #26010, #7793, #8287, #18480, #13271, #5276, #12772, #101, #17822 ),
 .UNSPECIFIED., .F., .F.,
 ( 4, 2, 2, 2, 4 ),
 ( 0.000000000000000000, 0.0003410363541725900923, 0.0006820727083451801846, 0.001023109062517770385, 0.001364145416690360369 ),
 .UNSPECIFIED. ) ;
#13768 = CARTESIAN_POINT ( 'NONE',  ( 71.84273455769063332, -21.42499078636442178, 4.522129901861158707 ) ) ;
#13769 = CARTESIAN_POINT ( 'NONE',  ( 7.249760686538667009, -0.8180878109962448352, 8.711672189281424394 ) ) ;
#13771 = ORIENTED_EDGE ( 'NONE', *, *, #10494, .F. ) ;
#13770 = FACE_OUTER_BOUND ( 'NONE', #3878, .T. ) ;
#13772 = CARTESIAN_POINT ( 'NONE',  ( 0.000000000000000000, 0.000000000000000000, 0.000000000000000000 ) ) ;
#13773 = CARTESIAN_POINT ( 'NONE',  ( 34.99999999999998579, 0.5174497483512504603, 2.981930256614502284 ) ) ;
#13774 = CARTESIAN_POINT ( 'NONE',  ( -34.48223484310472742, 0.5000000000000000000, -2.482234843104710986 ) ) ;
#13775 = FACE_OUTER_BOUND ( 'NONE', #2016, .T. ) ;
#13776 = CARTESIAN_POINT ( 'NONE',  ( 10.00000000000000000, 4.208382051008230818, -2.718385644597129502 ) ) ;
#13777 = CARTESIAN_POINT ( 'NONE',  ( 35.27024661284173845, -8.402227462205928532, -0.07017451552783472712 ) ) ;
#13778 = DIRECTION ( 'NONE',  ( -0.9960221812693187404, 0.08910563629484180570, 0.000000000000000000 ) ) ;
#13779 = EDGE_CURVE ( 'NONE', #6331, #2424, #17394, .T. ) ;
#13780 = DIRECTION ( 'NONE',  ( 0.000000000000000000, -0.9271838545667854259, -0.3746065934159166777 ) ) ;
#13781 = FACE_OUTER_BOUND ( 'NONE', #8264, .T. ) ;
#13782 = CARTESIAN_POINT ( 'NONE',  ( 107.3476768466458253, -15.88628154573095586, -1.500000000000000000 ) ) ;
#13783 = LINE ( 'NONE', #9436, #19338 ) ;
#13784 = DIRECTION ( 'NONE',  ( -1.000000000000000000, 0.000000000000000000, -0.000000000000000000 ) ) ;
#13785 = CARTESIAN_POINT ( 'NONE',  ( -2.262550801365593056, 3.521866450007987037, 0.3701630799359328372 ) ) ;
#13786 = ORIENTED_EDGE ( 'NONE', *, *, #2673, .F. ) ;
#13787 = CARTESIAN_POINT ( 'NONE',  ( -6.200050800000000528, -1.887961173149512062, -2.331437884370912261 ) ) ;
#13788 = FACE_OUTER_BOUND ( 'NONE', #18761, .T. ) ;
#13789 = LINE ( 'NONE', #6139, #1252 ) ;
#13790 = CARTESIAN_POINT ( 'NONE',  ( 6.666829201526833337, -7.372062170298320005, 1.500000000000000000 ) ) ;
#13791 = VERTEX_POINT ( 'NONE', #14858 ) ;
#13792 = CARTESIAN_POINT ( 'NONE',  ( -59.84585868070823267, -5.753144558333701752, 1.500000000000000000 ) ) ;
#13793 = VERTEX_POINT ( 'NONE', #3499 ) ;
#13794 = CARTESIAN_POINT ( 'NONE',  ( 6.604407424131250259, -13.59569599788273031, 1.499999999999154898 ) ) ;
#13795 = APPROVAL_ROLE ( '' ) ;
#13796 = CARTESIAN_POINT ( 'NONE',  ( 54.94895328793697331, -5.485086176145982151, 4.155404937709241686 ) ) ;
#13797 = CARTESIAN_POINT ( 'NONE',  ( -6.112942406915326643, -3.366872799099910998E-15, -3.000000000000000000 ) ) ;
#13798 = CARTESIAN_POINT ( 'NONE',  ( 21.08401840680132011, -16.78474387324121153, -1.499999999999999556 ) ) ;
#13799 = FACE_OUTER_BOUND ( 'NONE', #7801, .T. ) ;
#13800 = B_SPLINE_CURVE_WITH_KNOTS ( 'NONE', 3,
 ( #4076, #31985, #14242, #22439, #29655, #9053, #17428, #6736, #16926, #11929 ),
 .UNSPECIFIED., .F., .F.,
 ( 4, 2, 2, 2, 4 ),
 ( 0.000000000000000000, 5.472672424563606967E-05, 0.0001094534484912721393, 0.0002189068969825542805, 0.0004378137939651184814 ),
 .UNSPECIFIED. ) ;
#13801 = ORIENTED_EDGE ( 'NONE', *, *, #5956, .T. ) ;
#13802 = ADVANCED_FACE ( 'NONE', ( #6150 ), #32239, .T. ) ;
#13803 = CARTESIAN_POINT ( 'NONE',  ( 6.524595126109737464, -8.397268106035227220, 2.112519041817586984 ) ) ;
#13804 = CARTESIAN_POINT ( 'NONE',  ( 10.56870887191539587, 1.476463073999635389, 4.787500056513372293 ) ) ;
#13805 = CARTESIAN_POINT ( 'NONE',  ( 3.063284526839887167, -4.729683950898817102, -7.360373001730970977 ) ) ;
#13807 = ORIENTED_EDGE ( 'NONE', *, *, #30929, .F. ) ;
#13806 = FACE_OUTER_BOUND ( 'NONE', #20595, .T. ) ;
#13808 = CARTESIAN_POINT ( 'NONE',  ( -2.812550801365592879, -1.828967928396026510, 3.368539882008728004 ) ) ;
#13809 = EDGE_CURVE ( 'NONE', #29918, #15750, #2408, .T. ) ;
#13810 = CARTESIAN_POINT ( 'NONE',  ( 18.60402535544292490, -7.603424548862588672, 0.07017451552782096036 ) ) ;
#13811 = DIRECTION ( 'NONE',  ( -1.000000000000000000, 0.000000000000000000, 0.000000000000000000 ) ) ;
#13812 = FACE_OUTER_BOUND ( 'NONE', #24075, .T. ) ;
#13813 = CARTESIAN_POINT ( 'NONE',  ( 3.499999999999999556, 4.137773741518377513, 5.705158055754806945 ) ) ;
#13814 = CARTESIAN_POINT ( 'NONE',  ( -56.28351068137280322, 0.000000000000000000, 4.148259000770580407 ) ) ;
#13815 = CARTESIAN_POINT ( 'NONE',  ( -2.786590204610741583, -5.640011313470056464, 4.522129901861159595 ) ) ;
#13816 = EDGE_CURVE ( 'NONE', #25039, #3168, #23839, .T. ) ;
#13817 = ADVANCED_FACE ( 'NONE', ( #19022 ), #16171, .T. ) ;
#13818 = CARTESIAN_POINT ( 'NONE',  ( 48.01729800609908949, -4.703650321867185902, 4.522129901861162260 ) ) ;
#13819 = ORIENTED_EDGE ( 'NONE', *, *, #10494, .T. ) ;
#13820 = CARTESIAN_POINT ( 'NONE',  ( 6.037141848526922594, 2.473100090966272813, -8.105561522824284992 ) ) ;
#13821 = B_SPLINE_CURVE_WITH_KNOTS ( 'NONE', 3,
 ( #15294, #30207, #20161, #12465, #283, #2100, #9791, #20321 ),
 .UNSPECIFIED., .F., .F.,
 ( 4, 2, 2, 4 ),
 ( 2.213836054398032120E-07, 0.001227982086136578848, 0.001841862437402149106, 0.002455742788667719147 ),
 .UNSPECIFIED. ) ;
#13822 = AXIS2_PLACEMENT_3D ( 'NONE', #13250, #21134, #11238 ) ;
#13823 = LINE ( 'NONE', #6483, #11857 ) ;
#13824 = CARTESIAN_POINT ( 'NONE',  ( -4.587550801365592790, -0.3701630799359326152, 3.521866450007987037 ) ) ;
#13825 = CARTESIAN_POINT ( 'NONE',  ( -42.85764933975779201, 24.74387538314362800, 1.050000000000000044 ) ) ;
#13826 = CARTESIAN_POINT ( 'NONE',  ( 102.5019105821284313, -5.123465467906984649, 2.184956770195073616 ) ) ;
#13827 = ORIENTED_EDGE ( 'NONE', *, *, #26053, .T. ) ;
#13828 = FACE_OUTER_BOUND ( 'NONE', #13162, .T. ) ;
#13829 = EDGE_CURVE ( 'NONE', #8819, #19834, #21835, .T. ) ;
#13830 = EDGE_CURVE ( 'NONE', #25011, #30361, #11323, .T. ) ;
#13831 = EDGE_LOOP ( 'NONE', ( #8004, #17535 ) ) ;
#13832 = APPLICATION_PROTOCOL_DEFINITION ( 'international standard', 'config_control_design', 1994, #29768 ) ;
#13833 = CARTESIAN_POINT ( 'NONE',  ( 3.063284526839887167, 0.000000000000000000, -8.749000000000004107 ) ) ;
#13834 = ADVANCED_FACE ( 'NONE', ( #29553 ), #31584, .F. ) ;
#13835 = CIRCLE ( 'NONE', #14921, 4.000000000000000888 ) ;
#13836 = CARTESIAN_POINT ( 'NONE',  ( 56.97280603064898941, -277.2763395528616002, 2.806473568333438084 ) ) ;
#13837 = ORIENTED_EDGE ( 'NONE', *, *, #9242, .T. ) ;
#13838 = DIRECTION ( 'NONE',  ( -0.000000000000000000, -0.000000000000000000, -1.000000000000000000 ) ) ;
#13839 = ORIENTED_EDGE ( 'NONE', *, *, #28744, .T. ) ;
#13840 = ORIENTED_EDGE ( 'NONE', *, *, #2731, .T. ) ;
#13841 = CARTESIAN_POINT ( 'NONE',  ( -1.170068671574743036, -6.059534462705075342, -4.522129901861164925 ) ) ;
#13842 = CARTESIAN_POINT ( 'NONE',  ( -4.912550801365593856, -1.088641768524163611, -3.675193018007245627 ) ) ;
#13843 = CARTESIAN_POINT ( 'NONE',  ( 22.48500000000000298, -2.486304738420683780, 0.2613211581691335383 ) ) ;
#13844 = CARTESIAN_POINT ( 'NONE',  ( 1.184589434306864364, -2.669489141080311434, -1.500000000000000222 ) ) ;
#13845 = CIRCLE ( 'NONE', #14930, 0.4999999999999995559 ) ;
#13846 =( BOUNDED_CURVE ( )  B_SPLINE_CURVE ( 2, ( #13592, #6574, #16771, #26970, #26625, #6384, #8569, #23944, #26483, #26323, #23797 ),
 .UNSPECIFIED., .F., .F. ) 
 B_SPLINE_CURVE_WITH_KNOTS ( ( 3, 2, 2, 2, 2, 3 ),
 ( 0.09661161918950035565, 0.1000000000000000056, 0.1250000000000000000, 0.1499999999999999944, 0.1749999999999999889, 0.1966116191895003751 ),
 .UNSPECIFIED. ) 
 CURVE ( )  GEOMETRIC_REPRESENTATION_ITEM ( )  RATIONAL_B_SPLINE_CURVE ( ( 0.9821626249036858880, 0.9896829947469992783, 1.000000000000000000, 0.9238795325112867385, 1.000000000000000000, 0.9238795325112867385, 1.000000000000000000, 0.9238795325112867385, 1.000000000000000000, 0.9341965377642874602, 0.9821626249036858880 ) ) 
 REPRESENTATION_ITEM ( '' )  );
#13848 = VERTEX_POINT ( 'NONE', #32552 ) ;
#13847 = DIRECTION ( 'NONE',  ( 1.000000000000000000, 0.000000000000000000, 0.000000000000000000 ) ) ;
#13849 = CARTESIAN_POINT ( 'NONE',  ( -5.887550801365593500, -2.228590825266444586, -2.752080473201636401 ) ) ;
#13850 = CARTESIAN_POINT ( 'NONE',  ( 19.54096706358707181, 15.62796595325201920, 1.500000000000000222 ) ) ;
#13851 = B_SPLINE_CURVE_WITH_KNOTS ( 'NONE', 3,
 ( #2468, #5287, #20827, #12785, #28536, #4969, #28344, #30373 ),
 .UNSPECIFIED., .F., .F.,
 ( 4, 2, 2, 4 ),
 ( 5.099451029780936180E-07, 0.001229189756360174034, 0.001843529661988772611, 0.002457869567617371187 ),
 .UNSPECIFIED. ) ;
#13852 = DIRECTION ( 'NONE',  ( 0.03488359650710505522, -0.9989355049964838695, -0.03018263660036221013 ) ) ;
#13853 = CARTESIAN_POINT ( 'NONE',  ( 10.56870887191539587, -1.946309384392561626, -4.616489984850551842 ) ) ;
#13855 = ORIENTED_EDGE ( 'NONE', *, *, #24252, .T. ) ;
#13854 = DIRECTION ( 'NONE',  ( 0.000000000000000000, 0.000000000000000000, -1.000000000000000000 ) ) ;
#13856 = CARTESIAN_POINT ( 'NONE',  ( 22.36000000273118715, 1.942864903642424146, 1.573300977624592534 ) ) ;
#13857 = ADVANCED_FACE ( 'NONE', ( #29715 ), #22487, .F. ) ;
#13858 = EDGE_CURVE ( 'NONE', #25356, #6749, #27683, .T. ) ;
#13859 = CARTESIAN_POINT ( 'NONE',  ( 5.377543748152548986, -1.391664247347174754, -7.892520144992448472 ) ) ;
#13860 = VECTOR ( 'NONE', #4025, 1000.000000000000000 ) ;
#13861 = DIRECTION ( 'NONE',  ( -1.000000000000000000, 0.000000000000000000, 0.000000000000000000 ) ) ;
#13862 = DIRECTION ( 'NONE',  ( -0.000000000000000000, -0.000000000000000000, -1.000000000000000000 ) ) ;
#13863 = CYLINDRICAL_SURFACE ( 'NONE', #26345, 4.000000000000001776 ) ;
#13864 = CIRCLE ( 'NONE', #4803, 8.999999999999998224 ) ;
#13865 = B_SPLINE_CURVE_WITH_KNOTS ( 'NONE', 3,
 ( #17691, #20067, #13023, #23229, #166, #22881, #33083, #20719 ),
 .UNSPECIFIED., .F., .F.,
 ( 4, 2, 2, 4 ),
 ( 2.851296420411806090E-07, 0.001262135616826462903, 0.001893060860418671653, 0.002523986104010880402 ),
 .UNSPECIFIED. ) ;
#13866 = FACE_BOUND ( 'NONE', #21923, .T. ) ;
#13867 = CARTESIAN_POINT ( 'NONE',  ( -1.959487840848880017E-16, -2.285372942704922306, -4.458382051008217495 ) ) ;
#13868 = ORIENTED_EDGE ( 'NONE', *, *, #17940, .T. ) ;
#13869 = VECTOR ( 'NONE', #15892, 1000.000000000000227 ) ;
#13870 = CARTESIAN_POINT ( 'NONE',  ( 17.33093461831347781, -21.43932300456618378, 1.499999999999999112 ) ) ;
#13871 = CARTESIAN_POINT ( 'NONE',  ( 0.000000000000000000, 1.418488851014406693, 6.085876303339381899 ) ) ;
#13873 = CARTESIAN_POINT ( 'NONE',  ( 24.01922593961334940, -17.30645187339506563, 1.384626276794619137 ) ) ;
#13872 = DIRECTION ( 'NONE',  ( 1.000000000000000000, -0.000000000000000000, -0.000000000000000000 ) ) ;
#13874 = ORIENTED_EDGE ( 'NONE', *, *, #2933, .T. ) ;
#13875 = ADVANCED_FACE ( 'NONE', ( #25003 ), #9619, .F. ) ;
#13876 = CC_DESIGN_PERSON_AND_ORGANIZATION_ASSIGNMENT ( #637, #6147, ( #15168 ) ) ;
#13877 = FACE_OUTER_BOUND ( 'NONE', #6374, .T. ) ;
#13878 = VERTEX_POINT ( 'NONE', #7143 ) ;
#13879 = CYLINDRICAL_SURFACE ( 'NONE', #26297, 11.00000000000000000 ) ;
#13881 = ORIENTED_EDGE ( 'NONE', *, *, #2953, .F. ) ;
#13880 = CARTESIAN_POINT ( 'NONE',  ( 84.96557803822885546, -4.058969597092461079, -3.993433529893592571 ) ) ;
#13882 = ORIENTED_EDGE ( 'NONE', *, *, #23198, .T. ) ;
#13883 = CARTESIAN_POINT ( 'NONE',  ( 10.55147673363119232, 2.718385644597172579, 4.208382051008202396 ) ) ;
#13884 = VECTOR ( 'NONE', #23453, 1000.000000000000000 ) ;
#13885 = CARTESIAN_POINT ( 'NONE',  ( 43.06800534735074137, -24.01680020629799728, -1.499999999999999556 ) ) ;
#13887 = EDGE_LOOP ( 'NONE', ( #23305, #23426, #5625, #21132 ) ) ;
#13886 = CARTESIAN_POINT ( 'NONE',  ( -2.558315521542159132, 0.4094970184090410137, -1.491740999229417941 ) ) ;
#13888 = DIRECTION ( 'NONE',  ( 0.000000000000000000, -0.9659258262890662028, -0.2588190451025286221 ) ) ;
#13889 = CIRCLE ( 'NONE', #27248, 0.4500000000000006772 ) ;
#13890 = CARTESIAN_POINT ( 'NONE',  ( 12.23764924856644143, -13.51220073293806223, -1.000000000000000000 ) ) ;
#13891 = CARTESIAN_POINT ( 'NONE',  ( -23.54713438637982748, 10.71031731502107576, 2.573304945315896042 ) ) ;
#13893 = CARTESIAN_POINT ( 'NONE',  ( 8.789577373537829530, -11.69574158658589091, -1.500000000000000000 ) ) ;
#13892 = CIRCLE ( 'NONE', #19794, 6.035938585833444670 ) ;
#13894 = CARTESIAN_POINT ( 'NONE',  ( 107.9755271014895754, -17.71695846615960335, -4.186189698420959004 ) ) ;
#13895 = CARTESIAN_POINT ( 'NONE',  ( -4.800050802731187005, -3.113457007523259268, 0.9222479816126455399 ) ) ;
#13896 = EDGE_CURVE ( 'NONE', #28781, #2837, #1969, .T. ) ;
#13897 = VECTOR ( 'NONE', #19932, 1000.000000000000114 ) ;
#13898 = CARTESIAN_POINT ( 'NONE',  ( 3.063284526846069777, -2.223716399039799452, 8.461683424479977234 ) ) ;
#13899 = DIRECTION ( 'NONE',  ( 0.000000000000000000, 0.000000000000000000, 1.000000000000000000 ) ) ;
#13900 = CARTESIAN_POINT ( 'NONE',  ( 7.249760686538667009, 8.437262856154164936, 2.318425219014256911 ) ) ;
#13901 = DIRECTION ( 'NONE',  ( 1.000000000000000000, -0.000000000000000000, -0.000000000000000000 ) ) ;
#13902 = ORIENTED_EDGE ( 'NONE', *, *, #28245, .T. ) ;
#13903 = DIRECTION ( 'NONE',  ( 0.000000000000000000, 0.000000000000000000, 1.000000000000000000 ) ) ;
#13904 = AXIS2_PLACEMENT_3D ( 'NONE', #793, #10972, #7193 ) ;
#13905 = CIRCLE ( 'NONE', #14433, 10.99999999999999822 ) ;
#13906 = CARTESIAN_POINT ( 'NONE',  ( 8.886976913778035225, 2.271465516421274549E-16, -1.168311665897499463 ) ) ;
#13907 = CARTESIAN_POINT ( 'NONE',  ( -8.000050800000002127, 3.541248556864417196, 0.01107501445590582979 ) ) ;
#13908 = ORIENTED_EDGE ( 'NONE', *, *, #6293, .F. ) ;
#13909 = CIRCLE ( 'NONE', #26747, 2.999999999999999556 ) ;
#13910 = AXIS2_PLACEMENT_3D ( 'NONE', #17524, #7842, #7490 ) ;
#13911 = CARTESIAN_POINT ( 'NONE',  ( -15.35000000000000320, -10.96966150227469505, 4.500000000000000888 ) ) ;
#13912 = CARTESIAN_POINT ( 'NONE',  ( 47.40009415622113664, 24.02318594975524491, -5.396302277755718357 ) ) ;
#13913 = EDGE_LOOP ( 'NONE', ( #18139, #11818, #19626, #12632 ) ) ;
#13914 = CARTESIAN_POINT ( 'NONE',  ( 10.52034268205830259, -3.055657119358826446, 3.641590349731918863 ) ) ;
#13915 = EDGE_LOOP ( 'NONE', ( #22447, #20848, #1168, #18005, #14603, #16023, #407, #3862, #3271, #28649, #25508, #23343, #2792, #17921, #24037, #15309, #23463, #19089, #3804, #22951, #7383, #10015, #13208, #599, #29745, #28517, #9344, #10762, #16875, #17600, #13543, #28289, #12743, #11148, #20710, #18592, #14770, #5820, #7145, #31367, #8400, #4097, #29320, #25904, #31851, #1694, #22301, #26169, #1116, #32580, #17383, #25975, #11305, #24227, #23274, #14505, #32125, #30583, #26296, #17950, #13006, #17956, #26669, #32646, #21063, #31696, #28292, #20561, #13700, #26464, #27852, #14943, #30029, #12723, #31144, #2747, #20641, #23850, #4239, #5883, #22869, #18818, #28966, #6913, #18518, #19112, #32855, #11073, #5910, #5600, #29976, #16642, #31938, #27047, #20289, #14267, #25258, #13663, #24577, #22676, #5547, #20273, #23535, #7942, #32940, #25728, #24353, #16822 ) ) ;
#13916 = AXIS2_PLACEMENT_3D ( 'NONE', #22838, #7802, #5129 ) ;
#13917 = EDGE_LOOP ( 'NONE', ( #28599, #5356, #31617, #32168 ) ) ;
#13918 = CARTESIAN_POINT ( 'NONE',  ( 19.03654924710324181, -2.768675503676409466, -2.713652344655540727 ) ) ;
#13920 = ORIENTED_EDGE ( 'NONE', *, *, #17491, .F. ) ;
#13919 = CARTESIAN_POINT ( 'NONE',  ( 8.007433738499996068, 15.00000000000000000, 5.412820279296878923 ) ) ;
#13921 = ORIENTED_EDGE ( 'NONE', *, *, #26018, .F. ) ;
#13922 = CARTESIAN_POINT ( 'NONE',  ( 25.23500000136559507, -1.570731468192933633, -2.892927487894330962 ) ) ;
#13923 = ORIENTED_EDGE ( 'NONE', *, *, #27133, .F. ) ;
#13924 = CARTESIAN_POINT ( 'NONE',  ( 0.3285611067768013926, -13.34342412962908497, 4.522129901861158707 ) ) ;
#13925 = DIRECTION ( 'NONE',  ( 1.000000000000000000, -2.473959037481237219E-13, 0.000000000000000000 ) ) ;
#13927 = ORIENTED_EDGE ( 'NONE', *, *, #21218, .T. ) ;
#13926 = CARTESIAN_POINT ( 'NONE',  ( 41.34386496146469625, -3.886814715719084656, -0.4367667078930305147 ) ) ;
#13928 = FACE_OUTER_BOUND ( 'NONE', #31113, .T. ) ;
#13929 = DIRECTION ( 'NONE',  ( 1.000000000000000000, -3.469446951953588156E-15, 1.053584095796274567E-14 ) ) ;
#13930 = VECTOR ( 'NONE', #22483, 1000.000000000000000 ) ;
#13931 = EDGE_CURVE ( 'NONE', #26262, #3931, #10736, .T. ) ;
#13932 = DIRECTION ( 'NONE',  ( -1.000000000000000000, 0.000000000000000000, -0.000000000000000000 ) ) ;
#13933 = CARTESIAN_POINT ( 'NONE',  ( 2.795120501770171018, 5.116149273379854812, -8.308193303472245717 ) ) ;
#13934 = ADVANCED_FACE ( 'NONE', ( #30053 ), #16596, .F. ) ;
#13935 = AXIS2_PLACEMENT_3D ( 'NONE', #754, #5752, #15930 ) ;
#13936 = CARTESIAN_POINT ( 'NONE',  ( 108.0288187330202732, -18.48434470291169873, 4.339809795830553263 ) ) ;
#13937 = CIRCLE ( 'NONE', #4357, 10.94895958125474245 ) ;
#13938 = ADVANCED_FACE ( 'NONE', ( #6795 ), #22340, .T. ) ;
#13939 = CARTESIAN_POINT ( 'NONE',  ( 3.554613218822866738, -15.76807188677689275, -4.522129901861166701 ) ) ;
#13940 = CARTESIAN_POINT ( 'NONE',  ( 18.60402535544292490, -7.603424548862588672, -0.07017451552783671165 ) ) ;
#13941 = DIRECTION ( 'NONE',  ( 0.000000000000000000, 0.000000000000000000, -1.000000000000000000 ) ) ;
#13942 = CONICAL_SURFACE ( 'NONE', #18241, 2.524999999999999911, 0.7853981633974627119 ) ;
#13943 = VECTOR ( 'NONE', #26462, 1000.000000000000000 ) ;
#13944 = AXIS2_PLACEMENT_3D ( 'NONE', #29554, #6151, #18860 ) ;
#13945 = DIRECTION ( 'NONE',  ( -0.000000000000000000, 0.000000000000000000, 1.000000000000000000 ) ) ;
#13946 = FACE_OUTER_BOUND ( 'NONE', #15315, .T. ) ;
#13947 = LINE ( 'NONE', #9733, #7616 ) ;
#13948 = CARTESIAN_POINT ( 'NONE',  ( 7.249760686538667009, 7.135485519862069914, -5.064320921489747995 ) ) ;
#13949 = CARTESIAN_POINT ( 'NONE',  ( 21.67249999999999943, -1.291182301015472600, -2.378061970571982098 ) ) ;
#13950 = CARTESIAN_POINT ( 'NONE',  ( -4.850050802731186828, -2.331437884370912705, 1.887961173149512062 ) ) ;
#13951 = ORIENTED_EDGE ( 'NONE', *, *, #26274, .F. ) ;
#13952 = CARTESIAN_POINT ( 'NONE',  ( -5.050050800000001061, 2.853674364686379583, 1.549418761218565921 ) ) ;
#13953 = CIRCLE ( 'NONE', #21972, 2.999999999999999112 ) ;
#13954 = CARTESIAN_POINT ( 'NONE',  ( 108.1721831928535806, 19.13694388309671623, 4.863130064418045961 ) ) ;
#13955 = DIRECTION ( 'NONE',  ( 0.000000000000000000, 0.000000000000000000, 1.000000000000000000 ) ) ;
#13956 = CARTESIAN_POINT ( 'NONE',  ( 8.845957756505406167, -0.9823800962678642668, 1.000000000000000000 ) ) ;
#13957 = ORIENTED_EDGE ( 'NONE', *, *, #21383, .F. ) ;
#13958 = CARTESIAN_POINT ( 'NONE',  ( -7.000050800000001239, -1.887961173149512062, -2.331437884370912261 ) ) ;
#13959 = VECTOR ( 'NONE', #21852, 1000.000000000000000 ) ;
#13960 = CONICAL_SURFACE ( 'NONE', #9171, 3.024999999999999911, 0.7853981633974520538 ) ;
#13961 = ORIENTED_EDGE ( 'NONE', *, *, #16319, .T. ) ;
#13962 = CARTESIAN_POINT ( 'NONE',  ( 0.3143644610611543433, -7.550156354830646954, 1.500000000000071720 ) ) ;
#13963 = PERSON_AND_ORGANIZATION ( #6766, #25292 ) ;
#13964 = ORIENTED_EDGE ( 'NONE', *, *, #29281, .F. ) ;
#13965 = CARTESIAN_POINT ( 'NONE',  ( 40.88276903860496247, -6.671230418110412508, 4.215290092866328386 ) ) ;
#13966 = VECTOR ( 'NONE', #12700, 1000.000000000000114 ) ;
#13967 = VECTOR ( 'NONE', #3935, 999.9999999999998863 ) ;
#13968 = CYLINDRICAL_SURFACE ( 'NONE', #1100, 2.999999999999999112 ) ;
#13969 = CARTESIAN_POINT ( 'NONE',  ( 40.87824777906663343, -5.842713490123291109, -4.112224033464637607 ) ) ;
#13970 = CARTESIAN_POINT ( 'NONE',  ( 23.02255580926556178, -17.31849206757231840, -1.529834177132233686 ) ) ;
#13972 = CARTESIAN_POINT ( 'NONE',  ( 2.437082530871053532, 5.244446742619491175, 9.289394354155787070 ) ) ;
#13971 = B_SPLINE_CURVE_WITH_KNOTS ( 'NONE', 3,
 ( #15370, #28244, #15036, #27746, #198, #28098 ),
 .UNSPECIFIED., .F., .F.,
 ( 4, 2, 4 ),
 ( 0.009541643435016610234, 0.5047708217175083112, 1.000000000000000000 ),
 .UNSPECIFIED. ) ;
#13973 = EDGE_LOOP ( 'NONE', ( #9567, #9215, #29950, #460 ) ) ;
#13974 = EDGE_CURVE ( 'NONE', #10113, #22357, #1921, .T. ) ;
#13975 = EDGE_CURVE ( 'NONE', #17287, #6932, #3265, .T. ) ;
#13976 = CARTESIAN_POINT ( 'NONE',  ( 9.031711214211203043, 0.01997115109544704906, 1.016156546702292829 ) ) ;
#13977 = CARTESIAN_POINT ( 'NONE',  ( 107.6567828190203215, 16.56237727417163796, 1.453690251525116217 ) ) ;
#13978 = CARTESIAN_POINT ( 'NONE',  ( 18.89383689343546280, -4.363913198432375573, -3.393559380852849028 ) ) ;
#13979 = EDGE_CURVE ( 'NONE', #21819, #6075, #12638, .T. ) ;
#13981 = ORIENTED_EDGE ( 'NONE', *, *, #25725, .T. ) ;
#13980 = PLANE ( 'NONE',  #30467 ) ;
#13982 = AXIS2_PLACEMENT_3D ( 'NONE', #1764, #25590, #25273 ) ;
#13983 = CARTESIAN_POINT ( 'NONE',  ( -4.462550801365592790, -0.3701630799359326152, 3.521866450007987037 ) ) ;
#13984 = B_SPLINE_SURFACE_WITH_KNOTS ( 'NONE', 1, 3, ( 
 ( #4831, #7338, #10355, #5174, #2663, #25233, #32599, #27418, #32780, #17382, #22884, #33088, #2162, #25402, #27576, #10009 ),
 ( #12833, #30604, #9671, #19899, #20566, #4524, #24897, #23048, #172, #17212, #7686, #30113, #20220, #30415, #4675, #14845 ),
 ( #25044, #9858, #5022, #15200, #2512, #27722, #2353, #12528, #22735, #13321, #8334, #30922, #28400, #16181, #31087, #8480 ) ),
 .UNSPECIFIED., .F., .F., .F.,
 ( 2, 1, 2 ),
 ( 4, 2, 2, 2, 2, 2, 2, 4 ),
 ( 0.000000000000000000, 1.000000000000000000, 1.172438907768402538 ),
 ( 0.000000000000000000, 0.5000000000000000000, 0.6250000000000000000, 0.7500000000000000000, 0.8125000000000000000, 0.8750000000000000000, 0.9375000000000000000, 1.000000000000000000 ),
 .UNSPECIFIED. ) ;
#13985 = AXIS2_PLACEMENT_3D ( 'NONE', #30171, #26977, #1559 ) ;
#13986 = CARTESIAN_POINT ( 'NONE',  ( 10.56870887191539587, 1.946309384392654218, -4.616489984850511874 ) ) ;
#13987 = DIRECTION ( 'NONE',  ( 0.000000000000000000, 0.000000000000000000, 1.000000000000000000 ) ) ;
#13988 = CARTESIAN_POINT ( 'NONE',  ( 2.661997913519430714, -2.255009087902858589, -9.876677602395409039 ) ) ;
#13989 = DIRECTION ( 'NONE',  ( 1.000000000000000000, 0.000000000000000000, 0.000000000000000000 ) ) ;
#13990 = AXIS2_PLACEMENT_3D ( 'NONE', #24869, #19036, #21853 ) ;
#13991 = CIRCLE ( 'NONE', #21486, 4.000000000000001776 ) ;
#13992 = VECTOR ( 'NONE', #7558, 1000.000000000000227 ) ;
#13993 = CARTESIAN_POINT ( 'NONE',  ( 17.75999999999999801, -2.208672634433321348E-15, 0.000000000000000000 ) ) ;
#13994 = DIRECTION ( 'NONE',  ( 0.000000000000000000, 0.000000000000000000, -1.000000000000000000 ) ) ;
#13995 = CARTESIAN_POINT ( 'NONE',  ( 10.56870887191539587, -1.625881193364669297, -4.467071865485488402 ) ) ;
#13996 = CARTESIAN_POINT ( 'NONE',  ( 0.3285611067768007265, -13.34342412962908853, 4.522129901861159595 ) ) ;
#13997 = ORIENTED_EDGE ( 'NONE', *, *, #5186, .F. ) ;
#13998 = CIRCLE ( 'NONE', #7074, 2.999999999999999112 ) ;
#13999 = CYLINDRICAL_SURFACE ( 'NONE', #25255, 4.000000000000001776 ) ;
#14000 = VERTEX_POINT ( 'NONE', #33044 ) ;
#14001 = AXIS2_PLACEMENT_3D ( 'NONE', #3534, #23893, #6183 ) ;
#14002 = CARTESIAN_POINT ( 'NONE',  ( 2.619288827430985567, 0.4094970184090461762, -1.491740999229418829 ) ) ;
#14003 = CARTESIAN_POINT ( 'NONE',  ( -1.981386825810575125, 0.8521285013611177295, 3.209918541081830945 ) ) ;
#14004 = CARTESIAN_POINT ( 'NONE',  ( -4.137550801365593500, 1.828967928396027398, -3.368539882008727115 ) ) ;
#14005 = PLANE ( 'NONE',  #10315 ) ;
#14006 = CARTESIAN_POINT ( 'NONE',  ( 18.64064227445971866, -7.194120883405200395, 1.873789191074036964 ) ) ;
#14007 = VERTEX_POINT ( 'NONE', #10118 ) ;
#14008 = DIRECTION ( 'NONE',  ( 1.000000000000000000, -8.574039729943018344E-17, -0.000000000000000000 ) ) ;
#14009 = AXIS2_PLACEMENT_3D ( 'NONE', #24386, #1354, #32594 ) ;
#14010 = AXIS2_PLACEMENT_3D ( 'NONE', #23230, #5330, #8333 ) ;
#14012 = EDGE_CURVE ( 'NONE', #8919, #29952, #32732, .T. ) ;
#14011 = VERTEX_POINT ( 'NONE', #7445 ) ;
#14014 = CIRCLE ( 'NONE', #19362, 8.749000000000002331 ) ;
#14013 = DATE_AND_TIME ( #14506, #3426 ) ;
#14015 = CARTESIAN_POINT ( 'NONE',  ( 2.143509932485593732E-17, 0.2499999999999817368, 5.003758587302149508 ) ) ;
#14016 = CIRCLE ( 'NONE', #30071, 4.000000000000001776 ) ;
#14017 = VECTOR ( 'NONE', #23729, 1000.000000000000000 ) ;
#14018 = VECTOR ( 'NONE', #32616, 1000.000000000000000 ) ;
#14019 = EDGE_CURVE ( 'NONE', #1268, #228, #7294, .T. ) ;
#14020 = CARTESIAN_POINT ( 'NONE',  ( -10.00000000000000000, 0.000000000000000000, 0.000000000000000000 ) ) ;
#14021 = EDGE_LOOP ( 'NONE', ( #33089, #17599, #31036, #12183 ) ) ;
#14022 = CARTESIAN_POINT ( 'NONE',  ( 5.561021557437512364, 7.493231324518997205, 2.854557343487603038 ) ) ;
#14023 = ORIENTED_EDGE ( 'NONE', *, *, #12194, .F. ) ;
#14024 = ORIENTED_EDGE ( 'NONE', *, *, #11032, .F. ) ;
#14025 = FACE_OUTER_BOUND ( 'NONE', #2584, .T. ) ;
#14026 = CARTESIAN_POINT ( 'NONE',  ( -5.412550801365593856, 3.368539882008727115, 1.828967928396027176 ) ) ;
#14027 = CARTESIAN_POINT ( 'NONE',  ( 24.10999999999999943, 1.942864903642424146, 1.573300977624592534 ) ) ;
#14028 = DIRECTION ( 'NONE',  ( -1.000000000000000000, 0.000000000000000000, 0.000000000000000000 ) ) ;
#14030 = ORIENTED_EDGE ( 'NONE', *, *, #2240, .T. ) ;
#14029 = CARTESIAN_POINT ( 'NONE',  ( 0.000000000000000000, 0.000000000000000000, 0.000000000000000000 ) ) ;
#14031 = CARTESIAN_POINT ( 'NONE',  ( -5.737550801365594033, 1.828967928396027176, -3.368539882008727115 ) ) ;
#14032 = CARTESIAN_POINT ( 'NONE',  ( 107.7704431822035076, 16.89989698459580225, -1.579319589807283819 ) ) ;
#14033 = EDGE_CURVE ( 'NONE', #24488, #16352, #7920, .T. ) ;
#14034 = FACE_OUTER_BOUND ( 'NONE', #17430, .T. ) ;
#14035 = CARTESIAN_POINT ( 'NONE',  ( 3.249999999999999556, 0.000000000000000000, 0.000000000000000000 ) ) ;
#14036 = EDGE_LOOP ( 'NONE', ( #25377, #7249, #13379, #12711, #19291 ) ) ;
#14038 = ORIENTED_EDGE ( 'NONE', *, *, #1584, .T. ) ;
#14037 = CARTESIAN_POINT ( 'NONE',  ( -59.84585868070823267, -5.753144558333704417, 1.949999999999999734 ) ) ;
#14039 = AXIS2_PLACEMENT_3D ( 'NONE', #24975, #24637, #17114 ) ;
#14040 = AXIS2_PLACEMENT_3D ( 'NONE', #19009, #32844, #13955 ) ;
#14041 = CARTESIAN_POINT ( 'NONE',  ( 23.36000000273119070, 1.942864903642424146, 1.573300977624592534 ) ) ;
#14042 = ADVANCED_FACE ( 'NONE', ( #22188 ), #19675, .T. ) ;
#14043 = VECTOR ( 'NONE', #27207, 1000.000000000000000 ) ;
#14044 = AXIS2_PLACEMENT_3D ( 'NONE', #2143, #17511, #14829 ) ;
#14045 = CARTESIAN_POINT ( 'NONE',  ( 25.75999999999999801, -2.208672634433321348E-15, -3.024999999999999911 ) ) ;
#14046 = AXIS2_PLACEMENT_3D ( 'NONE', #21549, #16349, #18539 ) ;
#14047 = CARTESIAN_POINT ( 'NONE',  ( -27.13750370379022314, 17.93667199020026715, 1.500000000000000000 ) ) ;
#14048 = CARTESIAN_POINT ( 'NONE',  ( -4.433175167559320506, -8.339139981106209021, -1.500000000000000000 ) ) ;
#14049 = CARTESIAN_POINT ( 'NONE',  ( 3.249999999999999556, 9.314797388894893615, 1.239665997526919972 ) ) ;
#14050 = AXIS2_PLACEMENT_3D ( 'NONE', #30943, #684, #28601 ) ;
#14051 = SECURITY_CLASSIFICATION ( '', '', #11521 ) ;
#14052 = LINE ( 'NONE', #18930, #12955 ) ;
#14053 = CARTESIAN_POINT ( 'NONE',  ( -3.037550801365593411, 1.088641768524161613, 3.675193018007247403 ) ) ;
#14054 = CARTESIAN_POINT ( 'NONE',  ( 101.7091070155185690, -2.709697044720575931, 3.690548917384798955 ) ) ;
#14055 = ORIENTED_EDGE ( 'NONE', *, *, #22335, .F. ) ;
#14056 = EDGE_CURVE ( 'NONE', #31304, #6067, #20664, .T. ) ;
#14057 = CARTESIAN_POINT ( 'NONE',  ( 21.02910828058395865, -21.78322936331010595, 1.363801422436717870 ) ) ;
#14058 = ADVANCED_FACE ( 'NONE', ( #7956 ), #5316, .T. ) ;
#14059 = CARTESIAN_POINT ( 'NONE',  ( -29.23615344119660264, -25.43932300454937945, 11.04051477514566315 ) ) ;
#14061 = CARTESIAN_POINT ( 'NONE',  ( 107.9480651260689967, -17.32151285178439437, 4.509510090909671476 ) ) ;
#14060 = LINE ( 'NONE', #18936, #28907 ) ;
#14062 = EDGE_LOOP ( 'NONE', ( #8720, #19118, #29160, #27398 ) ) ;
#14063 =( BOUNDED_SURFACE ( )  B_SPLINE_SURFACE ( 3, 3, ( 
 ( #23512, #21190, #31728, #26200 ),
 ( #8463, #23992, #13480, #5653 ),
 ( #18660, #31542, #20851, #3487 ),
 ( #8804, #1299, #8152, #26043 ) ),
 .UNSPECIFIED., .F., .F., .F. ) 
 B_SPLINE_SURFACE_WITH_KNOTS ( ( 4, 4 ),
 ( 4, 4 ),
 ( 0.000000000000000000, 1.000000000000000000 ),
 ( 0.000000000000000000, 1.000000000000000000 ),
 .UNSPECIFIED. ) 
 GEOMETRIC_REPRESENTATION_ITEM ( )  RATIONAL_B_SPLINE_SURFACE ( (
 ( 1.000000000000000000, 0.9321687722090974404, 0.9321687722090974404, 1.000000000000000000),
 ( 0.6539698177806696489, 0.6096102421024139906, 0.6096102421024139906, 0.6539698177806696489),
 ( 0.6539698177806696489, 0.6096102421024139906, 0.6096102421024139906, 0.6539698177806696489),
 ( 1.000000000000000000, 0.9321687722090974404, 0.9321687722090974404, 1.000000000000000000) ) ) 
 REPRESENTATION_ITEM ( '' )  SURFACE ( )  );
#14064 = VECTOR ( 'NONE', #20650, 1000.000000000000000 ) ;
#14065 = CARTESIAN_POINT ( 'NONE',  ( 3.499999999999999556, -1.179494851233859887, -6.136676046192499179 ) ) ;
#14066 = ORIENTED_EDGE ( 'NONE', *, *, #613, .F. ) ;
#14067 = DIRECTION ( 'NONE',  ( -1.000000000000000000, 0.000000000000000000, 0.000000000000000000 ) ) ;
#14069 = ORIENTED_EDGE ( 'NONE', *, *, #20596, .T. ) ;
#14068 = CARTESIAN_POINT ( 'NONE',  ( 18.86054332783762177, -4.736068442332642903, -3.993434335991318473 ) ) ;
#14070 = ORIENTED_EDGE ( 'NONE', *, *, #6890, .T. ) ;
#14071 = EDGE_CURVE ( 'NONE', #12752, #11856, #117, .T. ) ;
#14072 = VECTOR ( 'NONE', #20987, 1000.000000000000000 ) ;
#14073 = EDGE_CURVE ( 'NONE', #17287, #30501, #29825, .T. ) ;
#14074 = AXIS2_PLACEMENT_3D ( 'NONE', #20130, #22451, #17590 ) ;
#14075 = DIRECTION ( 'NONE',  ( 1.000000000000000000, 0.000000000000000000, 0.000000000000000000 ) ) ;
#14077 = ORIENTED_EDGE ( 'NONE', *, *, #21661, .F. ) ;
#14076 = CARTESIAN_POINT ( 'NONE',  ( 10.55147673363119232, -4.116875700062100130, 2.376879293651050329 ) ) ;
#14078 = CARTESIAN_POINT ( 'NONE',  ( 23.25111450864416085, -3.256483526998273983E-15, 2.499999999999998668 ) ) ;
#14079 = CARTESIAN_POINT ( 'NONE',  ( 25.43628654896041397, -17.54453578616353582, -1.000000000000000000 ) ) ;
#14080 = FACE_OUTER_BOUND ( 'NONE', #22507, .T. ) ;
#14081 = B_SPLINE_CURVE_WITH_KNOTS ( 'NONE', 3,
 ( #3317, #23032, #153, #25897, #13011, #10338, #7984, #20553 ),
 .UNSPECIFIED., .F., .F.,
 ( 4, 2, 2, 4 ),
 ( 2.851296507433586163E-07, 0.001262135616845464631, 0.001893060860442827460, 0.002523986104040190290 ),
 .UNSPECIFIED. ) ;
#14082 = LOCAL_TIME ( 16, 7, 10.00000000000000000, #1797 ) ;
#14083 = CARTESIAN_POINT ( 'NONE',  ( 12.29359088965170521, -13.32350402071905471, -1.000000000000000000 ) ) ;
#14084 = EDGE_CURVE ( 'NONE', #32977, #30284, #10185, .T. ) ;
#14086 = EDGE_LOOP ( 'NONE', ( #5656, #23539, #18329 ) ) ;
#14085 = CARTESIAN_POINT ( 'NONE',  ( 107.9811858922438006, -17.79844364529119716, -4.362021580293085954 ) ) ;
#14087 = LINE ( 'NONE', #19107, #2903 ) ;
#14088 = FACE_OUTER_BOUND ( 'NONE', #18323, .T. ) ;
#14089 = FACE_OUTER_BOUND ( 'NONE', #32386, .T. ) ;
#14090 = ADVANCED_FACE ( 'NONE', ( #30950 ), #30647, .F. ) ;
#14091 = CARTESIAN_POINT ( 'NONE',  ( 5.377543748152548098, 7.530955069117513112, 2.741043480754951744 ) ) ;
#14092 = CARTESIAN_POINT ( 'NONE',  ( 85.38119660045754244, -6.034158634414237277, -4.522129901861164036 ) ) ;
#14093 = CC_DESIGN_DATE_AND_TIME_ASSIGNMENT ( #12629, #25505, ( #8747 ) ) ;
#14094 = VECTOR ( 'NONE', #10711, 1000.000000000000000 ) ;
#14095 = VERTEX_POINT ( 'NONE', #25769 ) ;
#14096 = DIRECTION ( 'NONE',  ( 0.000000000000000000, 0.000000000000000000, 1.000000000000000000 ) ) ;
#14097 = FACE_OUTER_BOUND ( 'NONE', #15142, .T. ) ;
#14098 = DIRECTION ( 'NONE',  ( 2.473959037481237219E-13, 1.000000000000000000, -0.000000000000000000 ) ) ;
#14099 = ORIENTED_EDGE ( 'NONE', *, *, #8993, .F. ) ;
#14100 = CARTESIAN_POINT ( 'NONE',  ( 102.8580990270160385, -4.820463887425400884, -4.522129901861163148 ) ) ;
#14101 = CARTESIAN_POINT ( 'NONE',  ( 21.37217251140765484, -21.79767279465048802, -1.352145825573628279 ) ) ;
#14102 = CC_DESIGN_APPROVAL ( #10621, ( #32825 ) ) ;
#14103 = ORIENTED_EDGE ( 'NONE', *, *, #22795, .F. ) ;
#14104 = CARTESIAN_POINT ( 'NONE',  ( 9.130836792357447607, -14.25899304337494478, -1.499999999999999112 ) ) ;
#14105 = ADVANCED_FACE ( 'NONE', ( #2389 ), #4872, .F. ) ;
#14106 = ORIENTED_EDGE ( 'NONE', *, *, #16588, .T. ) ;
#14107 = ORIENTED_EDGE ( 'NONE', *, *, #6133, .F. ) ;
#14108 = DIRECTION ( 'NONE',  ( 0.000000000000000000, 0.000000000000000000, -1.000000000000000000 ) ) ;
#14110 = ORIENTED_EDGE ( 'NONE', *, *, #7221, .F. ) ;
#14109 = FACE_OUTER_BOUND ( 'NONE', #28666, .T. ) ;
#14111 = ORIENTED_EDGE ( 'NONE', *, *, #782, .F. ) ;
#14112 = CARTESIAN_POINT ( 'NONE',  ( 108.8138202772576903, 17.05235780320128569, -4.110854392070767638 ) ) ;
#14113 = EDGE_CURVE ( 'NONE', #9508, #31957, #15736, .T. ) ;
#14114 = ORIENTED_EDGE ( 'NONE', *, *, #2811, .T. ) ;
#14115 = CARTESIAN_POINT ( 'NONE',  ( 2.274274201625327230, -9.680994141368730155, -5.222868219166962866 ) ) ;
#14116 = CARTESIAN_POINT ( 'NONE',  ( -3.671333707197877479E-13, 1.999317321091317545, -10.76487093102143433 ) ) ;
#14117 = VECTOR ( 'NONE', #16808, 1000.000000000000000 ) ;
#14119 = VERTEX_POINT ( 'NONE', #2897 ) ;
#14118 = CARTESIAN_POINT ( 'NONE',  ( 17.32050807568873552, 10.00000000000002309, -4.612695725900422872 ) ) ;
#14120 = CARTESIAN_POINT ( 'NONE',  ( 1.750000000000000000, 0.6700234925293840904, -8.473551116235670477 ) ) ;
#14121 = CARTESIAN_POINT ( 'NONE',  ( 5.377543748152547209, 1.391664247347333294, -7.892520144992419162 ) ) ;
#14122 = CARTESIAN_POINT ( 'NONE',  ( 101.9038780646438056, -5.514351699183295707, 1.526432238275731379 ) ) ;
#14123 = CARTESIAN_POINT ( 'NONE',  ( 102.7595417042496706, -3.401262957566509204, -3.636029349014984202 ) ) ;
#14124 = DIRECTION ( 'NONE',  ( 0.000000000000000000, 0.000000000000000000, 1.000000000000000000 ) ) ;
#14125 = EDGE_CURVE ( 'NONE', #19712, #16397, #8731, .T. ) ;
#14126 = CARTESIAN_POINT ( 'NONE',  ( 17.97422212135272446, -19.86246923125032282, -4.522129901861166701 ) ) ;
#14127 = FACE_OUTER_BOUND ( 'NONE', #21085, .T. ) ;
#14128 = CARTESIAN_POINT ( 'NONE',  ( 6.749760686538667009, 0.000000000000000000, 0.000000000000000000 ) ) ;
#14129 = EDGE_CURVE ( 'NONE', #4959, #31510, #9874, .T. ) ;
#14130 = LINE ( 'NONE', #6272, #26762 ) ;
#14131 = CC_DESIGN_PERSON_AND_ORGANIZATION_ASSIGNMENT ( #500, #13685, ( #21105 ) ) ;
#14132 = FACE_OUTER_BOUND ( 'NONE', #8319, .T. ) ;
#14133 = DIRECTION ( 'NONE',  ( 1.000000000000000000, -8.574039729943018344E-17, -0.000000000000000000 ) ) ;
#14134 = DIRECTION ( 'NONE',  ( -0.000000000000000000, -0.000000000000000000, -1.000000000000000000 ) ) ;
#14135 = CARTESIAN_POINT ( 'NONE',  ( -5.450050802731187360, -1.887961173149512062, -2.331437884370912261 ) ) ;
#14136 = VERTEX_POINT ( 'NONE', #19216 ) ;
#14137 = CARTESIAN_POINT ( 'NONE',  ( -6.950050800000000528, -0.9222479816126459840, -3.113457007523259268 ) ) ;
#14138 = CARTESIAN_POINT ( 'NONE',  ( 22.45654429440861222, -21.89488324759587101, -1.207178455809153395 ) ) ;
#14139 = DIRECTION ( 'NONE',  ( 0.000000000000000000, 0.1045284632676536235, -0.9945218953682734009 ) ) ;
#14140 = CARTESIAN_POINT ( 'NONE',  ( 9.437548970008970528, 0.1642588933130853524, 1.500000000000000000 ) ) ;
#14141 = ORIENTED_EDGE ( 'NONE', *, *, #2772, .T. ) ;
#14142 = CARTESIAN_POINT ( 'NONE',  ( 11.67286638378758745, -13.57952815233258903, -1.499999999999999778 ) ) ;
#14143 = ADVANCED_FACE ( 'NONE', ( #6834 ), #29913, .F. ) ;
#14144 = ORIENTED_EDGE ( 'NONE', *, *, #14073, .T. ) ;
#14145 = CARTESIAN_POINT ( 'NONE',  ( 0.1995908835383632951, -7.569794710591879472, 1.774175096175876432 ) ) ;
#14146 = EDGE_CURVE ( 'NONE', #14600, #29447, #14189, .T. ) ;
#14147 = CALENDAR_DATE ( 2026, 6, 10 ) ;
#14148 = CARTESIAN_POINT ( 'NONE',  ( 0.000000000000000000, 4.561279057474412646, 4.271385531633187682 ) ) ;
#14149 = ORIENTED_EDGE ( 'NONE', *, *, #23196, .T. ) ;
#14150 = CARTESIAN_POINT ( 'NONE',  ( 40.87896744410521421, -5.974071964853076899, 4.215290092884966811 ) ) ;
#14151 = CARTESIAN_POINT ( 'NONE',  ( -6.106376978575948300, 0.1572233378491222633, -3.000000000000000000 ) ) ;
#14152 = CARTESIAN_POINT ( 'NONE',  ( 40.87845373110570080, -5.880277441428658491, -4.150065482907210779 ) ) ;
#14153 = CARTESIAN_POINT ( 'NONE',  ( 24.05790257984022062, -17.31116499701210287, -1.379149890413408963 ) ) ;
#14154 = LINE ( 'NONE', #13656, #10771 ) ;
#14155 = EDGE_LOOP ( 'NONE', ( #20344, #23556, #17388, #16112 ) ) ;
#14156 = LINE ( 'NONE', #14303, #12484 ) ;
#14157 = LINE ( 'NONE', #27369, #16622 ) ;
#14158 = CARTESIAN_POINT ( 'NONE',  ( 25.96712173632212384, 22.75279134953752447, -5.471072653611070535 ) ) ;
#14160 = ORIENTED_EDGE ( 'NONE', *, *, #31653, .T. ) ;
#14159 = FACE_OUTER_BOUND ( 'NONE', #1365, .T. ) ;
#14161 = DIRECTION ( 'NONE',  ( 0.000000000000000000, -0.9993908270190956511, 0.03489949670250104552 ) ) ;
#14162 = DIRECTION ( 'NONE',  ( -2.219124775574964855E-17, -0.2588190451025251804, 0.9659258262890670910 ) ) ;
#14163 = DIRECTION ( 'NONE',  ( 1.000000000000000000, -0.000000000000000000, -0.000000000000000000 ) ) ;
#14164 = DIRECTION ( 'NONE',  ( 0.000000000000000000, 0.000000000000000000, -1.000000000000000000 ) ) ;
#14165 = CARTESIAN_POINT ( 'NONE',  ( 5.377543748152550762, -1.391664247347281780, 7.892520144992429820 ) ) ;
#14166 = DIRECTION ( 'NONE',  ( -1.000000000000000000, 0.000000000000000000, -0.000000000000000000 ) ) ;
#14167 = CARTESIAN_POINT ( 'NONE',  ( 3.249999999999999556, 0.000000000000000000, 0.000000000000000000 ) ) ;
#14168 = ORIENTED_EDGE ( 'NONE', *, *, #25213, .F. ) ;
#14169 = DIRECTION ( 'NONE',  ( -3.623545766764197982E-17, -0.4226182617406974984, -0.9063077870366508249 ) ) ;
#14170 = ORIENTED_EDGE ( 'NONE', *, *, #15116, .T. ) ;
#14171 = DIRECTION ( 'NONE',  ( -7.770718973608945377E-17, -0.9063077870366467170, -0.4226182617407064912 ) ) ;
#14172 = CARTESIAN_POINT ( 'NONE',  ( -59.40973711574257976, -5.237753430259554754, 5.221982333003774457 ) ) ;
#14173 = CARTESIAN_POINT ( 'NONE',  ( 29.25343337322282622, -7.426690278353109242, -4.522129901861164036 ) ) ;
#14174 = CARTESIAN_POINT ( 'NONE',  ( 7.249760686538667009, 0.000000000000000000, 0.000000000000000000 ) ) ;
#14175 = FACE_OUTER_BOUND ( 'NONE', #15638, .T. ) ;
#14176 = ORIENTED_EDGE ( 'NONE', *, *, #14409, .F. ) ;
#14177 = ADVANCED_FACE ( 'NONE', ( #22228 ), #32595, .T. ) ;
#14178 = CARTESIAN_POINT ( 'NONE',  ( 107.8403069887453967, 17.28892622633358656, -3.570939384223136059 ) ) ;
#14179 = EDGE_CURVE ( 'NONE', #11951, #29082, #26917, .T. ) ;
#14180 = VERTEX_POINT ( 'NONE', #24387 ) ;
#14181 = DATE_AND_TIME ( #24379, #9824 ) ;
#14182 = DIRECTION ( 'NONE',  ( 0.1027947991993878873, -0.9947025833170223263, 2.669847849745554669E-15 ) ) ;
#14183 = PLANE ( 'NONE',  #10151 ) ;
#14184 = ORIENTED_EDGE ( 'NONE', *, *, #31416, .T. ) ;
#14185 = CARTESIAN_POINT ( 'NONE',  ( 10.00000000000000000, -2.376879293651094294, 4.116875700062075261 ) ) ;
#14186 = ORIENTED_EDGE ( 'NONE', *, *, #26498, .F. ) ;
#14187 = ORIENTED_EDGE ( 'NONE', *, *, #25064, .F. ) ;
#14188 = DIRECTION ( 'NONE',  ( -1.000000000000000000, 0.000000000000000000, 0.000000000000000000 ) ) ;
#14189 = LINE ( 'NONE', #6682, #4880 ) ;
#14190 = CARTESIAN_POINT ( 'NONE',  ( 21.98499999999999943, 2.486304738420679783, -0.2613211581691337604 ) ) ;
#14191 = CARTESIAN_POINT ( 'NONE',  ( 0.4785084283111751269, -8.598468463561344421, -1.771410369227642834 ) ) ;
#14192 = B_SPLINE_CURVE_WITH_KNOTS ( 'NONE', 3,
 ( #7853, #15525, #17708, #5033, #2677, #15211, #12843, #2870 ),
 .UNSPECIFIED., .F., .F.,
 ( 4, 2, 2, 4 ),
 ( 2.304311362615608600E-07, 0.001227991214883613832, 0.001841871606757292763, 0.002455751998630971693 ),
 .UNSPECIFIED. ) ;
#14194 = ORIENTED_EDGE ( 'NONE', *, *, #23581, .F. ) ;
#14193 = CARTESIAN_POINT ( 'NONE',  ( 10.07279555557439998, 2.216694168388106068, -1.500000000000000222 ) ) ;
#14195 = CARTESIAN_POINT ( 'NONE',  ( -6.987550801365594033, -0.3701630799359326152, 3.521866450007987037 ) ) ;
#14196 = DIRECTION ( 'NONE',  ( 0.000000000000000000, -0.7071067811865465735, 0.7071067811865484609 ) ) ;
#14197 = DIRECTION ( 'NONE',  ( 0.000000000000000000, 0.000000000000000000, -1.000000000000000000 ) ) ;
#14198 = CARTESIAN_POINT ( 'NONE',  ( -14.83051435581985444, -21.73221622337167958, -1.500000000000000000 ) ) ;
#14199 = ORIENTED_EDGE ( 'NONE', *, *, #11602, .T. ) ;
#14201 = EDGE_LOOP ( 'NONE', ( #4488, #19293, #28530, #16978 ) ) ;
#14200 = CARTESIAN_POINT ( 'NONE',  ( -15.00280984543113583, -21.93932300455818307, 1.000000000000000000 ) ) ;
#14202 = CARTESIAN_POINT ( 'NONE',  ( -6.900050800000000706, 0.3135853898029611342, -2.983565686104819648 ) ) ;
#14203 = CARTESIAN_POINT ( 'NONE',  ( 23.54750000273119070, -0.7685399846772070775, 2.594547506269381465 ) ) ;
#14204 = DIRECTION ( 'NONE',  ( -1.000000000000000000, 8.574039729943019576E-17, -0.000000000000000000 ) ) ;
#14205 = B_SPLINE_CURVE_WITH_KNOTS ( 'NONE', 3,
 ( #5259, #32693, #9935, #12609, #20652, #9773, #2759 ),
 .UNSPECIFIED., .F., .F.,
 ( 4, 3, 4 ),
 ( 1.015220885719448636E-17, 0.002676966304866045410, 0.003456443485869430642 ),
 .UNSPECIFIED. ) ;
#14206 = CARTESIAN_POINT ( 'NONE',  ( -38.14293509397969473, 10.97000000000000419, 1.500000000000000000 ) ) ;
#14207 = DIRECTION ( 'NONE',  ( 0.000000000000000000, -0.9271838545667856479, -0.3746065934159164001 ) ) ;
#14208 = EDGE_CURVE ( 'NONE', #448, #14007, #9070, .T. ) ;
#14209 = CARTESIAN_POINT ( 'NONE',  ( 10.57125986779756843, 4.884328206559835905, 1.115095498423326559 ) ) ;
#14210 = CARTESIAN_POINT ( 'NONE',  ( 19.01022352368274326, -3.062944256723961534, 0.8105616806065999436 ) ) ;
#14211 = CARTESIAN_POINT ( 'NONE',  ( 107.3477315916820913, -15.88627780335592732, 1.500000000000000000 ) ) ;
#14212 = VERTEX_POINT ( 'NONE', #24894 ) ;
#14213 = CARTESIAN_POINT ( 'NONE',  ( 2.274274201625327230, 5.222868219166857173, 9.680994141368788775 ) ) ;
#14214 = ORIENTED_EDGE ( 'NONE', *, *, #30405, .T. ) ;
#14215 = CARTESIAN_POINT ( 'NONE',  ( 0.000000000000000000, 0.000000000000000000, 0.000000000000000000 ) ) ;
#14216 = CARTESIAN_POINT ( 'NONE',  ( 7.249760686538667009, 0.000000000000000000, 0.000000000000000000 ) ) ;
#14218 = CARTESIAN_POINT ( 'NONE',  ( 24.35832023931602208, -17.33818253687209676, 1.317734466820223549 ) ) ;
#14217 = CARTESIAN_POINT ( 'NONE',  ( 7.064423600674403225, -2.210816291637359932, -8.466096581344345395 ) ) ;
#14219 = EDGE_LOOP ( 'NONE', ( #26487, #30184, #914, #19213, #18911 ) ) ;
#14220 = LINE ( 'NONE', #16557, #14445 ) ;
#14221 = VERTEX_POINT ( 'NONE', #4671 ) ;
#14222 = DIRECTION ( 'NONE',  ( -0.03489949670250104552, -0.9993908270190956511, 0.000000000000000000 ) ) ;
#14224 = EDGE_LOOP ( 'NONE', ( #10387, #31858, #21755, #16279 ) ) ;
#14223 = CARTESIAN_POINT ( 'NONE',  ( 18.86025921852518650, -4.739244214245537101, -3.998506281407207208 ) ) ;
#14225 = ADVANCED_FACE ( 'NONE', ( #19894 ), #30109, .T. ) ;
#14226 = ORIENTED_EDGE ( 'NONE', *, *, #31005, .T. ) ;
#14227 = CARTESIAN_POINT ( 'NONE',  ( 2.425585535379221280, -9.314797388879910045, 5.239665997526856245 ) ) ;
#14228 = CARTESIAN_POINT ( 'NONE',  ( 25.75999999999999446, 1.024942698525265428, 2.863353032229740691 ) ) ;
#14230 = VERTEX_POINT ( 'NONE', #6505 ) ;
#14229 = CARTESIAN_POINT ( 'NONE',  ( -3.368835499171254799, -11.43153892038626829, -1.500000000000000888 ) ) ;
#14231 = CARTESIAN_POINT ( 'NONE',  ( 12.22604216692669254, 4.899348761096485205, -1.499999999999763300 ) ) ;
#14232 = CARTESIAN_POINT ( 'NONE',  ( 8.870145747188287189, 0.000000000000000000, -1.000000000000000222 ) ) ;
#14233 = ADVANCED_FACE ( 'NONE', ( #4022 ), #1504, .F. ) ;
#14234 = DIRECTION ( 'NONE',  ( 0.000000000000000000, 0.4226182617407007736, -0.9063077870366493816 ) ) ;
#14235 = CARTESIAN_POINT ( 'NONE',  ( 8.323087564152283235, -11.23204384871575812, -1.500000000000000000 ) ) ;
#14237 = ORIENTED_EDGE ( 'NONE', *, *, #32875, .T. ) ;
#14236 = CARTESIAN_POINT ( 'NONE',  ( 107.4512831466929583, -17.37794483578546689, -4.567559570125502511 ) ) ;
#14238 = DIRECTION ( 'NONE',  ( 1.000000000000000000, 0.000000000000000000, 0.000000000000000000 ) ) ;
#14239 = ADVANCED_FACE ( 'NONE', ( #17881 ), #5171, .T. ) ;
#14240 = PLANE ( 'NONE',  #16092 ) ;
#14241 = CARTESIAN_POINT ( 'NONE',  ( 8.585585455345263739, 0.000000000000000000, -1.000000000000000000 ) ) ;
#14242 = CARTESIAN_POINT ( 'NONE',  ( 24.41748882719689107, -17.42561905328290095, -1.443068816866804882 ) ) ;
#14243 = FACE_OUTER_BOUND ( 'NONE', #7216, .T. ) ;
#14244 = ORIENTED_EDGE ( 'NONE', *, *, #17256, .T. ) ;
#14245 = CARTESIAN_POINT ( 'NONE',  ( 0.7632845268398871230, 0.000000000000000000, 0.000000000000000000 ) ) ;
#14246 = EDGE_CURVE ( 'NONE', #18415, #5412, #15197, .T. ) ;
#14247 = CARTESIAN_POINT ( 'NONE',  ( 0.000000000000000000, 0.000000000000000000, 0.000000000000000000 ) ) ;
#14248 = EDGE_CURVE ( 'NONE', #31994, #24044, #12852, .T. ) ;
#14249 = CARTESIAN_POINT ( 'NONE',  ( 0.6708088701982984903, 0.000000000000000000, -4.612695725900422872 ) ) ;
#14250 = ORIENTED_EDGE ( 'NONE', *, *, #11893, .F. ) ;
#14251 = CARTESIAN_POINT ( 'NONE',  ( -10.00000000000000000, 0.000000000000000000, 0.000000000000000000 ) ) ;
#14252 = CARTESIAN_POINT ( 'NONE',  ( 2.437082427505627091, 9.703015696712945726, 4.432669656489494514 ) ) ;
#14253 = ORIENTED_EDGE ( 'NONE', *, *, #27663, .F. ) ;
#14254 = CARTESIAN_POINT ( 'NONE',  ( 108.1960732670207079, 19.26997324246909926, 4.630839363390458985 ) ) ;
#14255 = ORIENTED_EDGE ( 'NONE', *, *, #15500, .F. ) ;
#14256 = VERTEX_POINT ( 'NONE', #25399 ) ;
#14257 = CARTESIAN_POINT ( 'NONE',  ( -3.148734258548802813E-16, -3.672404558090061943, 3.407865132560167432 ) ) ;
#14259 = ORIENTED_EDGE ( 'NONE', *, *, #7015, .T. ) ;
#14258 = CARTESIAN_POINT ( 'NONE',  ( 7.064632879756603145, -8.711672189281433276, 0.8180878109961572386 ) ) ;
#14260 = ORIENTED_EDGE ( 'NONE', *, *, #4736, .F. ) ;
#14261 = CARTESIAN_POINT ( 'NONE',  ( 23.61000000136559507, 3.156283516753366047, 0.9349337715887203748 ) ) ;
#14262 = ADVANCED_FACE ( 'NONE', ( #2659 ), #8583, .T. ) ;
#14263 = VERTEX_POINT ( 'NONE', #15510 ) ;
#14264 = CARTESIAN_POINT ( 'NONE',  ( 7.249760686538667009, 0.000000000000000000, 0.000000000000000000 ) ) ;
#14265 = CARTESIAN_POINT ( 'NONE',  ( 6.883866557622100757, -7.943335131954982309, -3.625395379390166983 ) ) ;
#14267 = ORIENTED_EDGE ( 'NONE', *, *, #26751, .F. ) ;
#14266 = DIRECTION ( 'NONE',  ( 0.000000000000000000, -0.8191520442889983489, 0.5735764363510366115 ) ) ;
#14268 = CARTESIAN_POINT ( 'NONE',  ( 21.98500000273118715, -0.2613211581691358698, -2.486304738420681559 ) ) ;
#14269 = CARTESIAN_POINT ( 'NONE',  ( -56.77852586542613267, 0.3797334620625366086, -1.050000000000000044 ) ) ;
#14270 = CARTESIAN_POINT ( 'NONE',  ( 6.357667697713667465, 0.9262207444595902395, 8.557242355892487495 ) ) ;
#14271 = CARTESIAN_POINT ( 'NONE',  ( 4.749760686538667009, 7.892520144992435149, 1.391664247347255134 ) ) ;
#14272 =( BOUNDED_SURFACE ( )  B_SPLINE_SURFACE ( 1, 3, ( 
 ( #15210, #7505, #27920, #15524 ),
 ( #32949, #30782, #5032, #25738 ) ),
 .UNSPECIFIED., .F., .F., .F. ) 
 B_SPLINE_SURFACE_WITH_KNOTS ( ( 2, 2 ),
 ( 4, 4 ),
 ( 0.000000000000000000, 1.000000000000000000 ),
 ( 0.000000000000000000, 1.000000000000000000 ),
 .UNSPECIFIED. ) 
 GEOMETRIC_REPRESENTATION_ITEM ( )  RATIONAL_B_SPLINE_SURFACE ( (
 ( 1.000000000000000000, 0.9321687722090974404, 0.9321687722090974404, 1.000000000000000000),
 ( 1.000000000000000000, 0.9321687722090974404, 0.9321687722090974404, 1.000000000000000000) ) ) 
 REPRESENTATION_ITEM ( '' )  SURFACE ( )  );
#14273 = CARTESIAN_POINT ( 'NONE',  ( 13.24595149388380300, -17.70232641594038014, -5.485967528433937979 ) ) ;
#14274 = CYLINDRICAL_SURFACE ( 'NONE', #31067, 6.250000000000000000 ) ;
#14275 = DIRECTION ( 'NONE',  ( 1.224646799147353207E-16, 1.000000000000000000, 0.000000000000000000 ) ) ;
#14276 = EDGE_CURVE ( 'NONE', #15410, #28448, #20216, .T. ) ;
#14277 = CARTESIAN_POINT ( 'NONE',  ( -2.249956573341760357, 1.323625320507108460, 3.284597389080124774 ) ) ;
#14278 = DIRECTION ( 'NONE',  ( -1.000000000000000000, 0.000000000000000000, 0.000000000000000000 ) ) ;
#14279 = CARTESIAN_POINT ( 'NONE',  ( 3.499999999999999556, -2.652816298622381996, -5.657964889053610058 ) ) ;
#14280 = EDGE_CURVE ( 'NONE', #3186, #3463, #12828, .T. ) ;
#14281 = CARTESIAN_POINT ( 'NONE',  ( 3.063284526839887167, -2.223716399045513992, -8.461683424509338636 ) ) ;
#14282 = EDGE_CURVE ( 'NONE', #11672, #29889, #6985, .T. ) ;
#14283 = CARTESIAN_POINT ( 'NONE',  ( -5.400050802731186650, -0.9222479816126459840, -3.113457007523259268 ) ) ;
#14284 = ORIENTED_EDGE ( 'NONE', *, *, #11205, .T. ) ;
#14285 = CARTESIAN_POINT ( 'NONE',  ( -3.350050800000000439, 0.9222479816126443186, 3.113457007523260156 ) ) ;
#14286 = CARTESIAN_POINT ( 'NONE',  ( 0.000000000000000000, 0.000000000000000000, 0.000000000000000000 ) ) ;
#14287 = CARTESIAN_POINT ( 'NONE',  ( -5.500050802731188071, -2.853674364686378695, -1.549418761218566809 ) ) ;
#14288 = CARTESIAN_POINT ( 'NONE',  ( 7.594557537342751630, -2.555973540832573665, 1.500000000000000000 ) ) ;
#14289 = ORIENTED_EDGE ( 'NONE', *, *, #30070, .T. ) ;
#14290 = ORIENTED_EDGE ( 'NONE', *, *, #2889, .T. ) ;
#14291 = CARTESIAN_POINT ( 'NONE',  ( 5.414493835220194562, -13.03402177297271791, 1.500000000000845324 ) ) ;
#14292 = APPROVAL_DATE_TIME ( #32041, #29231 ) ;
#14293 = CARTESIAN_POINT ( 'NONE',  ( 5.377543748152549874, 5.151476664237477188, 6.139290821770273077 ) ) ;
#14294 = ORIENTED_EDGE ( 'NONE', *, *, #31668, .T. ) ;
#14295 = CARTESIAN_POINT ( 'NONE',  ( -0.6222850063875347004, -14.83242053952924522, 1.500000000000000000 ) ) ;
#14296 = EDGE_CURVE ( 'NONE', #17299, #19432, #28223, .T. ) ;
#14297 = CC_DESIGN_PERSON_AND_ORGANIZATION_ASSIGNMENT ( #5969, #16329, ( #30333 ) ) ;
#14298 = CARTESIAN_POINT ( 'NONE',  ( 25.75999999999999801, -2.208672634433321348E-15, 0.000000000000000000 ) ) ;
#14299 = CARTESIAN_POINT ( 'NONE',  ( -2.673784117434885310, -0.4252644786298063750, 1.725835304028459527 ) ) ;
#14300 = CARTESIAN_POINT ( 'NONE',  ( 3.063284526839887167, -0.4999240074895051067, 8.734705317681624948 ) ) ;
#14301 = CARTESIAN_POINT ( 'NONE',  ( 7.249760686538667009, 1.391664247347333294, -7.892520144992419162 ) ) ;
#14302 = VERTEX_POINT ( 'NONE', #9854 ) ;
#14303 = CARTESIAN_POINT ( 'NONE',  ( 10.52034268205830259, -3.672404558090015314, -3.407865132560218946 ) ) ;
#14304 = CARTESIAN_POINT ( 'NONE',  ( 23.24965750580003387, -21.93932300456764395, -1.000000000000000000 ) ) ;
#14305 = CARTESIAN_POINT ( 'NONE',  ( 7.249760686538667009, -7.953573330858239920, 3.647351267791542284 ) ) ;
#14307 = ORIENTED_EDGE ( 'NONE', *, *, #24268, .T. ) ;
#14306 = FACE_OUTER_BOUND ( 'NONE', #6285, .T. ) ;
#14308 = DIRECTION ( 'NONE',  ( -8.649074885250573632E-15, 0.03489949670250105246, 0.9993908270190957621 ) ) ;
#14309 = CARTESIAN_POINT ( 'NONE',  ( -31.18783180709124636, -21.43932300455417916, 1.500000000000000000 ) ) ;
#14310 = LINE ( 'NONE', #4143, #20421 ) ;
#14311 = CARTESIAN_POINT ( 'NONE',  ( 26.07786135537692473, 19.05625643470508024, 1.113327811892661501 ) ) ;
#14312 = CARTESIAN_POINT ( 'NONE',  ( 0.5032039692148283505, 9.704418393831403478, 0.7352278974741125461 ) ) ;
#14313 = EDGE_CURVE ( 'NONE', #10741, #3275, #13865, .T. ) ;
#14314 = DIRECTION ( 'NONE',  ( -1.000000000000000000, -0.000000000000000000, -0.000000000000000000 ) ) ;
#14315 = CARTESIAN_POINT ( 'NONE',  ( 25.02103040602151651, -17.46523595225292880, -1.208340562988329037 ) ) ;
#14316 = PLANE ( 'NONE',  #14516 ) ;
#14317 = DIRECTION ( 'NONE',  ( 1.000000000000000000, 0.000000000000000000, 0.000000000000000000 ) ) ;
#14318 = ORIENTED_EDGE ( 'NONE', *, *, #27986, .T. ) ;
#14319 = DIRECTION ( 'NONE',  ( 1.000000000000000000, 2.650271977186794621E-15, 0.000000000000000000 ) ) ;
#14320 = ORIENTED_EDGE ( 'NONE', *, *, #28987, .F. ) ;
#14321 = DIRECTION ( 'NONE',  ( -1.000000000000000000, 8.574039729943019576E-17, -6.162975822039154730E-33 ) ) ;
#14322 = DIRECTION ( 'NONE',  ( 0.000000000000000000, -0.08715574274764384399, -0.9961946980917467664 ) ) ;
#14323 = LINE ( 'NONE', #24524, #24750 ) ;
#14324 = DIRECTION ( 'NONE',  ( -1.000000000000000000, -0.000000000000000000, 0.000000000000000000 ) ) ;
#14325 = CYLINDRICAL_SURFACE ( 'NONE', #5541, 0.5000000000000004441 ) ;
#14326 = ORIENTED_EDGE ( 'NONE', *, *, #29744, .F. ) ;
#14327 = ORIENTED_EDGE ( 'NONE', *, *, #24977, .F. ) ;
#14328 = DATE_AND_TIME ( #9157, #23688 ) ;
#14329 = CARTESIAN_POINT ( 'NONE',  ( 102.4230704567010264, -3.996592730545043715, 3.998506272702885056 ) ) ;
#14330 = EDGE_CURVE ( 'NONE', #32682, #23691, #7993, .T. ) ;
#14331 = CARTESIAN_POINT ( 'NONE',  ( -8.000050800000000351, 0.000000000000000000, -3.000000000000000444 ) ) ;
#14332 = CARTESIAN_POINT ( 'NONE',  ( 7.064423669210280643, 6.226446564518129279, -6.147671362330616063 ) ) ;
#14333 = EDGE_LOOP ( 'NONE', ( #1953, #1468, #1400, #6600, #28563 ) ) ;
#14334 = VERTEX_POINT ( 'NONE', #10352 ) ;
#14335 = PLANE ( 'NONE',  #29523 ) ;
#14336 = CARTESIAN_POINT ( 'NONE',  ( 6.880159396099835512, -7.882559112973138937, -3.754731129947869395 ) ) ;
#14337 = CARTESIAN_POINT ( 'NONE',  ( 24.92249999999999943, 2.378061970571979433, -1.291182301015470824 ) ) ;
#14338 = CARTESIAN_POINT ( 'NONE',  ( 7.214435349459066060, -13.85197079645077878, -1.500000000000000444 ) ) ;
#14340 = ORIENTED_EDGE ( 'NONE', *, *, #18545, .F. ) ;
#14339 = DIRECTION ( 'NONE',  ( 0.000000000000000000, 0.2079116908177532919, 0.9781476007338070211 ) ) ;
#14341 = CARTESIAN_POINT ( 'NONE',  ( -2.187550801365593767, -0.3701630799359326152, 3.521866450007987037 ) ) ;
#14342 = DIRECTION ( 'NONE',  ( -0.9960221812693187404, 0.08910563629484180570, 0.000000000000000000 ) ) ;
#14343 = CARTESIAN_POINT ( 'NONE',  ( 2.864530875629061057, -9.539603485476147782, -0.6595692664038580455 ) ) ;
#14344 = DIRECTION ( 'NONE',  ( -1.067350013832299672E-17, 0.4539904997395510788, -0.8910065241883655673 ) ) ;
#14345 = ORIENTED_EDGE ( 'NONE', *, *, #19783, .T. ) ;
#14346 = ADVANCED_FACE ( 'NONE', ( #5019 ), #30771, .T. ) ;
#14348 = ORIENTED_EDGE ( 'NONE', *, *, #24314, .F. ) ;
#14347 = DIRECTION ( 'NONE',  ( 0.8660254037844427044, -0.4999999999999931721, 0.000000000000000000 ) ) ;
#14349 = EDGE_CURVE ( 'NONE', #2520, #19511, #20563, .T. ) ;
#14350 = CARTESIAN_POINT ( 'NONE',  ( 5.521001242456709868, 0.4999999999999998890, 5.764947386686755770 ) ) ;
#14351 = ADVANCED_FACE ( 'NONE', ( #25724 ), #5512, .T. ) ;
#14352 = CARTESIAN_POINT ( 'NONE',  ( 12.44989959798868817, 20.00000000000000000, 13.00000000000004441 ) ) ;
#14353 = CARTESIAN_POINT ( 'NONE',  ( 25.11000000136559507, -2.892927487894331406, 1.570731468192932523 ) ) ;
#14354 = CARTESIAN_POINT ( 'NONE',  ( 2.857987970441411729, -3.588272043362970898, -8.861329655858744658 ) ) ;
#14355 = DIRECTION ( 'NONE',  ( 0.000000000000000000, -0.000000000000000000, -1.000000000000000000 ) ) ;
#14356 = DIRECTION ( 'NONE',  ( 0.000000000000000000, -0.9271838545667855369, -0.3746065934159163446 ) ) ;
#14357 = CARTESIAN_POINT ( 'NONE',  ( 29.33166896507317389, -3.955587949931067993, 1.529339504158915064 ) ) ;
#14358 = CARTESIAN_POINT ( 'NONE',  ( -3.387550801365593056, 0.3701630799359330593, -3.521866450007987037 ) ) ;
#14359 = EDGE_LOOP ( 'NONE', ( #13087, #18132, #7852, #28102 ) ) ;
#14360 = CARTESIAN_POINT ( 'NONE',  ( 102.9885081044300676, -6.698322160490901567, -0.07017451552783579571 ) ) ;
#14361 = ORIENTED_EDGE ( 'NONE', *, *, #27593, .T. ) ;
#14362 = AXIS2_PLACEMENT_3D ( 'NONE', #14558, #10146, #7668 ) ;
#14363 = CARTESIAN_POINT ( 'NONE',  ( 25.98690466878746008, 22.56136012750956965, -0.4463807625373771293 ) ) ;
#14364 = CARTESIAN_POINT ( 'NONE',  ( 3.499999999999999556, -5.349675154362298457, -3.229702268444986757 ) ) ;
#14365 = CARTESIAN_POINT ( 'NONE',  ( 2.593512329575687483E-16, 3.024842911000745094, -3.993798362933278057 ) ) ;
#14366 = VERTEX_POINT ( 'NONE', #25228 ) ;
#14367 = VECTOR ( 'NONE', #26178, 1000.000000000000114 ) ;
#14368 = CARTESIAN_POINT ( 'NONE',  ( 21.16281565822857758, -21.79884031534714595, 1.349901004997127396 ) ) ;
#14369 = EDGE_LOOP ( 'NONE', ( #30944, #2222, #14532, #28254, #32631 ) ) ;
#14370 = CARTESIAN_POINT ( 'NONE',  ( 1.149978682276028730, 0.000000000000000000, -7.916915373446320459 ) ) ;
#14372 = ORIENTED_EDGE ( 'NONE', *, *, #16988, .T. ) ;
#14371 = CARTESIAN_POINT ( 'NONE',  ( 40.87773210429867987, -5.748708618940125525, -3.993433839915444761 ) ) ;
#14373 = ORIENTED_EDGE ( 'NONE', *, *, #1623, .T. ) ;
#14374 = CYLINDRICAL_SURFACE ( 'NONE', #28432, 6.250000000000000000 ) ;
#14375 = CARTESIAN_POINT ( 'NONE',  ( 41.43141396789279440, -2.886852813799070105, 1.010822989962091301 ) ) ;
#14376 = EDGE_CURVE ( 'NONE', #10953, #11269, #23550, .T. ) ;
#14378 = ORIENTED_EDGE ( 'NONE', *, *, #25190, .T. ) ;
#14377 = CARTESIAN_POINT ( 'NONE',  ( -3.686555117304171070, -10.77456164543319161, -1.500000000000000444 ) ) ;
#14379 = CARTESIAN_POINT ( 'NONE',  ( 21.53922796474764567, 16.55061608779757520, -1.500000000000000000 ) ) ;
#14380 = FACE_OUTER_BOUND ( 'NONE', #29248, .T. ) ;
#14381 = CARTESIAN_POINT ( 'NONE',  ( -3.467098320250194821, -1.941669238915278983, 1.500000000001435296 ) ) ;
#14382 = CARTESIAN_POINT ( 'NONE',  ( 7.230698034991824841, -5.790874021893237966, -1.499999999999857225 ) ) ;
#14384 = ORIENTED_EDGE ( 'NONE', *, *, #5111, .T. ) ;
#14383 = CARTESIAN_POINT ( 'NONE',  ( 108.0598553040188534, -18.93126360436130895, -4.568634059891971688 ) ) ;
#14385 = DIRECTION ( 'NONE',  ( 1.000000000000000000, -8.574039729943018344E-17, -0.000000000000000000 ) ) ;
#14386 = VECTOR ( 'NONE', #12960, 1000.000000000000000 ) ;
#14387 = TOROIDAL_SURFACE ( 'NONE', #11211, 10.43371088333261731, 0.4500000000000000111 ) ;
#14388 = B_SPLINE_CURVE_WITH_KNOTS ( 'NONE', 3,
 ( #24288, #3732, #11247, #16418, #21938, #21451, #6233, #31828 ),
 .UNSPECIFIED., .F., .F.,
 ( 4, 2, 2, 4 ),
 ( 2.213836054374538867E-07, 0.001261154818855340096, 0.001891621536480290978, 0.002522088254105242077 ),
 .UNSPECIFIED. ) ;
#14389 = CARTESIAN_POINT ( 'NONE',  ( 5.887530024394195038, -2.518482652462503690, -8.008238305624875153 ) ) ;
#14390 = CARTESIAN_POINT ( 'NONE',  ( 24.48500000136559507, 2.892927487894327410, -1.570731468192931635 ) ) ;
#14391 = LINE ( 'NONE', #12086, #31600 ) ;
#14392 = CARTESIAN_POINT ( 'NONE',  ( 0.1606233661161337867, -7.161985370900606718, 7.854816391753094429 ) ) ;
#14393 = VECTOR ( 'NONE', #30960, 1000.000000000000000 ) ;
#14394 = ORIENTED_EDGE ( 'NONE', *, *, #14562, .T. ) ;
#14395 = CARTESIAN_POINT ( 'NONE',  ( -6.350050800000000883, -3.113457007523259268, 0.9222479816126455399 ) ) ;
#14396 = CARTESIAN_POINT ( 'NONE',  ( -10.00000000000000000, 0.000000000000000000, 0.000000000000000000 ) ) ;
#14397 = CARTESIAN_POINT ( 'NONE',  ( -23.54713438637982748, 5.934235225036485595, 7.654118351624816796 ) ) ;
#14398 = VERTEX_POINT ( 'NONE', #4827 ) ;
#14399 = CARTESIAN_POINT ( 'NONE',  ( -2.162942409646512854, 4.884725290497410777E-15, -2.999999999999999556 ) ) ;
#14400 = CIRCLE ( 'NONE', #31529, 6.000000000000000888 ) ;
#14401 = CARTESIAN_POINT ( 'NONE',  ( 3.393608999705061802, -0.06500480712390584170, -1.255126411524210450 ) ) ;
#14402 = VERTEX_POINT ( 'NONE', #334 ) ;
#14403 = CARTESIAN_POINT ( 'NONE',  ( 56.97280603064898941, -277.2763395528616002, 4.999054092451758358 ) ) ;
#14404 = ORIENTED_EDGE ( 'NONE', *, *, #774, .F. ) ;
#14405 = CIRCLE ( 'NONE', #35, 8.750000000000000000 ) ;
#14406 = AXIS2_PLACEMENT_3D ( 'NONE', #10928, #31180, #18280 ) ;
#14407 = ORIENTED_EDGE ( 'NONE', *, *, #31622, .F. ) ;
#14408 = CARTESIAN_POINT ( 'NONE',  ( 13.62547635268498780, 21.94000000000002970, 1.500000000000000000 ) ) ;
#14409 = EDGE_CURVE ( 'NONE', #6020, #23760, #28355, .T. ) ;
#14410 = APPROVAL_DATE_TIME ( #21960, #10621 ) ;
#14412 = ORIENTED_EDGE ( 'NONE', *, *, #30395, .F. ) ;
#14411 = CARTESIAN_POINT ( 'NONE',  ( 20.06012370291166391, -21.48645126995948829, -1.642756992391330773 ) ) ;
#14413 = ORIENTED_EDGE ( 'NONE', *, *, #28588, .T. ) ;
#14414 = CARTESIAN_POINT ( 'NONE',  ( 21.29750000136559507, -0.3178988483021076838, -3.024605502323848949 ) ) ;
#14415 = AXIS2_PLACEMENT_3D ( 'NONE', #16832, #1129, #31741 ) ;
#14416 = ORIENTED_EDGE ( 'NONE', *, *, #27126, .F. ) ;
#14418 = AXIS2_PLACEMENT_3D ( 'NONE', #18645, #450, #28357 ) ;
#14417 = CARTESIAN_POINT ( 'NONE',  ( -8.000050800000000351, 0.000000000000000000, 0.000000000000000000 ) ) ;
#14419 = ADVANCED_FACE ( 'NONE', ( #20870 ), #18211, .T. ) ;
#14420 = CARTESIAN_POINT ( 'NONE',  ( -31.60000000000018971, -21.93932300455407969, 1.499999999998983480 ) ) ;
#14422 = EDGE_LOOP ( 'NONE', ( #16334, #11603, #32675, #24966 ) ) ;
#14421 = CARTESIAN_POINT ( 'NONE',  ( -50.60000000000000142, -10.96966150227468972, 1.000000000000000000 ) ) ;
#14423 = CARTESIAN_POINT ( 'NONE',  ( 0.000000000000000000, 4.472189673936902032, -8.264486777890061475 ) ) ;
#14424 = CARTESIAN_POINT ( 'NONE',  ( 7.249760686538667009, -7.953573330858239920, 3.647351267791542284 ) ) ;
#14425 = EDGE_CURVE ( 'NONE', #17751, #1971, #6303, .T. ) ;
#14426 = CYLINDRICAL_SURFACE ( 'NONE', #537, 6.999999999999998224 ) ;
#14427 = CARTESIAN_POINT ( 'NONE',  ( 22.92250000136559862, -1.913930629741527500, 2.363507492473149618 ) ) ;
#14428 = DIRECTION ( 'NONE',  ( 0.000000000000000000, -0.7071067811865495711, 0.7071067811865455743 ) ) ;
#14429 = CIRCLE ( 'NONE', #52, 11.00000000000000000 ) ;
#14430 = CARTESIAN_POINT ( 'NONE',  ( 0.4398628304357228846, -12.95602692781729282, -5.485967528433938867 ) ) ;
#14431 = DIRECTION ( 'NONE',  ( -1.000000000000000000, -0.000000000000000000, -0.000000000000000000 ) ) ;
#14432 = CYLINDRICAL_SURFACE ( 'NONE', #32291, 8.749000000000002331 ) ;
#14433 = AXIS2_PLACEMENT_3D ( 'NONE', #21310, #8924, #6602 ) ;
#14434 = EDGE_CURVE ( 'NONE', #140, #16376, #32115, .T. ) ;
#14435 = AXIS2_PLACEMENT_3D ( 'NONE', #22776, #7546, #25601 ) ;
#14436 = FACE_OUTER_BOUND ( 'NONE', #25513, .T. ) ;
#14437 = DIRECTION ( 'NONE',  ( 0.000000000000000000, 0.000000000000000000, 1.000000000000000000 ) ) ;
#14438 = CARTESIAN_POINT ( 'NONE',  ( 4.749760686538667009, 4.007137495034909236, -6.940565734314555257 ) ) ;
#14439 = AXIS2_PLACEMENT_3D ( 'NONE', #14842, #9347, #25041 ) ;
#14440 = FACE_OUTER_BOUND ( 'NONE', #13707, .T. ) ;
#14441 = CARTESIAN_POINT ( 'NONE',  ( -5.150050802731186650, 2.983565686104819648, 0.3135853898029609677 ) ) ;
#14442 = ORIENTED_EDGE ( 'NONE', *, *, #28160, .T. ) ;
#14443 = EDGE_CURVE ( 'NONE', #14180, #3790, #23531, .T. ) ;
#14444 = CARTESIAN_POINT ( 'NONE',  ( -3.700050800000000084, 0.3135853898029611342, -2.983565686104819648 ) ) ;
#14445 = VECTOR ( 'NONE', #24418, 1000.000000000000114 ) ;
#14446 = FACE_OUTER_BOUND ( 'NONE', #883, .T. ) ;
#14447 = LINE ( 'NONE', #6936, #741 ) ;
#14448 = ORIENTED_EDGE ( 'NONE', *, *, #14855, .T. ) ;
#14449 = DIRECTION ( 'NONE',  ( -1.000000000000000000, -0.000000000000000000, -0.000000000000000000 ) ) ;
#14450 = CARTESIAN_POINT ( 'NONE',  ( -7.312942406915325044, -8.831141768130910875E-16, 2.999999999999999556 ) ) ;
#14452 = ORIENTED_EDGE ( 'NONE', *, *, #6755, .T. ) ;
#14451 = B_SPLINE_CURVE_WITH_KNOTS ( 'NONE', 3,
 ( #27917, #2519, #12687, #22891, #10173, #15359, #7197, #17892 ),
 .UNSPECIFIED., .F., .F.,
 ( 4, 2, 2, 4 ),
 ( 5.099451029773404998E-07, 0.001229189756374618209, 0.001843529662010439307, 0.002457869567646260404 ),
 .UNSPECIFIED. ) ;
#14453 = CARTESIAN_POINT ( 'NONE',  ( 18.48762451651099781, -16.70791404657606094, 1.499999999999163558 ) ) ;
#14454 = PERSON_AND_ORGANIZATION ( #6766, #25292 ) ;
#14455 = AXIS2_PLACEMENT_3D ( 'NONE', #12451, #19653, #4262 ) ;
#14456 = CARTESIAN_POINT ( 'NONE',  ( -2.850050799999999995, 1.549418761218566143, -2.853674364686379583 ) ) ;
#14457 = VERTEX_POINT ( 'NONE', #23714 ) ;
#14458 = CARTESIAN_POINT ( 'NONE',  ( -0.3439025151734569907, -15.06911885298311304, 1.500000000000000444 ) ) ;
#14459 = AXIS2_PLACEMENT_3D ( 'NONE', #2020, #24557, #1681 ) ;
#14460 = CIRCLE ( 'NONE', #1680, 0.4499999999999999556 ) ;
#14461 = CARTESIAN_POINT ( 'NONE',  ( -5.900050800000000706, 2.983565686104819648, 0.3135853898029609677 ) ) ;
#14462 = CARTESIAN_POINT ( 'NONE',  ( 69.07045576167539025, -6.116484151751043541, -3.993434826750828837 ) ) ;
#14463 = VECTOR ( 'NONE', #2949, 1000.000000000000000 ) ;
#14464 = CARTESIAN_POINT ( 'NONE',  ( 5.887529755120530339, -1.823049025159242831, 8.194579018285287120 ) ) ;
#14465 = CARTESIAN_POINT ( 'NONE',  ( -23.54713438637982748, 10.22246055240786333, 9.386673846173426483 ) ) ;
#14466 =( BOUNDED_CURVE ( )  B_SPLINE_CURVE ( 2, ( #18955, #6232, #3910, #29471, #1052, #13895, #28984, #4071, #6381, #1552, #29145 ),
 .UNSPECIFIED., .F., .F. ) 
 B_SPLINE_CURVE_WITH_KNOTS ( ( 3, 2, 2, 2, 2, 3 ),
 ( 0.4353822619934377136, 0.4375000000000000000, 0.4531250000000000000, 0.4687500000000000000, 0.4843750000000000000, 0.4978822619934377136 ),
 .UNSPECIFIED. ) 
 CURVE ( )  GEOMETRIC_REPRESENTATION_ITEM ( )  RATIONAL_B_SPLINE_CURVE ( ( 0.9821626249036857770, 0.9896829947469991673, 1.000000000000000000, 0.9238795325112867385, 1.000000000000000000, 0.9238795325112867385, 1.000000000000000000, 0.9238795325112867385, 1.000000000000000000, 0.9341965377642874602, 0.9821626249036857770 ) ) 
 REPRESENTATION_ITEM ( '' )  );
#14467 = ORIENTED_EDGE ( 'NONE', *, *, #15411, .T. ) ;
#14468 = EDGE_CURVE ( 'NONE', #14256, #12536, #18526, .T. ) ;
#14469 = AXIS2_PLACEMENT_3D ( 'NONE', #24097, #14075, #11723 ) ;
#14470 = CARTESIAN_POINT ( 'NONE',  ( -2.681019058075245542, 0.000000000000000000, 1.353976854744275871 ) ) ;
#14471 = ADVANCED_FACE ( 'NONE', ( #8478 ), #1134, .F. ) ;
#14472 = DIRECTION ( 'NONE',  ( -0.000000000000000000, -0.8191520442889951292, 0.5735764363510413855 ) ) ;
#14473 = LINE ( 'NONE', #27187, #18308 ) ;
#14474 = CIRCLE ( 'NONE', #8615, 0.4500000000000000111 ) ;
#14475 = CIRCLE ( 'NONE', #18768, 0.4500000000000013989 ) ;
#14477 = ORIENTED_EDGE ( 'NONE', *, *, #17541, .F. ) ;
#14476 = CARTESIAN_POINT ( 'NONE',  ( 25.71927239433071222, 2.993516940937198889, -0.04068705237182682760 ) ) ;
#14478 = CARTESIAN_POINT ( 'NONE',  ( 6.357667408475528248, -8.588075071450651521, -0.5738000813809884804 ) ) ;
#14479 = CARTESIAN_POINT ( 'NONE',  ( 41.43141396789281572, -2.886852813804338780, 0.07017451552781951707 ) ) ;
#14480 = CYLINDRICAL_SURFACE ( 'NONE', #28352, 8.500000000000000000 ) ;
#14481 = CARTESIAN_POINT ( 'NONE',  ( 26.02102126874770249, 19.05032542655294137, 1.189564967197544343 ) ) ;
#14482 = CARTESIAN_POINT ( 'NONE',  ( 2.440333653313243367, -9.715096239900898212, 4.424884217110374607 ) ) ;
#14483 = ADVANCED_FACE ( 'NONE', ( #18676 ), #5980, .F. ) ;
#14484 = CARTESIAN_POINT ( 'NONE',  ( -29.24402871571406237, -28.43932300454937590, 11.00000000000000000 ) ) ;
#14485 = DIRECTION ( 'NONE',  ( -1.000000000000000000, 0.000000000000000000, 0.000000000000000000 ) ) ;
#14486 = CARTESIAN_POINT ( 'NONE',  ( 23.27353278736381981, -21.94187821002792660, 1.000000000000000000 ) ) ;
#14487 = LINE ( 'NONE', #3549, #28953 ) ;
#14488 = ORIENTED_EDGE ( 'NONE', *, *, #14246, .T. ) ;
#14489 = CARTESIAN_POINT ( 'NONE',  ( 20.73500000273118715, -2.486304738420683780, 0.2613211581691335383 ) ) ;
#14490 = ORIENTED_EDGE ( 'NONE', *, *, #9236, .F. ) ;
#14491 = AXIS2_PLACEMENT_3D ( 'NONE', #616, #10807, #18835 ) ;
#14493 = EDGE_CURVE ( 'NONE', #28865, #18809, #2769, .T. ) ;
#14492 = AXIS2_PLACEMENT_3D ( 'NONE', #910, #31982, #3913 ) ;
#14494 = CARTESIAN_POINT ( 'NONE',  ( -6.454531657079158435, -1.545410377633946286, 2.846291840500174697 ) ) ;
#14495 = CC_DESIGN_PERSON_AND_ORGANIZATION_ASSIGNMENT ( #26013, #31212, ( #21588 ) ) ;
#14496 = CARTESIAN_POINT ( 'NONE',  ( 25.23500000136559507, -3.156283516753370044, -0.9349337715887220401 ) ) ;
#14497 = CIRCLE ( 'NONE', #31611, 0.5000000000000004441 ) ;
#14498 = DIRECTION ( 'NONE',  ( 1.000000000000000000, 0.000000000000000000, -0.000000000000000000 ) ) ;
#14499 = CARTESIAN_POINT ( 'NONE',  ( 109.4831014662949116, 20.77917954950587998, -0.7764623179268941300 ) ) ;
#14500 = CARTESIAN_POINT ( 'NONE',  ( 108.0946672814455525, 20.79497283818417230, 1.508486338784366998 ) ) ;
#14501 = AXIS2_PLACEMENT_3D ( 'NONE', #22734, #23047, #10354 ) ;
#14502 = VERTEX_POINT ( 'NONE', #11150 ) ;
#14503 = CARTESIAN_POINT ( 'NONE',  ( -58.12441765334286004, -3.826327783517069481, 5.759795199666357668 ) ) ;
#14504 = TOROIDAL_SURFACE ( 'NONE', #12913, 298.6457063863958865, 4.000000000000000888 ) ;
#14505 = ORIENTED_EDGE ( 'NONE', *, *, #3941, .F. ) ;
#14506 = CALENDAR_DATE ( 2026, 6, 10 ) ;
#14507 = CARTESIAN_POINT ( 'NONE',  ( 18.75871281239513166, -5.874329233548843732, 4.001040682667124315 ) ) ;
#14508 = CARTESIAN_POINT ( 'NONE',  ( -3.550050802731187005, 2.983565686104819648, 0.3135853898029609677 ) ) ;
#14509 = VECTOR ( 'NONE', #21547, 1000.000000000000000 ) ;
#14511 = DIRECTION ( 'NONE',  ( -1.000000000000000000, 0.000000000000000000, 0.000000000000000000 ) ) ;
#14510 = CARTESIAN_POINT ( 'NONE',  ( -34.99330891680700972, 0.1916075530515712055, -2.493613503297456901 ) ) ;
#14512 = VERTEX_POINT ( 'NONE', #18866 ) ;
#14513 = VECTOR ( 'NONE', #23467, 999.9999999999998863 ) ;
#14514 = ORIENTED_EDGE ( 'NONE', *, *, #9626, .F. ) ;
#14515 = EDGE_CURVE ( 'NONE', #26262, #4614, #24008, .T. ) ;
#14516 = AXIS2_PLACEMENT_3D ( 'NONE', #13995, #32414, #19535 ) ;
#14517 = CARTESIAN_POINT ( 'NONE',  ( 24.48499999999999943, -2.486304738420683780, 0.2613211581691335383 ) ) ;
#14518 = CARTESIAN_POINT ( 'NONE',  ( -2.162550801365593856, 2.228590825266444142, 2.752080473201636845 ) ) ;
#14519 = CIRCLE ( 'NONE', #8658, 9.000000000000001776 ) ;
#14520 = CARTESIAN_POINT ( 'NONE',  ( 23.04750000000000654, 2.594547506269380133, 0.7685399846772031918 ) ) ;
#14521 = AXIS2_PLACEMENT_3D ( 'NONE', #12997, #617, #23687 ) ;
#14522 = CARTESIAN_POINT ( 'NONE',  ( 2.896241209900578539, -11.44832573956215249, -1.500000000000036637 ) ) ;
#14524 = EDGE_LOOP ( 'NONE', ( #30134, #31987, #4510, #10430 ) ) ;
#14523 = DIRECTION ( 'NONE',  ( 0.000000000000000000, 0.000000000000000000, 1.000000000000000000 ) ) ;
#14525 = CARTESIAN_POINT ( 'NONE',  ( -2.487550801365593589, 2.752080473201636845, -2.228590825266444142 ) ) ;
#14526 = CIRCLE ( 'NONE', #143, 2.099999999999997868 ) ;
#14527 = DIRECTION ( 'NONE',  ( -1.000000000000000000, 8.574039729943015878E-17, 1.232595164407830946E-32 ) ) ;
#14528 = VECTOR ( 'NONE', #23150, 1000.000000000000000 ) ;
#14529 = CARTESIAN_POINT ( 'NONE',  ( 2.976845687893340919, -9.149921655307462487, -0.5490754078163497809 ) ) ;
#14530 = DIRECTION ( 'NONE',  ( 1.000000000000000000, -0.000000000000000000, -0.000000000000000000 ) ) ;
#14531 = AXIS2_PLACEMENT_3D ( 'NONE', #7710, #17905, #7360 ) ;
#14532 = ORIENTED_EDGE ( 'NONE', *, *, #21315, .T. ) ;
#14534 = ORIENTED_EDGE ( 'NONE', *, *, #11231, .T. ) ;
#14533 = CARTESIAN_POINT ( 'NONE',  ( 10.56870887191539587, 1.625881193364757449, -4.467071865485455540 ) ) ;
#14535 = CIRCLE ( 'NONE', #4419, 8.750000000000000000 ) ;
#14536 = CARTESIAN_POINT ( 'NONE',  ( 107.3062245775731895, 17.12232141698407517, 3.051466462891762266 ) ) ;
#14537 = CARTESIAN_POINT ( 'NONE',  ( 10.52034268205830259, -3.407865132560206511, 3.672404558090026860 ) ) ;
#14538 = CARTESIAN_POINT ( 'NONE',  ( 24.98500000136559507, -0.9349337715887247047, 3.156283516753367824 ) ) ;
#14539 = EDGE_CURVE ( 'NONE', #5929, #25797, #24627, .T. ) ;
#14540 = CARTESIAN_POINT ( 'NONE',  ( -27.92832289637407328, 17.36640870223426347, 1.500000000000000000 ) ) ;
#14541 = CARTESIAN_POINT ( 'NONE',  ( 0.7299402604449777288, -15.54820927731847569, -1.500000000000079270 ) ) ;
#14542 = CC_DESIGN_DATE_AND_TIME_ASSIGNMENT ( #5834, #26724, ( #7128 ) ) ;
#14543 = VECTOR ( 'NONE', #15322, 1000.000000000000114 ) ;
#14544 = CARTESIAN_POINT ( 'NONE',  ( 24.80656763371926843, 0.8852964313267430718, -2.499999999999998224 ) ) ;
#14545 = PRODUCT_DEFINITION_SHAPE ( 'NONE', 'NONE',  #23132 ) ;
#14546 = CONICAL_SURFACE ( 'NONE', #31147, 10.00000000000000178, 0.03490658503988666728 ) ;
#14547 = AXIS2_PLACEMENT_3D ( 'NONE', #6972, #1642, #14319 ) ;
#14548 = CARTESIAN_POINT ( 'NONE',  ( 35.33267181912139421, -4.397467831973882468, 2.184956776455081240 ) ) ;
#14549 = CARTESIAN_POINT ( 'NONE',  ( -3.337550801365593678, 1.828967928396027176, -3.368539882008727115 ) ) ;
#14550 = ORIENTED_EDGE ( 'NONE', *, *, #19634, .T. ) ;
#14551 = CARTESIAN_POINT ( 'NONE',  ( 101.6441386174529953, -1.774168274679931212, 2.184956718805492581 ) ) ;
#14552 = EDGE_LOOP ( 'NONE', ( #21905, #19283, #31393 ) ) ;
#14553 = VECTOR ( 'NONE', #28733, 1000.000000000000000 ) ;
#14554 = CIRCLE ( 'NONE', #19369, 2.999999999999999112 ) ;
#14555 = LINE ( 'NONE', #32314, #3333 ) ;
#14556 = CIRCLE ( 'NONE', #25237, 0.4500000000000007327 ) ;
#14557 = DIRECTION ( 'NONE',  ( 7.463161420169937263E-17, 2.480565909891936463E-17, 1.000000000000000000 ) ) ;
#14558 = CARTESIAN_POINT ( 'NONE',  ( 56.97280603064898941, -277.2763395528616002, 1.508259000770582059 ) ) ;
#14560 = FACE_OUTER_BOUND ( 'NONE', #31128, .T. ) ;
#14559 = AXIS2_PLACEMENT_3D ( 'NONE', #24841, #12470, #7283 ) ;
#14561 = ORIENTED_EDGE ( 'NONE', *, *, #692, .T. ) ;
#14562 = EDGE_CURVE ( 'NONE', #19632, #9004, #3291, .T. ) ;
#14563 = VECTOR ( 'NONE', #25222, 1000.000000000000000 ) ;
#14564 = CARTESIAN_POINT ( 'NONE',  ( -29.24402871571405882, -25.93932300454937945, 11.00000000000000000 ) ) ;
#14565 = ORIENTED_EDGE ( 'NONE', *, *, #14721, .F. ) ;
#14566 = DIRECTION ( 'NONE',  ( 0.000000000000000000, 0.000000000000000000, 1.000000000000000000 ) ) ;
#14567 = EDGE_CURVE ( 'NONE', #18257, #24987, #5667, .T. ) ;
#14569 = VERTEX_POINT ( 'NONE', #828 ) ;
#14568 = CARTESIAN_POINT ( 'NONE',  ( 69.01331421734823834, -4.972002658698717603, -3.996605157047315338 ) ) ;
#14570 = ORIENTED_EDGE ( 'NONE', *, *, #4084, .F. ) ;
#14571 = CARTESIAN_POINT ( 'NONE',  ( 2.678494152628110303, -8.648785596948973975, 5.187417801898995151 ) ) ;
#14572 = CARTESIAN_POINT ( 'NONE',  ( 19.03654924710325602, -2.768675503676416572, 2.713652344655541615 ) ) ;
#14574 = EDGE_LOOP ( 'NONE', ( #19990, #23908, #21783, #14452, #11607 ) ) ;
#14573 = CARTESIAN_POINT ( 'NONE',  ( 107.4297505511455313, -17.06807598898313927, 3.923214148221579656 ) ) ;
#14575 = AXIS2_PLACEMENT_3D ( 'NONE', #2854, #11005, #10842 ) ;
#14576 = CARTESIAN_POINT ( 'NONE',  ( 19.52627448105246444, 15.61656174521109364, -1.500000000000000000 ) ) ;
#14577 = CARTESIAN_POINT ( 'NONE',  ( 22.67250000000000298, -1.291182301015472600, -2.378061970571982098 ) ) ;
#14578 = VECTOR ( 'NONE', #29899, 1000.000000000000000 ) ;
#14579 = CARTESIAN_POINT ( 'NONE',  ( 7.064632918400240769, -3.647351267791623552, 7.953573330858202617 ) ) ;
#14580 = AXIS2_PLACEMENT_3D ( 'NONE', #5799, #6624, #6435 ) ;
#14581 = CARTESIAN_POINT ( 'NONE',  ( 6.784984840995218924, -5.399320162307486903, -1.500000000000000000 ) ) ;
#14583 = ORIENTED_EDGE ( 'NONE', *, *, #20393, .T. ) ;
#14582 = CARTESIAN_POINT ( 'NONE',  ( 107.5536565100458830, -18.86584003217233629, -4.757788453915527960 ) ) ;
#14584 = DIRECTION ( 'NONE',  ( -0.000000000000000000, 0.000000000000000000, 1.000000000000000000 ) ) ;
#14585 = CIRCLE ( 'NONE', #199, 6.248999999999998778 ) ;
#14586 = CIRCLE ( 'NONE', #200, 6.999999999999998224 ) ;
#14587 = PLANE ( 'NONE',  #2763 ) ;
#14588 = CARTESIAN_POINT ( 'NONE',  ( 24.29750000136559507, -0.3178988483021076838, -3.024605502323848949 ) ) ;
#14589 = DIRECTION ( 'NONE',  ( 0.000000000000000000, 1.000000000000000000, 0.000000000000000000 ) ) ;
#14590 = FACE_OUTER_BOUND ( 'NONE', #29837, .T. ) ;
#14591 = PLANE ( 'NONE',  #20390 ) ;
#14592 = DIRECTION ( 'NONE',  ( 0.000000000000000000, -0.9063077870366440525, -0.4226182617407121533 ) ) ;
#14593 = ORIENTED_EDGE ( 'NONE', *, *, #23857, .F. ) ;
#14594 = CARTESIAN_POINT ( 'NONE',  ( 7.064632940817594076, -4.973063321323921926, 7.199384779417104419 ) ) ;
#14595 = CARTESIAN_POINT ( 'NONE',  ( 110.5397548702477764, 21.00556809464029939, -2.806473568333519353 ) ) ;
#14596 = CARTESIAN_POINT ( 'NONE',  ( -5.427698642335591239E-12, -21.93932300456189566, 1.500000000000000000 ) ) ;
#14597 = ORIENTED_EDGE ( 'NONE', *, *, #14515, .F. ) ;
#14598 = CARTESIAN_POINT ( 'NONE',  ( 8.911384905465473238, 0.2172754300402908179, -1.412391582771881371 ) ) ;
#14599 = CARTESIAN_POINT ( 'NONE',  ( 108.4615897723380868, -15.55450498649102720, -0.9788672205888330202 ) ) ;
#14600 = VERTEX_POINT ( 'NONE', #11328 ) ;
#14601 = DIRECTION ( 'NONE',  ( -6.062761635205638616E-17, -0.7071067811865540120, 0.7071067811865410224 ) ) ;
#14602 = EDGE_CURVE ( 'NONE', #23931, #22574, #21538, .T. ) ;
#14603 = ORIENTED_EDGE ( 'NONE', *, *, #29343, .F. ) ;
#14604 = CIRCLE ( 'NONE', #1813, 5.100000000000000533 ) ;
#14606 = ADVANCED_FACE ( 'NONE', ( #3329 ), #11004, .T. ) ;
#14605 = VECTOR ( 'NONE', #5997, 1000.000000000000000 ) ;
#14607 = ORIENTED_EDGE ( 'NONE', *, *, #7480, .F. ) ;
#14608 = DIRECTION ( 'NONE',  ( 0.000000000000000000, 0.000000000000000000, 1.000000000000000000 ) ) ;
#14610 = ORIENTED_EDGE ( 'NONE', *, *, #1746, .T. ) ;
#14609 = CARTESIAN_POINT ( 'NONE',  ( -59.84585868070823267, -5.753144558333701752, 1.949999999999999956 ) ) ;
#14611 = ORIENTED_EDGE ( 'NONE', *, *, #16946, .F. ) ;
#14612 = CARTESIAN_POINT ( 'NONE',  ( 24.29750000136559507, -0.3178988483021076838, -3.024605502323848949 ) ) ;
#14613 = LOCAL_TIME ( 16, 7, 10.00000000000000000, #10294 ) ;
#14614 = ORIENTED_EDGE ( 'NONE', *, *, #23158, .T. ) ;
#14615 = FACE_OUTER_BOUND ( 'NONE', #1147, .T. ) ;
#14617 = ORIENTED_EDGE ( 'NONE', *, *, #10745, .F. ) ;
#14616 = CARTESIAN_POINT ( 'NONE',  ( 102.2651039925858072, -1.731228206879547704, -2.184956770111041280 ) ) ;
#14618 = CARTESIAN_POINT ( 'NONE',  ( -56.48155856471830560, 0.04209818965781165351, -1.019622293805160007 ) ) ;
#14619 = DIRECTION ( 'NONE',  ( -1.000000000000000000, -0.000000000000000000, 1.387778780781444256E-14 ) ) ;
#14620 = CARTESIAN_POINT ( 'NONE',  ( 23.98500000136559507, -2.892927487894331406, 1.570731468192932301 ) ) ;
#14621 = CARTESIAN_POINT ( 'NONE',  ( 108.1293191352079361, -19.93152549158542897, 2.509206947344208238 ) ) ;
#14622 = AXIS2_PLACEMENT_3D ( 'NONE', #30663, #10052, #20266 ) ;
#14623 = AXIS2_PLACEMENT_3D ( 'NONE', #1622, #11813, #16836 ) ;
#14624 = CARTESIAN_POINT ( 'NONE',  ( -0.7867377105085294753, -2.707992247746929149, -5.485967528433937979 ) ) ;
#14625 = CARTESIAN_POINT ( 'NONE',  ( -1.433134780067091442E-16, -9.620177616658022401, 5.227991826304056566 ) ) ;
#14626 = CARTESIAN_POINT ( 'NONE',  ( 0.3749740905863481744, 7.612528756000837227, -6.632019415960804132 ) ) ;
#14627 = EDGE_CURVE ( 'NONE', #30284, #21159, #11086, .T. ) ;
#14628 = DIRECTION ( 'NONE',  ( 4.917867153432943562E-17, 0.5735764363510392760, 0.8191520442889966835 ) ) ;
#14629 = CARTESIAN_POINT ( 'NONE',  ( 110.2779561444949223, -18.44184597392422020, 5.485967528433935314 ) ) ;
#14630 = FACE_OUTER_BOUND ( 'NONE', #8215, .T. ) ;
#14631 = FACE_OUTER_BOUND ( 'NONE', #10943, .T. ) ;
#14632 = APPROVAL_PERSON_ORGANIZATION ( #20021, #7567, #27840 ) ;
#14633 = DIRECTION ( 'NONE',  ( 1.000000000000000000, 0.000000000000000000, 0.000000000000000000 ) ) ;
#14634 = CARTESIAN_POINT ( 'NONE',  ( -6.250050802731187183, -1.887961173149512062, -2.331437884370912261 ) ) ;
#14635 = ORIENTED_EDGE ( 'NONE', *, *, #9124, .F. ) ;
#14636 = CARTESIAN_POINT ( 'NONE',  ( -2.950050800000000528, -0.9222479816126459840, -3.113457007523259268 ) ) ;
#14637 = EDGE_CURVE ( 'NONE', #30629, #4825, #21949, .T. ) ;
#14638 = DIRECTION ( 'NONE',  ( 0.000000000000000000, -1.000000000000000000, 0.000000000000000000 ) ) ;
#14639 = ORIENTED_EDGE ( 'NONE', *, *, #5664, .F. ) ;
#14640 = CARTESIAN_POINT ( 'NONE',  ( 0.000000000000000000, 0.000000000000000000, 0.000000000000000000 ) ) ;
#14641 = FACE_OUTER_BOUND ( 'NONE', #11406, .T. ) ;
#14642 = EDGE_CURVE ( 'NONE', #29668, #23825, #18236, .T. ) ;
#14643 = VECTOR ( 'NONE', #18119, 1000.000000000000000 ) ;
#14644 = B_SPLINE_CURVE_WITH_KNOTS ( 'NONE', 3,
 ( #11831, #9478, #1484, #19693, #14675, #30082, #11660, #21856, #17177, #32071 ),
 .UNSPECIFIED., .F., .F.,
 ( 4, 2, 2, 2, 4 ),
 ( 1.968338519010298316E-07, 0.0005467927057105484217, 0.001093388577569195854, 0.001639984449427843395, 0.002186580321286489201 ),
 .UNSPECIFIED. ) ;
#14645 = ORIENTED_EDGE ( 'NONE', *, *, #18703, .T. ) ;
#14646 = CARTESIAN_POINT ( 'NONE',  ( 101.7777806943559114, -3.698580936114888917, -4.282223226319369580 ) ) ;
#14647 = MECHANICAL_CONTEXT ( 'NONE', #19317, 'mechanical' ) ;
#14649 = EDGE_CURVE ( 'NONE', #17768, #29452, #16067, .T. ) ;
#14648 = CARTESIAN_POINT ( 'NONE',  ( 6.356382477965130562, 5.959271875177152289, 6.209963745178032291 ) ) ;
#14650 = VERTEX_POINT ( 'NONE', #11814 ) ;
#14651 = CARTESIAN_POINT ( 'NONE',  ( 3.249999999999999556, 8.152713396088763886, 3.174628368996105010 ) ) ;
#14652 = CARTESIAN_POINT ( 'NONE',  ( -29.24402871571405882, -27.93932300454937590, 11.00000000000000000 ) ) ;
#14653 = CARTESIAN_POINT ( 'NONE',  ( 85.03270493638194694, -5.154008962840147312, -4.074609222412457932 ) ) ;
#14654 = CARTESIAN_POINT ( 'NONE',  ( 1.624999999999999778, -9.915734732513186600, -4.762163868918378284 ) ) ;
#14655 = LINE ( 'NONE', #12141, #11241 ) ;
#14656 = ORIENTED_EDGE ( 'NONE', *, *, #18117, .T. ) ;
#14657 = EDGE_CURVE ( 'NONE', #17282, #1891, #20300, .T. ) ;
#14658 = DIRECTION ( 'NONE',  ( 7.770718973609008239E-17, 0.9063077870366537114, -0.4226182617406915032 ) ) ;
#14659 = CARTESIAN_POINT ( 'NONE',  ( 22.98163386837276434, -21.92547295135298313, -1.118948288781295153 ) ) ;
#14660 = CARTESIAN_POINT ( 'NONE',  ( 101.7264006491828638, -2.958721067370967184, 4.091315454821516262 ) ) ;
#14662 = ORIENTED_EDGE ( 'NONE', *, *, #822, .F. ) ;
#14661 = FACE_OUTER_BOUND ( 'NONE', #30042, .T. ) ;
#14663 = CARTESIAN_POINT ( 'NONE',  ( 108.1033629032233847, 18.75372535508294902, -4.515627687203030760 ) ) ;
#14664 = LINE ( 'NONE', #12151, #6413 ) ;
#14665 = CARTESIAN_POINT ( 'NONE',  ( 4.749760686538667009, -1.391664247347174754, -7.892520144992448472 ) ) ;
#14666 = EDGE_CURVE ( 'NONE', #18809, #4208, #32137, .T. ) ;
#14667 = DIRECTION ( 'NONE',  ( -0.000000000000000000, -0.000000000000000000, -1.000000000000000000 ) ) ;
#14668 = CARTESIAN_POINT ( 'NONE',  ( -34.98223484310472031, 0.5000000000000000000, 2.552009564962238297 ) ) ;
#14669 = CARTESIAN_POINT ( 'NONE',  ( 7.249760686538667009, 0.7071067811865129338, 8.721381771256208282 ) ) ;
#14670 = VECTOR ( 'NONE', #26452, 1000.000000000000000 ) ;
#14671 = CARTESIAN_POINT ( 'NONE',  ( 7.249760686538667009, 0.000000000000000000, 0.000000000000000000 ) ) ;
#14672 = CARTESIAN_POINT ( 'NONE',  ( 4.499760686538666121, 0.000000000000000000, 0.000000000000000000 ) ) ;
#14673 = ORIENTED_EDGE ( 'NONE', *, *, #20235, .T. ) ;
#14674 = EDGE_CURVE ( 'NONE', #29424, #24311, #14157, .T. ) ;
#14675 = CARTESIAN_POINT ( 'NONE',  ( 6.357667873252798252, 2.398098878660953392, 8.266402141659449754 ) ) ;
#14676 = EDGE_LOOP ( 'NONE', ( #30243, #27358, #27608, #32971, #16665 ) ) ;
#14677 = CARTESIAN_POINT ( 'NONE',  ( -6.404531657079157725, -2.325406398514293205, 1.883076972206379818 ) ) ;
#14678 = CARTESIAN_POINT ( 'NONE',  ( 108.8978791464556508, 17.52043075494136204, 4.999054092451758358 ) ) ;
#14679 = CARTESIAN_POINT ( 'NONE',  ( 18.87102749435251425, -4.618876501924994216, -5.695980980372493008 ) ) ;
#14680 = EDGE_CURVE ( 'NONE', #27411, #15557, #25710, .T. ) ;
#14681 = DIRECTION ( 'NONE',  ( -1.000000000000000000, 0.000000000000000000, 0.000000000000000000 ) ) ;
#14682 = CARTESIAN_POINT ( 'NONE',  ( 2.281627749324421917, -0.2935656086769610207, 1.757435426329174044 ) ) ;
#14683 = ORIENTED_EDGE ( 'NONE', *, *, #12640, .F. ) ;
#14684 = LINE ( 'NONE', #19702, #19375 ) ;
#14685 = EDGE_CURVE ( 'NONE', #2615, #17109, #26873, .T. ) ;
#14686 =( BOUNDED_SURFACE ( )  B_SPLINE_SURFACE ( 3, 3, ( 
 ( #6929, #12275, #25339, #9438, #17128, #1951, #32703, #12123 ),
 ( #27664, #2272, #5112, #15627, #10096, #25844, #18125, #30713 ),
 ( #13118, #2962, #278, #13263, #2771, #18472, #28664, #25652 ),
 ( #10450, #15289, #7607, #10602, #28165, #28514, #12764, #3109 ) ),
 .UNSPECIFIED., .F., .F., .F. ) 
 B_SPLINE_SURFACE_WITH_KNOTS ( ( 4, 4 ),
 ( 4, 2, 2, 4 ),
 ( 0.000000000000000000, 1.000000000000000000 ),
 ( 0.000000000000000000, 0.5000000000000000000, 0.7500000000000000000, 1.000000000000000000 ),
 .UNSPECIFIED. ) 
 GEOMETRIC_REPRESENTATION_ITEM ( )  RATIONAL_B_SPLINE_SURFACE ( (
 ( 1.000000000000000000, 1.000000000000000000, 1.000000000000000000, 1.000000000000000000, 1.000000000000000000, 1.000000000000000000, 1.000000000000000000, 1.000000000000000000),
 ( 0.6857970438836927807, 0.6857970438836927807, 0.6857970438836927807, 0.6857970438836927807, 0.6857970438836927807, 0.6857970438836927807, 0.6857970438836927807, 0.6857970438836927807),
 ( 0.6857970438836927807, 0.6857970438836927807, 0.6857970438836927807, 0.6857970438836927807, 0.6857970438836927807, 0.6857970438836927807, 0.6857970438836927807, 0.6857970438836927807),
 ( 1.000000000000000000, 1.000000000000000000, 1.000000000000000000, 1.000000000000000000, 1.000000000000000000, 1.000000000000000000, 1.000000000000000000, 1.000000000000000000) ) ) 
 REPRESENTATION_ITEM ( '' )  SURFACE ( )  );
#14687 = ORIENTED_EDGE ( 'NONE', *, *, #10526, .F. ) ;
#14688 = PERSON_AND_ORGANIZATION ( #6766, #25292 ) ;
#14689 = CARTESIAN_POINT ( 'NONE',  ( 28.66430776624534715, -6.757211549878646473, 4.006107076289154634 ) ) ;
#14690 = FACE_OUTER_BOUND ( 'NONE', #15454, .T. ) ;
#14692 = CARTESIAN_POINT ( 'NONE',  ( 7.064423539573519761, -0.7071067811874917064, -8.721381771257252780 ) ) ;
#14691 = CARTESIAN_POINT ( 'NONE',  ( 5.377543748152548098, 6.940565734314597002, 4.007137495034836405 ) ) ;
#14693 = EDGE_LOOP ( 'NONE', ( #13244, #25629, #17446, #24275 ) ) ;
#14694 = CARTESIAN_POINT ( 'NONE',  ( 6.038145268433182444, 6.194606843114086381, 5.783741681378098853 ) ) ;
#14695 = CARTESIAN_POINT ( 'NONE',  ( 6.356382399260311900, -7.723816458760322412, -3.797266095948563347 ) ) ;
#14696 = CARTESIAN_POINT ( 'NONE',  ( 25.29750000136559507, -2.363507492473152283, -1.913930629741525280 ) ) ;
#14697 = EDGE_CURVE ( 'NONE', #24965, #29752, #29721, .T. ) ;
#14698 = CARTESIAN_POINT ( 'NONE',  ( 0.1512968795556346446, -7.218651089666939136, -1.774506416594164637 ) ) ;
#14700 = ORIENTED_EDGE ( 'NONE', *, *, #23360, .T. ) ;
#14699 = CARTESIAN_POINT ( 'NONE',  ( 107.5137442065068996, 18.28919312501354710, 5.093186791727767115 ) ) ;
#14701 = CARTESIAN_POINT ( 'NONE',  ( -2.287550801365593856, 2.228590825266444142, 2.752080473201636845 ) ) ;
#14702 = CARTESIAN_POINT ( 'NONE',  ( 18.96044790064761898, -3.619335823787583006, -0.07017451552783579571 ) ) ;
#14703 = CARTESIAN_POINT ( 'NONE',  ( -57.40374817251313999, -2.616512360834426953, 5.500000000000000000 ) ) ;
#14704 = PLANE ( 'NONE',  #12463 ) ;
#14705 = ORIENTED_EDGE ( 'NONE', *, *, #18607, .F. ) ;
#14707 = VERTEX_POINT ( 'NONE', #6457 ) ;
#14706 = CARTESIAN_POINT ( 'NONE',  ( -15.02135460118491217, -21.93013659628234890, 1.095404497688272638 ) ) ;
#14708 = DIRECTION ( 'NONE',  ( 1.000000000000000000, 0.000000000000000000, 0.000000000000000000 ) ) ;
#14709 = B_SPLINE_CURVE_WITH_KNOTS ( 'NONE', 3,
 ( #5585, #25970, #10069, #30486, #7571, #27982, #5083, #23603, #10912, #1208 ),
 .UNSPECIFIED., .F., .F.,
 ( 4, 2, 2, 2, 4 ),
 ( 3.512955445812634541E-07, 0.0005479535487286800108, 0.001095555801912778812, 0.001643158055096877613, 0.002190760308280976631 ),
 .UNSPECIFIED. ) ;
#14710 = DIRECTION ( 'NONE',  ( 1.706601815529740836E-15, 0.000000000000000000, 1.000000000000000000 ) ) ;
#14711 = CARTESIAN_POINT ( 'NONE',  ( -16.91347898512169934, 12.16064947808539998, 1.928605623396539404 ) ) ;
#14712 = DIRECTION ( 'NONE',  ( -0.000000000000000000, -0.000000000000000000, -1.000000000000000000 ) ) ;
#14713 = CARTESIAN_POINT ( 'NONE',  ( 0.8027523773784053240, -15.44646927475563913, -1.746109446251894681 ) ) ;
#14714 = CARTESIAN_POINT ( 'NONE',  ( 6.357667975083867162, 7.150591204917396304, 4.790963222208030281 ) ) ;
#14715 = ADVANCED_FACE ( 'NONE', ( #3990 ), #12142, .F. ) ;
#14716 = CARTESIAN_POINT ( 'NONE',  ( 41.34428855215830367, -4.040999237037259384, 1.169951068917443049 ) ) ;
#14717 = CARTESIAN_POINT ( 'NONE',  ( 29.21519671786122885, -8.552672223064927692, 2.713652344655544724 ) ) ;
#14718 = ORIENTED_EDGE ( 'NONE', *, *, #22277, .F. ) ;
#14719 = DIRECTION ( 'NONE',  ( -1.000000000000000000, 0.000000000000000000, 0.000000000000000000 ) ) ;
#14720 = ORIENTED_EDGE ( 'NONE', *, *, #15276, .F. ) ;
#14721 = EDGE_CURVE ( 'NONE', #2170, #6161, #10750, .T. ) ;
#14722 = CARTESIAN_POINT ( 'NONE',  ( 3.063284526842892319, -5.538577986798981279, -6.772677083981775148 ) ) ;
#14723 = SHAPE_REPRESENTATION_RELATIONSHIP ( 'NONE' , 'NONE' ,  #13478, #10724 ) ;
#14724 = CARTESIAN_POINT ( 'NONE',  ( 0.000000000000000000, 0.000000000000000000, 0.000000000000000000 ) ) ;
#14725 = ORIENTED_EDGE ( 'NONE', *, *, #10345, .T. ) ;
#14726 = CARTESIAN_POINT ( 'NONE',  ( 107.6641398346957033, -20.45810202417174750, 1.500000000000000000 ) ) ;
#14727 = ORIENTED_EDGE ( 'NONE', *, *, #12064, .F. ) ;
#14728 = FACE_OUTER_BOUND ( 'NONE', #26731, .T. ) ;
#14730 = ORIENTED_EDGE ( 'NONE', *, *, #17868, .F. ) ;
#14729 = CARTESIAN_POINT ( 'NONE',  ( 84.96607275259252390, -4.067036972963657071, -4.006106264892282276 ) ) ;
#14731 = ORIENTED_EDGE ( 'NONE', *, *, #9517, .F. ) ;
#14732 = FACE_OUTER_BOUND ( 'NONE', #28691, .T. ) ;
#14733 = EDGE_CURVE ( 'NONE', #4619, #22777, #7591, .T. ) ;
#14734 = CARTESIAN_POINT ( 'NONE',  ( 47.99002579008096347, -3.080023785605708220, 1.915219082070892531 ) ) ;
#14735 = CC_DESIGN_DATE_AND_TIME_ASSIGNMENT ( #28384, #15987, ( #10350 ) ) ;
#14737 = ORIENTED_EDGE ( 'NONE', *, *, #13212, .F. ) ;
#14736 = CARTESIAN_POINT ( 'NONE',  ( -4.555597372409920354, -6.492899504186820714, -1.500000000000000666 ) ) ;
#14738 = CARTESIAN_POINT ( 'NONE',  ( 21.53922796458296318, 16.55061608804989604, -1.050000000000000044 ) ) ;
#14739 = CARTESIAN_POINT ( 'NONE',  ( 9.236821176939058020, 0.1505923090604457948, -1.036667534179769756 ) ) ;
#14740 = CARTESIAN_POINT ( 'NONE',  ( -17.45597128428593336, -27.93932300454937590, 11.00000000000000000 ) ) ;
#14741 = CARTESIAN_POINT ( 'NONE',  ( 8.060276137098751903, -2.738905750062150535, -1.000000000000000000 ) ) ;
#14743 = VERTEX_POINT ( 'NONE', #15784 ) ;
#14742 = CARTESIAN_POINT ( 'NONE',  ( 107.9496129882747937, -17.34380168244590337, -4.567365599077690241 ) ) ;
#14744 = CARTESIAN_POINT ( 'NONE',  ( 2.437082427505614657, -9.703015696712927962, -4.432669656489585108 ) ) ;
#14745 = CARTESIAN_POINT ( 'NONE',  ( 23.42250000273119070, 1.291182301015469047, 2.378061970571981654 ) ) ;
#14746 = DIRECTION ( 'NONE',  ( -0.000000000000000000, -0.000000000000000000, -1.000000000000000000 ) ) ;
#14747 = EDGE_CURVE ( 'NONE', #15147, #4279, #25177, .T. ) ;
#14748 = CARTESIAN_POINT ( 'NONE',  ( 108.2917183403186812, 19.80256275033599778, -2.304437341803263095 ) ) ;
#14749 = CARTESIAN_POINT ( 'NONE',  ( 12.44989959798879831, -0.06979899340500890503, 1.001218345961853107 ) ) ;
#14750 = CARTESIAN_POINT ( 'NONE',  ( 0.000000000000000000, 5.222868219166857173, 9.680994141368786998 ) ) ;
#14751 =( BOUNDED_SURFACE ( )  B_SPLINE_SURFACE ( 3, 3, ( 
 ( #27612, #15057, #2391, #19598, #4206, #4714, #17060, #14883 ),
 ( #27458, #12218, #12563, #28610, #30952, #3197, #20753, #13206 ),
 ( #28260, #15555, #8033, #513, #17743, #18233, #20255, #18069 ),
 ( #10209, #20432, #15234, #3052, #22917, #5369, #28446, #15739 ) ),
 .UNSPECIFIED., .F., .F., .F. ) 
 B_SPLINE_SURFACE_WITH_KNOTS ( ( 4, 4 ),
 ( 4, 2, 2, 4 ),
 ( 0.000000000000000000, 1.000000000000000000 ),
 ( 0.000000000000000000, 0.5000000000000000000, 0.7500000000000000000, 1.000000000000000000 ),
 .UNSPECIFIED. ) 
 GEOMETRIC_REPRESENTATION_ITEM ( )  RATIONAL_B_SPLINE_SURFACE ( (
 ( 1.000000000000000000, 1.000000000000000000, 1.000000000000000000, 1.000000000000000000, 1.000000000000000000, 1.000000000000000000, 1.000000000000000000, 1.000000000000000000),
 ( 0.9743068154145675397, 0.9743068154145675397, 0.9743068154145675397, 0.9743068154145675397, 0.9743068154145675397, 0.9743068154145675397, 0.9743068154145675397, 0.9743068154145675397),
 ( 0.9743068154145675397, 0.9743068154145675397, 0.9743068154145675397, 0.9743068154145675397, 0.9743068154145675397, 0.9743068154145675397, 0.9743068154145675397, 0.9743068154145675397),
 ( 1.000000000000000000, 1.000000000000000000, 1.000000000000000000, 1.000000000000000000, 1.000000000000000000, 1.000000000000000000, 1.000000000000000000, 1.000000000000000000) ) ) 
 REPRESENTATION_ITEM ( '' )  SURFACE ( )  );
#14752 = ORIENTED_EDGE ( 'NONE', *, *, #11395, .T. ) ;
#14753 = CARTESIAN_POINT ( 'NONE',  ( -12.44989959798873791, 0.5174497483512504603, -2.981930256614258923 ) ) ;
#14754 = EDGE_CURVE ( 'NONE', #32366, #27630, #29450, .T. ) ;
#14755 = DIRECTION ( 'NONE',  ( -0.000000000000000000, 0.000000000000000000, 1.000000000000000000 ) ) ;
#14756 = CARTESIAN_POINT ( 'NONE',  ( -6.837550801365592790, -3.675193018007245627, 1.088641768524163389 ) ) ;
#14757 = VERTEX_POINT ( 'NONE', #30700 ) ;
#14758 = DIRECTION ( 'NONE',  ( 0.000000000000000000, 0.000000000000000000, -1.000000000000000000 ) ) ;
#14759 = CARTESIAN_POINT ( 'NONE',  ( 2.454674724652319728, -0.02938977324472418981, -1.729574810602341861 ) ) ;
#14760 = ORIENTED_EDGE ( 'NONE', *, *, #7785, .T. ) ;
#14761 = CARTESIAN_POINT ( 'NONE',  ( 107.6996442589674103, 19.35565155597527109, 4.629213727441584325 ) ) ;
#14762 = ORIENTED_EDGE ( 'NONE', *, *, #17033, .T. ) ;
#14763 = VERTEX_POINT ( 'NONE', #23624 ) ;
#14764 = B_SPLINE_CURVE_WITH_KNOTS ( 'NONE', 3,
 ( #10143, #14500, #20202, #14989, #20364, #30398 ),
 .UNSPECIFIED., .F., .F.,
 ( 4, 2, 4 ),
 ( 0.000000000000000000, 0.0003973515176470922890, 0.0007947030352941845781 ),
 .UNSPECIFIED. ) ;
#14765 = CARTESIAN_POINT ( 'NONE',  ( -15.02135460118491217, -21.93013659628234890, 1.095404497688272638 ) ) ;
#14767 = ORIENTED_EDGE ( 'NONE', *, *, #16195, .F. ) ;
#14766 = LINE ( 'NONE', #27490, #28280 ) ;
#14768 = VERTEX_POINT ( 'NONE', #410 ) ;
#14769 = CARTESIAN_POINT ( 'NONE',  ( 23.11000000136559862, -3.156283516753370488, -0.9349337715887220401 ) ) ;
#14770 = ORIENTED_EDGE ( 'NONE', *, *, #16566, .F. ) ;
#14771 = FACE_OUTER_BOUND ( 'NONE', #20193, .T. ) ;
#14773 = ORIENTED_EDGE ( 'NONE', *, *, #9604, .T. ) ;
#14772 = CARTESIAN_POINT ( 'NONE',  ( 47.88685968122761238, -4.079890078783551921, -1.529339664923148323 ) ) ;
#14774 = CARTESIAN_POINT ( 'NONE',  ( 5.834205823644816213, 18.00000000000000355, 2.241549108841682791 ) ) ;
#14775 = CARTESIAN_POINT ( 'NONE',  ( 3.499999999999999556, 0.000000000000000000, 0.000000000000000000 ) ) ;
#14776 = CARTESIAN_POINT ( 'NONE',  ( 23.67250000136559507, 2.363507492473148286, 1.913930629741525058 ) ) ;
#14777 = CARTESIAN_POINT ( 'NONE',  ( 3.499999999999999556, -6.700937042937042065, -2.183447440113257976 ) ) ;
#14778 = CARTESIAN_POINT ( 'NONE',  ( -34.48223484310472742, 0.5000000000000000000, -2.982234843104710986 ) ) ;
#14779 = DIRECTION ( 'NONE',  ( -0.000000000000000000, -0.000000000000000000, 1.000000000000000000 ) ) ;
#14780 = FACE_OUTER_BOUND ( 'NONE', #3045, .T. ) ;
#14781 = EDGE_CURVE ( 'NONE', #2615, #11560, #2231, .T. ) ;
#14782 = ADVANCED_FACE ( 'NONE', ( #25479 ), #13107, .T. ) ;
#14783 = CARTESIAN_POINT ( 'NONE',  ( -1.152183934781129714E-14, 21.49000000000002331, 1.050000000000000044 ) ) ;
#14784 = FACE_BOUND ( 'NONE', #29541, .T. ) ;
#14785 = CARTESIAN_POINT ( 'NONE',  ( -5.323856294847543857, 1.496472198897157213, -3.277537277937041527 ) ) ;
#14786 = CARTESIAN_POINT ( 'NONE',  ( 29.27523314209665983, -3.695744416148424527, -0.02339150518254430253 ) ) ;
#14787 = EDGE_CURVE ( 'NONE', #15872, #25625, #1934, .T. ) ;
#14788 = DIRECTION ( 'NONE',  ( -3.469446951953478110E-15, 0.000000000000000000, 1.000000000000000000 ) ) ;
#14789 = CARTESIAN_POINT ( 'NONE',  ( -4.050050802731187005, -2.331437884370912705, 1.887961173149512062 ) ) ;
#14790 = ORIENTED_EDGE ( 'NONE', *, *, #17611, .T. ) ;
#14791 = CARTESIAN_POINT ( 'NONE',  ( -4.750050800000000351, -3.113457007523259268, 0.9222479816126455399 ) ) ;
#14792 = CARTESIAN_POINT ( 'NONE',  ( 107.2582456157670805, 16.85513498755496542, -2.462483528952394529 ) ) ;
#14793 = DIRECTION ( 'NONE',  ( 1.000000000000000000, -8.574039729943018344E-17, -0.000000000000000000 ) ) ;
#14794 = ORIENTED_EDGE ( 'NONE', *, *, #9279, .T. ) ;
#14795 = CARTESIAN_POINT ( 'NONE',  ( -2.150050802731187538, 0.3135853898029611342, -2.983565686104819648 ) ) ;
#14796 = CARTESIAN_POINT ( 'NONE',  ( 0.000000000000000000, 0.000000000000000000, 0.000000000000000000 ) ) ;
#14797 = ORIENTED_EDGE ( 'NONE', *, *, #11804, .T. ) ;
#14798 = DIRECTION ( 'NONE',  ( -0.000000000000000000, 0.000000000000000000, 1.000000000000000000 ) ) ;
#14799 = APPROVAL_STATUS ( 'not_yet_approved' ) ;
#14800 = CARTESIAN_POINT ( 'NONE',  ( -2.900050800000000706, 0.3135853898029611342, -2.983565686104819648 ) ) ;
#14801 = VERTEX_POINT ( 'NONE', #10436 ) ;
#14802 = CARTESIAN_POINT ( 'NONE',  ( 28.69360035300382705, -5.615748452717688188, 3.993434336046830513 ) ) ;
#14803 = ORIENTED_EDGE ( 'NONE', *, *, #21018, .T. ) ;
#14804 = DIRECTION ( 'NONE',  ( 0.000000000000000000, -1.000000000000000000, 0.000000000000000000 ) ) ;
#14805 = CARTESIAN_POINT ( 'NONE',  ( 9.256647899302816285, 0.1794474037904786601, -1.452724983837345718 ) ) ;
#14806 = CARTESIAN_POINT ( 'NONE',  ( -34.99744630603539974, 0.5000000000000000000, 2.982419344533008498 ) ) ;
#14807 = CARTESIAN_POINT ( 'NONE',  ( -23.54713438637982748, 8.429255322705477838, 8.219131494323725917 ) ) ;
#14808 = ORIENTED_EDGE ( 'NONE', *, *, #22094, .F. ) ;
#14809 = CARTESIAN_POINT ( 'NONE',  ( 22.80257615841729191, -21.89069152845288713, -1.310091664434587022 ) ) ;
#14810 = CARTESIAN_POINT ( 'NONE',  ( 101.7539407721759801, -3.355291987352425842, 4.312036717242840211 ) ) ;
#14811 = EDGE_CURVE ( 'NONE', #9859, #6440, #23451, .T. ) ;
#14813 = ORIENTED_EDGE ( 'NONE', *, *, #5919, .F. ) ;
#14812 = FACE_OUTER_BOUND ( 'NONE', #8341, .T. ) ;
#14814 = CARTESIAN_POINT ( 'NONE',  ( 5.489344087273877015, -6.152099123112487078, 5.297876218488298150 ) ) ;
#14815 = CARTESIAN_POINT ( 'NONE',  ( 5.489321676144490958, -3.969109389279916744, -7.082488557107332383 ) ) ;
#14816 = CARTESIAN_POINT ( 'NONE',  ( 4.749760686538667009, -6.940565734314625423, 4.007137495034787555 ) ) ;
#14817 = FACE_OUTER_BOUND ( 'NONE', #5990, .T. ) ;
#14818 = CARTESIAN_POINT ( 'NONE',  ( -8.000050800000000351, 2.947991532268304127, 1.750383400925231703 ) ) ;
#14819 = DIRECTION ( 'NONE',  ( 1.000000000000000000, 0.000000000000000000, -0.000000000000000000 ) ) ;
#14820 = CARTESIAN_POINT ( 'NONE',  ( -56.29156811815547456, 0.01555455218834706291, -1.127217129886184832 ) ) ;
#14821 = DIRECTION ( 'NONE',  ( 1.000000000000000000, -5.637851296924461498E-14, 0.000000000000000000 ) ) ;
#14822 = EDGE_LOOP ( 'NONE', ( #1249, #21627, #10924, #17763 ) ) ;
#14823 = CARTESIAN_POINT ( 'NONE',  ( -8.062550801365594211, 0.3701630799359330593, -3.521866450007987037 ) ) ;
#14824 = EDGE_LOOP ( 'NONE', ( #5830, #31761, #32571, #14904 ) ) ;
#14825 = CARTESIAN_POINT ( 'NONE',  ( -8.104531657079158791, -0.3127741368606806738, 2.975847129947406522 ) ) ;
#14826 = CARTESIAN_POINT ( 'NONE',  ( 25.92250000136559507, 0.3178988483021036315, 3.024605502323848949 ) ) ;
#14827 = CARTESIAN_POINT ( 'NONE',  ( 85.33608266635167183, -5.304379108986591262, -5.695980980372493008 ) ) ;
#14828 = CARTESIAN_POINT ( 'NONE',  ( 29.21519671786122885, -8.552672223070194590, -2.713652344655543391 ) ) ;
#14829 = DIRECTION ( 'NONE',  ( 0.000000000000000000, 0.000000000000000000, 1.000000000000000000 ) ) ;
#14830 = VERTEX_POINT ( 'NONE', #20487 ) ;
#14831 = DIRECTION ( 'NONE',  ( 1.000000000000000000, -0.000000000000000000, -0.000000000000000000 ) ) ;
#14832 = ORIENTED_EDGE ( 'NONE', *, *, #9517, .T. ) ;
#14833 = CARTESIAN_POINT ( 'NONE',  ( 6.037141812302425414, 1.911013226338409199, 8.256172215043582341 ) ) ;
#14834 = DATE_TIME_ROLE ( 'creation_date' ) ;
#14835 = CARTESIAN_POINT ( 'NONE',  ( 54.97676626710897096, -6.490013410911064540, 4.018750264949940032 ) ) ;
#14836 = CARTESIAN_POINT ( 'NONE',  ( -56.30345176035514498, 0.06347132377568256989, -1.252366240086452365 ) ) ;
#14838 = CARTESIAN_POINT ( 'NONE',  ( 25.75999999999999801, -2.208672634433321348E-15, 0.000000000000000000 ) ) ;
#14837 = CARTESIAN_POINT ( 'NONE',  ( 6.524595551582240915, 7.790581746767737847, 3.779376390944498620 ) ) ;
#14839 = EDGE_CURVE ( 'NONE', #24091, #19481, #27853, .T. ) ;
#14840 = ORIENTED_EDGE ( 'NONE', *, *, #7553, .F. ) ;
#14841 = CARTESIAN_POINT ( 'NONE',  ( 1.624999999999999778, -10.82112760146737962, 1.975651141462197113 ) ) ;
#14842 = CARTESIAN_POINT ( 'NONE',  ( -41.30970132048468457, -16.45499999999997343, 0.000000000000000000 ) ) ;
#14843 = CARTESIAN_POINT ( 'NONE',  ( 24.86000000136559862, 1.570731468192929858, 2.892927487894329186 ) ) ;
#14844 = CARTESIAN_POINT ( 'NONE',  ( 0.5290670167336711804, -6.525914665286372873, -1.500000000000000444 ) ) ;
#14846 = EDGE_LOOP ( 'NONE', ( #23400, #3575, #22288, #32180 ) ) ;
#14845 = CARTESIAN_POINT ( 'NONE',  ( 2.600000000000000089, 0.000000000000000000, 1.500000000000000444 ) ) ;
#14847 = CARTESIAN_POINT ( 'NONE',  ( -2.437550801365593767, 3.675193018007247403, -1.088641768524161391 ) ) ;
#14848 = CYLINDRICAL_SURFACE ( 'NONE', #22448, 0.5000000000000000000 ) ;
#14849 = CARTESIAN_POINT ( 'NONE',  ( 7.249760686538667009, -7.135485519862032611, 5.064320921489797733 ) ) ;
#14851 = EDGE_CURVE ( 'NONE', #19087, #596, #20965, .T. ) ;
#14850 = CARTESIAN_POINT ( 'NONE',  ( 23.71121667297774138, -6.322215142808039090, -3.993434336039487498 ) ) ;
#14852 = VERTEX_POINT ( 'NONE', #15428 ) ;
#14854 = ORIENTED_EDGE ( 'NONE', *, *, #16588, .F. ) ;
#14853 = CARTESIAN_POINT ( 'NONE',  ( 24.14342515508168674, -17.38895391569510807, 1.425886477552664289 ) ) ;
#14855 = EDGE_CURVE ( 'NONE', #30676, #24271, #31184, .T. ) ;
#14856 = CARTESIAN_POINT ( 'NONE',  ( 17.32050807568873552, 10.00000000000002309, 1.508259000770582059 ) ) ;
#14857 = CARTESIAN_POINT ( 'NONE',  ( 0.000000000000000000, -4.762163868918342757, 9.915734732513202587 ) ) ;
#14858 = CARTESIAN_POINT ( 'NONE',  ( 10.00000000000000000, 4.971152295393300946, 0.6226916219172224931 ) ) ;
#14859 = EDGE_CURVE ( 'NONE', #4708, #14801, #5942, .T. ) ;
#14860 = CARTESIAN_POINT ( 'NONE',  ( -21.68109753780534632, 18.70748839123718454, 1.500000000000000000 ) ) ;
#14861 = DIRECTION ( 'NONE',  ( 0.000000000000000000, 0.000000000000000000, 1.000000000000000000 ) ) ;
#14862 = CARTESIAN_POINT ( 'NONE',  ( -3.308580754637445498, -10.64006648303969271, -1.743554639575954690 ) ) ;
#14863 = CARTESIAN_POINT ( 'NONE',  ( 109.4744264295851082, 15.07339897850245158, 2.806473568333413660 ) ) ;
#14864 =( BOUNDED_SURFACE ( )  B_SPLINE_SURFACE ( 3, 2, ( 
 ( #31974, #29140, #23938 ),
 ( #21766, #18771, #3423 ),
 ( #9223, #24101, #24428 ),
 ( #9042, #6227, #21615 ),
 ( #4065, #14231, #28976 ),
 ( #19451, #29644, #6562 ),
 ( #13584, #16080, #26619 ),
 ( #3723, #16761, #23790 ),
 ( #902, #19101, #11080 ),
 ( #3576, #21279, #26962 ),
 ( #16571, #1227, #26783 ),
 ( #11420, #31478, #31819 ),
 ( #8891, #6076, #29289 ),
 ( #6375, #26477, #3900 ),
 ( #14576, #1717, #2394 ),
 ( #11915, #2206, #22611 ),
 ( #17063, #14379, #14738 ),
 ( #19755, #25090, #4563 ),
 ( #22771, #27461, #12392 ),
 ( #4393, #32822, #24590 ),
 ( #27275, #29961, #24780 ),
 ( #32978, #10046, #24935 ),
 ( #6725, #9542, #25277 ),
 ( #32331, #12566, #12075 ) ),
 .UNSPECIFIED., .F., .F., .F. ) 
 B_SPLINE_SURFACE_WITH_KNOTS ( ( 4, 2, 2, 2, 2, 2, 2, 2, 2, 2, 2, 4 ),
 ( 3, 3 ),
 ( 0.009504881860343756053, 0.01278571900407518211, 0.01606655614780660990, 0.01934739329153803422, 0.02098781186340374638, 0.02262823043526946201, 0.02590906757900088980, 0.02918990472273231412, 0.03083032329459802975, 0.03247074186646374538, 0.03411116043832945754, 0.03575157901019516971 ),
 ( 0.000000000000000000, 1.000000000000000000 ),
 .UNSPECIFIED. ) 
 GEOMETRIC_REPRESENTATION_ITEM ( )  RATIONAL_B_SPLINE_SURFACE ( (
 ( 1.000000000000000000, 0.7071067811865475727, 1.000000000000000000),
 ( 1.000000000000000000, 0.7071067811865475727, 1.000000000000000000),
 ( 1.000000000000000000, 0.7071067811865475727, 1.000000000000000000),
 ( 1.000000000000000000, 0.7071067811865475727, 1.000000000000000000),
 ( 1.000000000000000000, 0.7071067811865471286, 1.000000000000000000),
 ( 1.000000000000000000, 0.7071067811865471286, 1.000000000000000000),
 ( 1.000000000000000000, 0.7071067811865475727, 1.000000000000000000),
 ( 1.000000000000000000, 0.7071067811865475727, 1.000000000000000000),
 ( 1.000000000000000000, 0.7071067811865486830, 1.000000000000000000),
 ( 1.000000000000000000, 0.7071067811865486830, 1.000000000000000000),
 ( 1.000000000000000000, 0.7071067811865475727, 1.000000000000000000),
 ( 1.000000000000000000, 0.7071067811865475727, 1.000000000000000000),
 ( 1.000000000000000000, 0.7071067811865475727, 1.000000000000000000),
 ( 1.000000000000000000, 0.7071067811865475727, 1.000000000000000000),
 ( 1.000000000000000000, 0.7071067811865475727, 1.000000000000000000),
 ( 1.000000000000000000, 0.7071067811865475727, 1.000000000000000000),
 ( 1.000000000000000000, 0.7071067811865475727, 1.000000000000000000),
 ( 1.000000000000000000, 0.7071067811865475727, 1.000000000000000000),
 ( 1.000000000000000000, 0.7071067811865475727, 1.000000000000000000),
 ( 1.000000000000000000, 0.7071067811865475727, 1.000000000000000000),
 ( 1.000000000000000000, 0.7071067811865475727, 1.000000000000000000),
 ( 1.000000000000000000, 0.7071067811865475727, 1.000000000000000000),
 ( 1.000000000000000000, 0.7071067811865475727, 1.000000000000000000),
 ( 1.000000000000000000, 0.7071067811865475727, 1.000000000000000000) ) ) 
 REPRESENTATION_ITEM ( '' )  SURFACE ( )  );
#14865 = DIRECTION ( 'NONE',  ( 0.000000000000000000, 0.000000000000000000, 1.000000000000000000 ) ) ;
#14866 = DIRECTION ( 'NONE',  ( 0.000000000000000000, 0.000000000000000000, 1.000000000000000000 ) ) ;
#14867 = ORIENTED_EDGE ( 'NONE', *, *, #16934, .F. ) ;
#14868 = DIRECTION ( 'NONE',  ( 0.9896144216807900573, 0.000000000000000000, 0.1437473352845035912 ) ) ;
#14869 = ORIENTED_EDGE ( 'NONE', *, *, #15469, .T. ) ;
#14870 = EDGE_CURVE ( 'NONE', #31289, #28214, #6565, .T. ) ;
#14871 = B_SPLINE_CURVE_WITH_KNOTS ( 'NONE', 3,
 ( #6677, #29909, #11677, #16867, #27063, #4166, #27568, #29406, #14332, #4667 ),
 .UNSPECIFIED., .F., .F.,
 ( 4, 2, 2, 2, 4 ),
 ( 2.493548413898819905E-07, 0.0005478513795029398394, 0.001095453404164489775, 0.001643055428826039601, 0.002190657453487589428 ),
 .UNSPECIFIED. ) ;
#14872 = CARTESIAN_POINT ( 'NONE',  ( 21.37217251140774721, -21.79767279465052709, 1.352145825573594307 ) ) ;
#14873 = DIRECTION ( 'NONE',  ( -0.9207005872994481477, 0.3902696869428256554, -4.157791683307529050E-18 ) ) ;
#14874 = DIRECTION ( 'NONE',  ( 0.000000000000000000, 0.000000000000000000, -1.000000000000000000 ) ) ;
#14875 = ORIENTED_EDGE ( 'NONE', *, *, #31420, .T. ) ;
#14876 = CARTESIAN_POINT ( 'NONE',  ( 108.0381478102898853, 18.39058198498274876, -4.599267682029278603 ) ) ;
#14877 = ORIENTED_EDGE ( 'NONE', *, *, #18466, .T. ) ;
#14878 = CARTESIAN_POINT ( 'NONE',  ( 0.000000000000000000, 0.000000000000000000, 0.000000000000000000 ) ) ;
#14880 = VERTEX_POINT ( 'NONE', #11239 ) ;
#14879 = CARTESIAN_POINT ( 'NONE',  ( 102.3451239296545623, -2.871394787408288796, -4.018750258909830286 ) ) ;
#14881 = ORIENTED_EDGE ( 'NONE', *, *, #8916, .T. ) ;
#14882 = CARTESIAN_POINT ( 'NONE',  ( 23.48500000000000298, -2.486304738420683780, 0.2613211581691335383 ) ) ;
#14883 = CARTESIAN_POINT ( 'NONE',  ( 18.58227844715246135, -7.846511338401735536, -2.713652344655542059 ) ) ;
#14885 = ORIENTED_EDGE ( 'NONE', *, *, #29391, .F. ) ;
#14884 = CYLINDRICAL_SURFACE ( 'NONE', #12822, 5.010000000000000675 ) ;
#14886 = CARTESIAN_POINT ( 'NONE',  ( -17.45597128428592981, -27.93932300454937590, 11.00000000000000000 ) ) ;
#14887 = FACE_OUTER_BOUND ( 'NONE', #23662, .T. ) ;
#14888 = CARTESIAN_POINT ( 'NONE',  ( -4.458006279114910875, -5.037799543062196683, 1.500000000000000000 ) ) ;
#14889 = EDGE_CURVE ( 'NONE', #17028, #3611, #27298, .T. ) ;
#14890 = CARTESIAN_POINT ( 'NONE',  ( 107.3477315916820913, -15.88627780335592732, 1.500000000000000000 ) ) ;
#14892 = ORIENTED_EDGE ( 'NONE', *, *, #33071, .T. ) ;
#14891 = CARTESIAN_POINT ( 'NONE',  ( 108.0616218773274824, -18.95670182053928698, -4.502367357316522600 ) ) ;
#14893 = ADVANCED_FACE ( 'NONE', ( #11570 ), #13738, .T. ) ;
#14894 = LINE ( 'NONE', #4724, #759 ) ;
#14895 = CARTESIAN_POINT ( 'NONE',  ( 10.57125986779756843, -4.971152295393299170, -0.6226916219172566880 ) ) ;
#14896 = CARTESIAN_POINT ( 'NONE',  ( 22.98500000136559507, -2.892927487894331406, 1.570731468192932301 ) ) ;
#14897 = CARTESIAN_POINT ( 'NONE',  ( 108.2036592059122171, 19.31221474348546607, -3.351118779959896266 ) ) ;
#14898 = CARTESIAN_POINT ( 'NONE',  ( 0.000000000000000000, -1.999317321091575561, 10.76487093102064030 ) ) ;
#14899 = CARTESIAN_POINT ( 'NONE',  ( 20.00016891673655195, -21.67414139014265473, -1.443203664631054428 ) ) ;
#14900 = ORIENTED_EDGE ( 'NONE', *, *, #1015, .T. ) ;
#14901 = DIRECTION ( 'NONE',  ( -0.000000000000000000, -0.000000000000000000, -1.000000000000000000 ) ) ;
#14902 = FACE_OUTER_BOUND ( 'NONE', #3414, .T. ) ;
#14903 = CARTESIAN_POINT ( 'NONE',  ( -6.587550801365593678, 0.3701630799359330593, -3.521866450007987037 ) ) ;
#14904 = ORIENTED_EDGE ( 'NONE', *, *, #29524, .F. ) ;
#14905 = ADVANCED_FACE ( 'NONE', ( #18773 ), #16414, .T. ) ;
#14906 = CIRCLE ( 'NONE', #31492, 0.5000000000000000000 ) ;
#14907 = DIRECTION ( 'NONE',  ( 0.000000000000000000, -0.08715574274766134388, -0.9961946980917452121 ) ) ;
#14908 = FACE_OUTER_BOUND ( 'NONE', #13915, .T. ) ;
#14909 = CYLINDRICAL_SURFACE ( 'NONE', #19420, 5.010000000000000675 ) ;
#14910 = EDGE_LOOP ( 'NONE', ( #23091, #24422, #1924, #12825 ) ) ;
#14911 = DIRECTION ( 'NONE',  ( -0.000000000000000000, -0.000000000000000000, -1.000000000000000000 ) ) ;
#14912 = ORIENTED_EDGE ( 'NONE', *, *, #15920, .T. ) ;
#14913 = CARTESIAN_POINT ( 'NONE',  ( 0.5704036742843068275, -3.563415854978262409, -8.851103337321053033 ) ) ;
#14914 = ORIENTED_EDGE ( 'NONE', *, *, #20004, .T. ) ;
#14915 = LINE ( 'NONE', #1749, #7602 ) ;
#14917 = ORIENTED_EDGE ( 'NONE', *, *, #16796, .F. ) ;
#14916 = CARTESIAN_POINT ( 'NONE',  ( 0.000000000000000000, 0.000000000000000000, 0.000000000000000000 ) ) ;
#14918 = VERTEX_POINT ( 'NONE', #3903 ) ;
#14919 = CARTESIAN_POINT ( 'NONE',  ( 34.48223484310469900, 0.5000000000000000000, 2.482234843104950350 ) ) ;
#14920 = EDGE_CURVE ( 'NONE', #15578, #10646, #2305, .T. ) ;
#14922 = VERTEX_POINT ( 'NONE', #24103 ) ;
#14921 = AXIS2_PLACEMENT_3D ( 'NONE', #10519, #18048, #28237 ) ;
#14923 = PLANE ( 'NONE',  #27302 ) ;
#14925 = EDGE_LOOP ( 'NONE', ( #8588, #30540, #3794, #19749 ) ) ;
#14924 = CARTESIAN_POINT ( 'NONE',  ( 3.529609406779910419, -12.17998485103522199, -1.500000000000000000 ) ) ;
#14926 = AXIS2_PLACEMENT_3D ( 'NONE', #26014, #3121, #13762 ) ;
#14927 = DIRECTION ( 'NONE',  ( 0.000000000000000000, 0.000000000000000000, -1.000000000000000000 ) ) ;
#14928 = CARTESIAN_POINT ( 'NONE',  ( 26.34939556550225248, 19.05368625490715928, 2.334455007174210728 ) ) ;
#14929 = CARTESIAN_POINT ( 'NONE',  ( 107.5603894785017047, -18.96336710931705838, 4.563597971275775933 ) ) ;
#14930 = AXIS2_PLACEMENT_3D ( 'NONE', #30701, #2086, #30010 ) ;
#14931 =( BOUNDED_CURVE ( )  B_SPLINE_CURVE ( 2, ( #22043, #19377, #24875, #4151, #27048, #24517, #32264, #4649, #1335, #11509, #29575 ),
 .UNSPECIFIED., .F., .F. ) 
 B_SPLINE_CURVE_WITH_KNOTS ( ( 3, 2, 2, 2, 2, 3 ),
 ( 0.7478822619934377691, 0.7500000000000000000, 0.7656250000000000000, 0.7812500000000000000, 0.7968750000000000000, 0.8103822619934377691 ),
 .UNSPECIFIED. ) 
 CURVE ( )  GEOMETRIC_REPRESENTATION_ITEM ( )  RATIONAL_B_SPLINE_CURVE ( ( 0.9821626249036861100, 0.9896829947469995004, 1.000000000000000000, 0.9238795325112867385, 1.000000000000000000, 0.9238795325112867385, 1.000000000000000000, 0.9238795325112867385, 1.000000000000000000, 0.9341965377642872381, 0.9821626249036861100 ) ) 
 REPRESENTATION_ITEM ( '' )  );
#14932 = DIRECTION ( 'NONE',  ( -0.000000000000000000, 0.000000000000000000, 1.000000000000000000 ) ) ;
#14933 = CARTESIAN_POINT ( 'NONE',  ( 107.8460215217088631, -15.85211033425179039, -1.499787059522396326 ) ) ;
#14934 = CARTESIAN_POINT ( 'NONE',  ( 0.08034255810681184551, 7.899847910286125874, -7.347818361010319599 ) ) ;
#14935 = B_SPLINE_CURVE_WITH_KNOTS ( 'NONE', 3,
 ( #14165, #24363, #1480, #9135, #6967, #29730, #30386, #25017, #25191, #9318 ),
 .UNSPECIFIED., .F., .F.,
 ( 4, 2, 2, 2, 4 ),
 ( 3.032460776734494026E-07, 0.0005479053915603979358, 0.001095507537043122551, 0.001643109682525847057, 0.002190711828008571564 ),
 .UNSPECIFIED. ) ;
#14936 = DIRECTION ( 'NONE',  ( -0.08910563629484158366, -0.9960221812693186294, 0.000000000000000000 ) ) ;
#14937 = CARTESIAN_POINT ( 'NONE',  ( -1.170068671574867158, -6.059534462705557623, 4.522129901861156931 ) ) ;
#14938 = LINE ( 'NONE', #7782, #2824 ) ;
#14939 = CARTESIAN_POINT ( 'NONE',  ( 47.68482864957696421, -3.825617316378856714, -0.07017451552781628354 ) ) ;
#14940 = VECTOR ( 'NONE', #32431, 1000.000000000000114 ) ;
#14941 = DIRECTION ( 'NONE',  ( -0.000000000000000000, -0.000000000000000000, -1.000000000000000000 ) ) ;
#14942 = CARTESIAN_POINT ( 'NONE',  ( -4.200050802731187360, 0.9222479816126443186, 3.113457007523260156 ) ) ;
#14943 = ORIENTED_EDGE ( 'NONE', *, *, #24860, .F. ) ;
#14944 = CARTESIAN_POINT ( 'NONE',  ( -3.500050800000000351, 2.983565686104819648, 0.3135853898029609677 ) ) ;
#14945 = CIRCLE ( 'NONE', #7481, 10.99999999999999822 ) ;
#14946 = CARTESIAN_POINT ( 'NONE',  ( 3.936147556303794648, 18.00000000000000355, -4.854816414140051606 ) ) ;
#14947 = DIRECTION ( 'NONE',  ( -1.000000000000000000, 8.574039729943019576E-17, 0.000000000000000000 ) ) ;
#14948 = EDGE_LOOP ( 'NONE', ( #13104, #31434, #26115, #14840 ) ) ;
#14949 = CARTESIAN_POINT ( 'NONE',  ( -50.60000000000000142, -10.96966150227468972, -1.500000000000000000 ) ) ;
#14950 = CARTESIAN_POINT ( 'NONE',  ( 107.5411459829244052, -18.68417316270920026, 4.956489308412717065 ) ) ;
#14951 = VECTOR ( 'NONE', #19363, 1000.000000000000000 ) ;
#14952 = ORIENTED_EDGE ( 'NONE', *, *, #2273, .F. ) ;
#14953 = CARTESIAN_POINT ( 'NONE',  ( 6.555498503425793544, -13.70794208679299153, 1.755773382248213110 ) ) ;
#14954 = PERSON_AND_ORGANIZATION ( #20338, #26934 ) ;
#14955 = CARTESIAN_POINT ( 'NONE',  ( 3.500000000000000000, 0.000000000000000000, 0.000000000000000000 ) ) ;
#14956 = VERTEX_POINT ( 'NONE', #1230 ) ;
#14957 = CARTESIAN_POINT ( 'NONE',  ( 15.88616825581402203, -21.20699617082199850, 1.500000000000000000 ) ) ;
#14958 = ADVANCED_FACE ( 'NONE', ( #26786 ), #21618, .T. ) ;
#14959 = EDGE_CURVE ( 'NONE', #32661, #536, #89, .T. ) ;
#14960 = ORIENTED_EDGE ( 'NONE', *, *, #11578, .T. ) ;
#14961 = DIRECTION ( 'NONE',  ( 1.000000000000000000, -8.574039729943018344E-17, -0.000000000000000000 ) ) ;
#14962 = CARTESIAN_POINT ( 'NONE',  ( 85.01592635901995720, -4.880223576643683892, -4.275175582424107112 ) ) ;
#14963 = CARTESIAN_POINT ( 'NONE',  ( 6.530491482054475050, -2.114164693852647048, 8.398420403995366712 ) ) ;
#14964 = DIRECTION ( 'NONE',  ( 8.326672684688674053E-17, 0.3746065934159164001, -0.9271838545667857590 ) ) ;
#14965 = ADVANCED_FACE ( 'NONE', ( #1548 ), #29467, .F. ) ;
#14966 = AXIS2_PLACEMENT_3D ( 'NONE', #9118, #26541, #6636 ) ;
#14967 = DIRECTION ( 'NONE',  ( -0.000000000000000000, -0.9659258262890662028, -0.2588190451025286776 ) ) ;
#14968 = CARTESIAN_POINT ( 'NONE',  ( 7.249760686538667009, 6.940565734314597002, 4.007137495034836405 ) ) ;
#14969 = CIRCLE ( 'NONE', #1654, 8.500000000000000000 ) ;
#14970 = ORIENTED_EDGE ( 'NONE', *, *, #17900, .T. ) ;
#14971 = AXIS2_PLACEMENT_3D ( 'NONE', #14421, #24630, #11957 ) ;
#14972 = DIRECTION ( 'NONE',  ( 0.1027947991993878873, -0.9947025833170223263, 3.550762114890027021E-15 ) ) ;
#14973 = LINE ( 'NONE', #2310, #22481 ) ;
#14974 = DIRECTION ( 'NONE',  ( 0.000000000000000000, 0.000000000000000000, -1.000000000000000000 ) ) ;
#14975 = DIRECTION ( 'NONE',  ( -0.000000000000000000, -0.3746065934159164001, 0.9271838545667856479 ) ) ;
#14976 = CARTESIAN_POINT ( 'NONE',  ( -8.000050799999991469, 1.058074100335029355, 3.097767084515848701 ) ) ;
#14977 = DIRECTION ( 'NONE',  ( 7.770718973608992215E-17, 0.9063077870366522681, -0.4226182617406944453 ) ) ;
#14978 = CARTESIAN_POINT ( 'NONE',  ( -56.32770133515839461, 0.5000000000000000000, -1.500000000000000000 ) ) ;
#14979 = CARTESIAN_POINT ( 'NONE',  ( 23.24965665534722348, -21.93932291342295215, 1.034606501594972583 ) ) ;
#14980 = VERTEX_POINT ( 'NONE', #26479 ) ;
#14981 = CARTESIAN_POINT ( 'NONE',  ( -5.162550801365593856, -2.752080473201636845, 2.228590825266444586 ) ) ;
#14982 = ORIENTED_EDGE ( 'NONE', *, *, #12803, .T. ) ;
#14983 = CARTESIAN_POINT ( 'NONE',  ( -6.704531657079157547, 2.975847129947406522, 0.3127741368606808403 ) ) ;
#14984 = CARTESIAN_POINT ( 'NONE',  ( 25.73500000136559507, 3.156283516753366047, 0.9349337715887203748 ) ) ;
#14985 = AXIS2_PLACEMENT_3D ( 'NONE', #9434, #29846, #32527 ) ;
#14986 = PLANE ( 'NONE',  #16729 ) ;
#14987 = AXIS2_PLACEMENT_3D ( 'NONE', #3372, #26437, #28753 ) ;
#14988 = CARTESIAN_POINT ( 'NONE',  ( 3.519433398973329297, -1.626303258728258623E-15, -1.098451328137469929 ) ) ;
#14989 = CARTESIAN_POINT ( 'NONE',  ( 108.3631457176462618, 20.50192626814461860, 1.454023645857057678 ) ) ;
#14990 = ORIENTED_EDGE ( 'NONE', *, *, #11259, .T. ) ;
#14991 = CARTESIAN_POINT ( 'NONE',  ( -1.668773398854276148E-16, -1.946309384392560737, -4.616489984850551842 ) ) ;
#14992 = CIRCLE ( 'NONE', #28894, 8.750000000000000000 ) ;
#14993 = AXIS2_PLACEMENT_3D ( 'NONE', #5472, #25873, #7815 ) ;
#14994 = AXIS2_PLACEMENT_3D ( 'NONE', #12179, #27225, #1855 ) ;
#14995 = EDGE_LOOP ( 'NONE', ( #14110, #32382, #7190, #27134 ) ) ;
#14996 = CARTESIAN_POINT ( 'NONE',  ( 6.356381935169120645, 2.055898738447997864, 8.357622142800094522 ) ) ;
#14997 = PERSON_AND_ORGANIZATION ( #6766, #25292 ) ;
#14998 = ADVANCED_FACE ( 'NONE', ( #14080 ), #31661, .F. ) ;
#14999 = CARTESIAN_POINT ( 'NONE',  ( 18.75885765836901342, -5.872710146263817599, 4.003574682309002597 ) ) ;
#15000 = EDGE_CURVE ( 'NONE', #24269, #28814, #28381, .T. ) ;
#15001 = EDGE_CURVE ( 'NONE', #22521, #15923, #13937, .T. ) ;
#15002 = AXIS2_PLACEMENT_3D ( 'NONE', #20142, #9927, #30337 ) ;
#15003 = CARTESIAN_POINT ( 'NONE',  ( 5.377543748152550762, 6.139290821770327256, -5.151476664237414127 ) ) ;
#15005 = CARTESIAN_POINT ( 'NONE',  ( 4.075891499408641642E-16, 4.753758587302147731, 0.000000000000000000 ) ) ;
#15004 = LINE ( 'NONE', #7838, #14563 ) ;
#15006 = ORIENTED_EDGE ( 'NONE', *, *, #24264, .T. ) ;
#15007 = CARTESIAN_POINT ( 'NONE',  ( 108.0291781248180598, -18.48951985539477505, -4.325670280508457921 ) ) ;
#15008 = DIRECTION ( 'NONE',  ( 1.000000000000000000, -8.574039729943018344E-17, -0.000000000000000000 ) ) ;
#15009 = CARTESIAN_POINT ( 'NONE',  ( 22.73500000136559862, 3.156283516753366047, 0.9349337715887203748 ) ) ;
#15010 = CARTESIAN_POINT ( 'NONE',  ( 15.92126372259303224, -16.39212668776233883, -1.753532113938507608 ) ) ;
#15012 = ORIENTED_EDGE ( 'NONE', *, *, #7124, .F. ) ;
#15011 = CARTESIAN_POINT ( 'NONE',  ( 5.377543748152548986, 7.892520144992453801, -1.391664247347147443 ) ) ;
#15013 = CARTESIAN_POINT ( 'NONE',  ( -3.287550801365593856, 2.752080473201636845, -2.228590825266444142 ) ) ;
#15014 = DIRECTION ( 'NONE',  ( 0.000000000000000000, 0.000000000000000000, -1.000000000000000000 ) ) ;
#15015 = AXIS2_PLACEMENT_3D ( 'NONE', #23913, #13861, #715 ) ;
#15016 = CARTESIAN_POINT ( 'NONE',  ( -55.59999999999999432, -10.96966150227468972, 6.999999999999999112 ) ) ;
#15017 = CARTESIAN_POINT ( 'NONE',  ( 0.000000000000000000, 0.000000000000000000, -6.000000000000000888 ) ) ;
#15018 = ORIENTED_EDGE ( 'NONE', *, *, #15727, .T. ) ;
#15020 = VERTEX_POINT ( 'NONE', #904 ) ;
#15019 = CARTESIAN_POINT ( 'NONE',  ( 21.59695500784411593, -17.14749606024852469, 1.524646196218438110 ) ) ;
#15021 = AXIS2_PLACEMENT_3D ( 'NONE', #9474, #22528, #30076 ) ;
#15022 = AXIS2_PLACEMENT_3D ( 'NONE', #7600, #4448, #25485 ) ;
#15024 = VECTOR ( 'NONE', #10263, 1000.000000000000000 ) ;
#15023 = DIRECTION ( 'NONE',  ( 0.000000000000000000, 0.000000000000000000, -1.000000000000000000 ) ) ;
#15025 = CARTESIAN_POINT ( 'NONE',  ( 2.592584712405588299, -10.08167743096628222, -2.232024585011588069 ) ) ;
#15026 = CIRCLE ( 'NONE', #10216, 4.000000000000001776 ) ;
#15027 = CARTESIAN_POINT ( 'NONE',  ( 23.48500000136559862, 0.9349337715887185984, -3.156283516753368268 ) ) ;
#15028 = VECTOR ( 'NONE', #13723, 1000.000000000000000 ) ;
#15029 = CARTESIAN_POINT ( 'NONE',  ( 54.94526044242307705, -5.359369332727369262, 3.993434333344287435 ) ) ;
#15030 = CARTESIAN_POINT ( 'NONE',  ( -0.4073435738283839314, -14.65433346320568653, -1.499999999999723110 ) ) ;
#15031 = CARTESIAN_POINT ( 'NONE',  ( 3.249999999999999556, -1.239665997526818053, -9.314797388894906049 ) ) ;
#15032 = EDGE_CURVE ( 'NONE', #15923, #19457, #21429, .T. ) ;
#15033 = CARTESIAN_POINT ( 'NONE',  ( 3.063284526839887167, 0.000000000000000000, 0.000000000000000000 ) ) ;
#15034 = CARTESIAN_POINT ( 'NONE',  ( 48.08400536259535585, -8.675012021211058411, 2.713652344655544724 ) ) ;
#15035 = ORIENTED_EDGE ( 'NONE', *, *, #16922, .F. ) ;
#15036 = CARTESIAN_POINT ( 'NONE',  ( 68.59913483175155591, -3.860138077755596697, 2.184958020780332522 ) ) ;
#15037 = EDGE_CURVE ( 'NONE', #19939, #22762, #7568, .T. ) ;
#15038 = CIRCLE ( 'NONE', #10340, 6.000000000000001776 ) ;
#15040 = CIRCLE ( 'NONE', #8653, 2.999999999999999556 ) ;
#15039 = APPROVAL_DATE_TIME ( #25577, #29060 ) ;
#15041 = DIRECTION ( 'NONE',  ( -1.000000000000000000, 2.498001805406600196E-13, 0.000000000000000000 ) ) ;
#15042 = ORIENTED_EDGE ( 'NONE', *, *, #20840, .T. ) ;
#15043 = AXIS2_PLACEMENT_3D ( 'NONE', #26842, #19146, #3960 ) ;
#15044 = CARTESIAN_POINT ( 'NONE',  ( 108.0553047662118331, 18.48611868536735514, -4.631814065063916352 ) ) ;
#15045 = CIRCLE ( 'NONE', #24640, 0.5000000000000004441 ) ;
#15046 = ORIENTED_EDGE ( 'NONE', *, *, #27813, .F. ) ;
#15047 = CARTESIAN_POINT ( 'NONE',  ( -17.06946722187133147, 9.668269422107719890, 1.993141146079933312 ) ) ;
#15049 = ORIENTED_EDGE ( 'NONE', *, *, #2150, .T. ) ;
#15048 = CARTESIAN_POINT ( 'NONE',  ( 40.87792176339704042, -5.783270549457658838, -4.043900193582110170 ) ) ;
#15050 = EDGE_CURVE ( 'NONE', #19429, #7258, #9178, .T. ) ;
#15051 = VERTEX_POINT ( 'NONE', #1719 ) ;
#15052 = AXIS2_PLACEMENT_3D ( 'NONE', #29413, #21577, #14028 ) ;
#15053 = DIRECTION ( 'NONE',  ( -0.000000000000000000, -0.000000000000000000, -1.000000000000000000 ) ) ;
#15054 = CARTESIAN_POINT ( 'NONE',  ( -7.980601973981865882, 2.418815195390975781, -2.640139169206693115 ) ) ;
#15055 = LINE ( 'NONE', #29682, #10806 ) ;
#15056 = VECTOR ( 'NONE', #18482, 1000.000000000000227 ) ;
#15057 = CARTESIAN_POINT ( 'NONE',  ( 85.45070076415389337, -7.158483446636732417, -2.713652344655542059 ) ) ;
#15059 = EDGE_LOOP ( 'NONE', ( #15260, #32774, #31973 ) ) ;
#15058 = CARTESIAN_POINT ( 'NONE',  ( 0.7632845268430009655, 4.729683950891516275, 7.360373001717795738 ) ) ;
#15060 = CARTESIAN_POINT ( 'NONE',  ( 21.08401840680159367, -16.78474387324287775, 1.500000000000000000 ) ) ;
#15061 = LINE ( 'NONE', #32979, #29389 ) ;
#15062 = ADVANCED_FACE ( 'NONE', ( #17568 ), #22120, .T. ) ;
#15063 = CARTESIAN_POINT ( 'NONE',  ( 10.56870887191539587, 1.476463073999701781, -4.787500056513350977 ) ) ;
#15064 = CARTESIAN_POINT ( 'NONE',  ( 7.461135469111495944, -4.560857689424945960, -1.500000000000000000 ) ) ;
#15066 = ORIENTED_EDGE ( 'NONE', *, *, #25949, .F. ) ;
#15065 = DIRECTION ( 'NONE',  ( -1.000000000000000000, 0.000000000000000000, 0.000000000000000000 ) ) ;
#15067 = CARTESIAN_POINT ( 'NONE',  ( 0.000000000000000000, -7.593217523260520352, -7.958834565716849774 ) ) ;
#15068 = AXIS2_PLACEMENT_3D ( 'NONE', #29884, #30236, #6808 ) ;
#15069 = AXIS2_PLACEMENT_3D ( 'NONE', #29936, #7023, #14865 ) ;
#15070 = LINE ( 'NONE', #30469, #21427 ) ;
#15071 = CARTESIAN_POINT ( 'NONE',  ( 23.36000000136559507, 0.9349337715887185984, -3.156283516753368268 ) ) ;
#15072 = AXIS2_PLACEMENT_3D ( 'NONE', #14167, #19690, #24365 ) ;
#15073 = VECTOR ( 'NONE', #31155, 1000.000000000000000 ) ;
#15074 = CARTESIAN_POINT ( 'NONE',  ( -8.000050800000000351, -1.836970198721030181E-16, -3.000000000000000444 ) ) ;
#15075 = AXIS2_PLACEMENT_3D ( 'NONE', #13746, #31988, #9057 ) ;
#15076 = CARTESIAN_POINT ( 'NONE',  ( 18.74147553047095727, -6.067007450452971185, -3.690577026541935091 ) ) ;
#15077 = DIRECTION ( 'NONE',  ( -0.000000000000000000, -0.000000000000000000, -1.000000000000000000 ) ) ;
#15078 = ORIENTED_EDGE ( 'NONE', *, *, #15037, .T. ) ;
#15079 = CARTESIAN_POINT ( 'NONE',  ( 5.612974384376779646, -4.279837954023520297, 7.013635602076194075 ) ) ;
#15080 = ADVANCED_FACE ( 'NONE', ( #9392 ), #32333, .F. ) ;
#15081 = VECTOR ( 'NONE', #32734, 1000.000000000000000 ) ;
#15082 = AXIS2_PLACEMENT_3D ( 'NONE', #16361, #498, #26569 ) ;
#15083 = DIRECTION ( 'NONE',  ( 1.040834085586084257E-14, 0.000000000000000000, -1.000000000000000000 ) ) ;
#15084 = CARTESIAN_POINT ( 'NONE',  ( -6.037550801365593856, -3.675193018007245627, 1.088641768524163389 ) ) ;
#15085 = VERTEX_POINT ( 'NONE', #7231 ) ;
#15086 = AXIS2_PLACEMENT_3D ( 'NONE', #30915, #2845, #20559 ) ;
#15087 = FACE_OUTER_BOUND ( 'NONE', #30573, .T. ) ;
#15088 = FACE_OUTER_BOUND ( 'NONE', #12189, .T. ) ;
#15089 = ADVANCED_FACE ( 'NONE', ( #27767 ), #4565, .T. ) ;
#15090 = CARTESIAN_POINT ( 'NONE',  ( 6.013832568680315127, -13.53405802968792848, -1.500000000000000444 ) ) ;
#15091 = EDGE_LOOP ( 'NONE', ( #29817, #24492, #30335 ) ) ;
#15092 = CARTESIAN_POINT ( 'NONE',  ( 3.249999999999999556, -9.241976615262146311, 2.300561732649529567 ) ) ;
#15093 = EDGE_CURVE ( 'NONE', #19561, #10302, #12905, .T. ) ;
#15094 = ORIENTED_EDGE ( 'NONE', *, *, #22241, .T. ) ;
#15095 = VECTOR ( 'NONE', #18495, 1000.000000000000000 ) ;
#15096 = DIRECTION ( 'NONE',  ( 0.000000000000000000, 0.9659258262890670910, 0.2588190451025253469 ) ) ;
#15097 = VERTEX_POINT ( 'NONE', #17265 ) ;
#15098 = CARTESIAN_POINT ( 'NONE',  ( -2.767073886773234292, -0.6621507858625358400, 1.748408842879327629 ) ) ;
#15099 = PRODUCT_DEFINITION_SHAPE ( 'NONE', 'NONE',  #33105 ) ;
#15100 = CIRCLE ( 'NONE', #27403, 2.999999999999999112 ) ;
#15102 = EDGE_LOOP ( 'NONE', ( #26135, #27563, #18025, #32518, #31885 ) ) ;
#15101 = CARTESIAN_POINT ( 'NONE',  ( -3.029131898378900623, -0.04852093894418087194, 1.223527895085199768 ) ) ;
#15103 = ORIENTED_EDGE ( 'NONE', *, *, #28362, .T. ) ;
#15104 = DIRECTION ( 'NONE',  ( 0.000000000000000000, 0.000000000000000000, -1.000000000000000000 ) ) ;
#15105 = EDGE_CURVE ( 'NONE', #5620, #26082, #664, .T. ) ;
#15106 = VECTOR ( 'NONE', #17237, 1000.000000000000114 ) ;
#15107 = CIRCLE ( 'NONE', #714, 5.010000000000000675 ) ;
#15108 = ORIENTED_EDGE ( 'NONE', *, *, #4534, .T. ) ;
#15109 = CARTESIAN_POINT ( 'NONE',  ( 25.75999999999999801, -2.208672634433321348E-15, 0.000000000000000000 ) ) ;
#15111 = VERTEX_POINT ( 'NONE', #24938 ) ;
#15110 = CARTESIAN_POINT ( 'NONE',  ( 2.600000000000000089, 0.000000000000000000, 1.500000000000000000 ) ) ;
#15112 = LINE ( 'NONE', #20299, #27205 ) ;
#15113 = AXIS2_PLACEMENT_3D ( 'NONE', #29159, #17047, #14873 ) ;
#15114 = CARTESIAN_POINT ( 'NONE',  ( 29.35001421184127324, -4.582605737176272953, -4.522129901861162260 ) ) ;
#15115 = CARTESIAN_POINT ( 'NONE',  ( 108.1329823800173671, -19.98427530701536270, 1.262026545339602679 ) ) ;
#15116 = EDGE_CURVE ( 'NONE', #4840, #18222, #2049, .T. ) ;
#15117 = CARTESIAN_POINT ( 'NONE',  ( 45.78962651942645579, 26.61627915917710041, -1.491740999229417941 ) ) ;
#15118 = CARTESIAN_POINT ( 'NONE',  ( 0.1255855353732055757, -9.314797388894898944, 5.239665997526856245 ) ) ;
#15119 = CARTESIAN_POINT ( 'NONE',  ( 25.45368006873450994, -17.55541207042479712, 1.083666005367639018 ) ) ;
#15120 = DIRECTION ( 'NONE',  ( -0.000000000000000000, -0.000000000000000000, -1.000000000000000000 ) ) ;
#15121 = CARTESIAN_POINT ( 'NONE',  ( 10.56870887191539587, -1.476463073999670916, 4.787500056513361635 ) ) ;
#15122 = CIRCLE ( 'NONE', #9246, 0.4999999999999997224 ) ;
#15123 = CARTESIAN_POINT ( 'NONE',  ( 0.2562068301981437757, 8.982429233983488359, 5.229384870727559864 ) ) ;
#15124 = CIRCLE ( 'NONE', #27954, 8.750000000000000000 ) ;
#15125 = CARTESIAN_POINT ( 'NONE',  ( 19.01480233880806381, -3.011762293215138886, 0.07017451550800274385 ) ) ;
#15126 = AXIS2_PLACEMENT_3D ( 'NONE', #22940, #10416, #13089 ) ;
#15127 = AXIS2_PLACEMENT_3D ( 'NONE', #32577, #1649, #19697 ) ;
#15128 = LINE ( 'NONE', #1780, #2819 ) ;
#15129 = EDGE_CURVE ( 'NONE', #18014, #23780, #25841, .T. ) ;
#15130 = CARTESIAN_POINT ( 'NONE',  ( -1.750050802731187405, -0.3135853898029607456, 2.983565686104819648 ) ) ;
#15131 = ORIENTED_EDGE ( 'NONE', *, *, #32704, .T. ) ;
#15132 = VECTOR ( 'NONE', #24915, 1000.000000000000000 ) ;
#15133 = AXIS2_PLACEMENT_3D ( 'NONE', #31100, #8189, #28585 ) ;
#15134 = CARTESIAN_POINT ( 'NONE',  ( -4.437550801365594211, -3.675193018007246071, 1.088641768524163167 ) ) ;
#15135 = CARTESIAN_POINT ( 'NONE',  ( 25.75999999999999801, -2.208672634433321348E-15, -3.024999999999999911 ) ) ;
#15136 = EDGE_CURVE ( 'NONE', #13848, #22878, #19860, .T. ) ;
#15137 = CARTESIAN_POINT ( 'NONE',  ( -40.71733131760397129, -12.43974741078717372, 5.871858320049880398 ) ) ;
#15138 = APPROVAL_PERSON_ORGANIZATION ( #8161, #13290, #13650 ) ;
#15139 = ORIENTED_EDGE ( 'NONE', *, *, #12610, .T. ) ;
#15140 = CARTESIAN_POINT ( 'NONE',  ( -29.73484230743789070, -27.93932300454937590, 11.09540449768827308 ) ) ;
#15141 = CARTESIAN_POINT ( 'NONE',  ( 5.489344087273876127, -5.297876218488277722, -6.152099123112504842 ) ) ;
#15142 = EDGE_LOOP ( 'NONE', ( #2387, #22137, #20644, #12791, #20356 ) ) ;
#15143 = DIRECTION ( 'NONE',  ( 8.574039729943018344E-17, 1.000000000000000000, 0.000000000000000000 ) ) ;
#15144 = PERSON_AND_ORGANIZATION_ROLE ( 'classification_officer' ) ;
#15146 = ORIENTED_EDGE ( 'NONE', *, *, #4305, .T. ) ;
#15145 = CARTESIAN_POINT ( 'NONE',  ( 54.77277180716814087, -8.244003004416214253, 0.07017451552781736601 ) ) ;
#15147 = VERTEX_POINT ( 'NONE', #29646 ) ;
#15148 = CARTESIAN_POINT ( 'NONE',  ( -4.027742607708217015, -8.337697986505625991, 1.744154148835437956 ) ) ;
#15149 = ADVANCED_FACE ( 'NONE', ( #1904 ), #15561, .F. ) ;
#15150 = VERTEX_POINT ( 'NONE', #10892 ) ;
#15151 =( BOUNDED_SURFACE ( )  B_SPLINE_SURFACE ( 3, 2, ( 
 ( #14978, #7309, #7654 ),
 ( #17500, #27696, #4800 ),
 ( #7162, #2318, #5302 ),
 ( #12996, #27548, #32751 ),
 ( #30077, #4988, #30748 ),
 ( #17853, #9639, #30567 ),
 ( #9828, #25375, #2484 ),
 ( #10324, #22709, #25694 ),
 ( #7819, #32911, #20044 ),
 ( #25019, #17356, #18012 ),
 ( #2132, #9981, #20191 ),
 ( #30388, #10130, #4645 ),
 ( #14820, #28201, #2815 ),
 ( #12313, #22529, #7460 ),
 ( #30238, #15480, #25529 ),
 ( #17661, #28051, #27870 ) ),
 .UNSPECIFIED., .F., .F., .F. ) 
 B_SPLINE_SURFACE_WITH_KNOTS ( ( 4, 2, 2, 2, 2, 2, 2, 4 ),
 ( 3, 3 ),
 ( 0.0003684723101340264297, 0.0003800852853942607453, 0.0003916982606544950609, 0.0004033112359147293766, 0.0004149242111749636922, 0.0004381501616954323235, 0.0004497631369556666934, 0.0004613761122159010090 ),
 ( 0.000000000000000000, 1.000000000000000000 ),
 .UNSPECIFIED. ) 
 GEOMETRIC_REPRESENTATION_ITEM ( )  RATIONAL_B_SPLINE_SURFACE ( (
 ( 1.000000000000000000, 0.7071067811865529018, 1.000000000000000000),
 ( 1.000000000000000000, 0.7069009979025784318, 1.000000000000000000),
 ( 1.000000000000000000, 0.7132090502674284238, 1.000000000000000000),
 ( 1.000000000000000000, 0.7358066242641170263, 1.000000000000000000),
 ( 1.000000000000000000, 0.7518633517842446823, 1.000000000000000000),
 ( 1.000000000000000000, 0.7874886208250170272, 1.000000000000000000),
 ( 1.000000000000000000, 0.8071925469186636004, 1.000000000000000000),
 ( 1.000000000000000000, 0.8453094253659971802, 1.000000000000000000),
 ( 1.000000000000000000, 0.8640810776869900511, 1.000000000000000000),
 ( 1.000000000000000000, 0.9164353439694726822, 1.000000000000000000),
 ( 1.000000000000000000, 0.9447016862624076916, 1.000000000000000000),
 ( 1.000000000000000000, 0.9748905170909382134, 1.000000000000000000),
 ( 1.000000000000000000, 0.9828855915604548521, 1.000000000000000000),
 ( 1.000000000000000000, 0.9943518368180752631, 1.000000000000000000),
 ( 1.000000000000000000, 0.9980588531602458957, 1.000000000000000000),
 ( 1.000000000000000000, 0.9983060766582193546, 1.000000000000000000) ) ) 
 REPRESENTATION_ITEM ( '' )  SURFACE ( )  );
#15152 = CARTESIAN_POINT ( 'NONE',  ( 107.9812533011594269, -17.79941431690619069, -4.365076636216545403 ) ) ;
#15153 = VECTOR ( 'NONE', #17351, 1000.000000000000000 ) ;
#15155 = ORIENTED_EDGE ( 'NONE', *, *, #13830, .T. ) ;
#15154 = CARTESIAN_POINT ( 'NONE',  ( -2.354101222566610918, 0.8862716126563827679, 3.215327897825512427 ) ) ;
#15156 = VECTOR ( 'NONE', #13316, 1000.000000000000000 ) ;
#15157 = DIRECTION ( 'NONE',  ( 0.000000000000000000, 0.000000000000000000, -1.000000000000000000 ) ) ;
#15158 = CARTESIAN_POINT ( 'NONE',  ( 108.1288400433390393, -19.92462668933127290, 1.384270303710046335 ) ) ;
#15159 = AXIS2_PLACEMENT_3D ( 'NONE', #19971, #30485, #2732 ) ;
#15160 = DIRECTION ( 'NONE',  ( -1.000000000000000000, -0.000000000000000000, -0.000000000000000000 ) ) ;
#15161 = DIRECTION ( 'NONE',  ( 0.000000000000000000, -0.000000000000000000, -1.000000000000000000 ) ) ;
#15162 = ADVANCED_FACE ( 'NONE', ( #14034 ), #16379, .T. ) ;
#15163 = ORIENTED_EDGE ( 'NONE', *, *, #1446, .T. ) ;
#15164 = DIRECTION ( 'NONE',  ( 0.9947025833170223263, 0.1027947991993880261, -0.000000000000000000 ) ) ;
#15165 = CARTESIAN_POINT ( 'NONE',  ( 108.6457025336241031, 16.11621187055573046, 2.334455007174216057 ) ) ;
#15166 = CARTESIAN_POINT ( 'NONE',  ( -38.14293509397970183, 21.49000000000000199, 1.500000000000000000 ) ) ;
#15167 = LINE ( 'NONE', #4641, #8781 ) ;
#15168 = SECURITY_CLASSIFICATION ( '', '', #25898 ) ;
#15169 = LINE ( 'NONE', #32910, #24133 ) ;
#15170 = CARTESIAN_POINT ( 'NONE',  ( 23.85324836636416634, -17.43424264171716231, -1.580747861890610562 ) ) ;
#15171 = CARTESIAN_POINT ( 'NONE',  ( 24.11000000273118715, 1.573300977624590313, -1.942864903642426144 ) ) ;
#15172 = ORIENTED_EDGE ( 'NONE', *, *, #7059, .F. ) ;
#15173 = CARTESIAN_POINT ( 'NONE',  ( -7.262550801365593500, 0.3701630799359330593, -3.521866450007987037 ) ) ;
#15174 = VERTEX_POINT ( 'NONE', #13704 ) ;
#15175 = EDGE_CURVE ( 'NONE', #8736, #21127, #14497, .T. ) ;
#15176 = CARTESIAN_POINT ( 'NONE',  ( -8.004531657079157370, -2.325406398514293205, 1.883076972206379818 ) ) ;
#15177 = AXIS2_PLACEMENT_3D ( 'NONE', #25689, #21180, #31377 ) ;
#15178 = CARTESIAN_POINT ( 'NONE',  ( 23.98500000136559507, -0.9349337715887248157, 3.156283516753367824 ) ) ;
#15179 = EDGE_CURVE ( 'NONE', #15684, #21443, #116, .T. ) ;
#15180 = DIRECTION ( 'NONE',  ( 0.000000000000000000, 0.7071067811865442421, -0.7071067811865509034 ) ) ;
#15181 = LINE ( 'NONE', #12661, #5533 ) ;
#15182 = DIRECTION ( 'NONE',  ( -1.000000000000000000, -0.000000000000000000, -0.000000000000000000 ) ) ;
#15183 = ORIENTED_EDGE ( 'NONE', *, *, #25491, .T. ) ;
#15184 = DIRECTION ( 'NONE',  ( -1.000000000000000000, 4.930380657631322689E-32, -8.654346879536960414E-15 ) ) ;
#15185 = B_SPLINE_CURVE_WITH_KNOTS ( 'NONE', 3,
 ( #5044, #30439, #10191, #32960, #12857, #15538 ),
 .UNSPECIFIED., .F., .F.,
 ( 4, 2, 4 ),
 ( 0.0003283404404905848075, 0.001393105083344284116, 0.002457869726197983370 ),
 .UNSPECIFIED. ) ;
#15186 = CARTESIAN_POINT ( 'NONE',  ( 10.00000000000000000, -4.467071865485462645, -1.625881193364742572 ) ) ;
#15187 = VERTEX_POINT ( 'NONE', #16533 ) ;
#15188 = LINE ( 'NONE', #1381, #10222 ) ;
#15189 = PERSON_AND_ORGANIZATION ( #6766, #25292 ) ;
#15191 = CARTESIAN_POINT ( 'NONE',  ( 28.66461310467470724, -6.745212029000279053, 4.023790193031063112 ) ) ;
#15190 = CC_DESIGN_SECURITY_CLASSIFICATION ( #27464, ( #33102 ) ) ;
#15192 = DIRECTION ( 'NONE',  ( 0.000000000000000000, 1.000000000000000000, 0.000000000000000000 ) ) ;
#15194 = CARTESIAN_POINT ( 'NONE',  ( 4.749760686538667009, -7.892520144992443143, 1.391664247347202288 ) ) ;
#15193 = DIRECTION ( 'NONE',  ( 0.000000000000000000, 0.000000000000000000, 1.000000000000000000 ) ) ;
#15195 = ORIENTED_EDGE ( 'NONE', *, *, #10562, .T. ) ;
#15196 = CARTESIAN_POINT ( 'NONE',  ( -8.000050800000002127, -2.992755258463658308, -0.2534658811743740192 ) ) ;
#15197 = LINE ( 'NONE', #15701, #16042 ) ;
#15198 = CARTESIAN_POINT ( 'NONE',  ( 24.36000000136559507, -1.570731468192933633, -2.892927487894330074 ) ) ;
#15199 = DIRECTION ( 'NONE',  ( 7.023442172597848233E-17, 0.8191520442889907994, 0.5735764363510474917 ) ) ;
#15201 = ORIENTED_EDGE ( 'NONE', *, *, #19764, .T. ) ;
#15200 = CARTESIAN_POINT ( 'NONE',  ( 16.70660563660005593, -16.26387199940855410, 0.9788672205888330202 ) ) ;
#15202 = AXIS2_PLACEMENT_3D ( 'NONE', #12577, #27470, #17274 ) ;
#15203 = CARTESIAN_POINT ( 'NONE',  ( -7.112550801365592257, 3.675193018007247403, -1.088641768524161391 ) ) ;
#15204 = CARTESIAN_POINT ( 'NONE',  ( 2.274274201625313907, -9.915734732513202587, -4.762163868918404930 ) ) ;
#15205 = DIRECTION ( 'NONE',  ( -1.000000000000000000, 8.574039729943022041E-17, 1.232595164407830946E-32 ) ) ;
#15206 = CARTESIAN_POINT ( 'NONE',  ( 47.93076651534932608, -6.701564465775193824, -3.993434086979319453 ) ) ;
#15207 = VERTEX_POINT ( 'NONE', #1013 ) ;
#15209 = EDGE_LOOP ( 'NONE', ( #32999, #2421, #14832, #9372 ) ) ;
#15208 = CARTESIAN_POINT ( 'NONE',  ( 24.07542780980101682, -17.38801686517350475, 1.438486003925011136 ) ) ;
#15210 = CARTESIAN_POINT ( 'NONE',  ( 11.04311965146447427, 15.00000000000002132, -1.491740999229419273 ) ) ;
#15211 = CARTESIAN_POINT ( 'NONE',  ( 0.1574692315732393044, 5.243558859478304690, -9.238013023060988260 ) ) ;
#15212 = EDGE_CURVE ( 'NONE', #30805, #26351, #18786, .T. ) ;
#15213 = CARTESIAN_POINT ( 'NONE',  ( 21.86000000136559507, 1.570731468192929858, 2.892927487894329630 ) ) ;
#15214 = ADVANCED_FACE ( 'NONE', ( #18916 ), #13450, .F. ) ;
#15215 = CARTESIAN_POINT ( 'NONE',  ( -24.41293782978024041, 3.998227953278250535, 2.146185852361514268 ) ) ;
#15216 = CARTESIAN_POINT ( 'NONE',  ( 11.65799190157298781, -20.33406113955203409, -1.499999999999997780 ) ) ;
#15217 = LINE ( 'NONE', #10677, #4985 ) ;
#15218 = LINE ( 'NONE', #23073, #19921 ) ;
#15219 = DIRECTION ( 'NONE',  ( 1.000000000000000000, -0.000000000000000000, -0.000000000000000000 ) ) ;
#15220 = ORIENTED_EDGE ( 'NONE', *, *, #3636, .T. ) ;
#15221 = PLANE ( 'NONE',  #5494 ) ;
#15222 = APPROVAL_STATUS ( 'not_yet_approved' ) ;
#15223 = CARTESIAN_POINT ( 'NONE',  ( 1.624999999999999778, -9.915734732513254102, 4.762163868918234400 ) ) ;
#15224 = ORIENTED_EDGE ( 'NONE', *, *, #12803, .F. ) ;
#15225 = CARTESIAN_POINT ( 'NONE',  ( 107.5866720633429878, 18.70855422806117474, -5.131518431764148680 ) ) ;
#15226 = ORIENTED_EDGE ( 'NONE', *, *, #21793, .F. ) ;
#15227 = CARTESIAN_POINT ( 'NONE',  ( -23.08853323649765343, 18.46223496596753932, 1.773004750130224627 ) ) ;
#15229 = ORIENTED_EDGE ( 'NONE', *, *, #13642, .F. ) ;
#15228 = CARTESIAN_POINT ( 'NONE',  ( 18.85982315263666464, -4.744118555706133833, -4.006107076250019716 ) ) ;
#15230 = ORIENTED_EDGE ( 'NONE', *, *, #14276, .F. ) ;
#15231 = CARTESIAN_POINT ( 'NONE',  ( -1.738758153310166144, 1.323625320507516134, 3.284597389079960461 ) ) ;
#15232 = CARTESIAN_POINT ( 'NONE',  ( -6.412550801365592967, 1.828967928396027398, -3.368539882008727115 ) ) ;
#15233 = DIRECTION ( 'NONE',  ( -1.000000000000000000, 0.000000000000000000, 0.000000000000000000 ) ) ;
#15234 = CARTESIAN_POINT ( 'NONE',  ( 69.42401195566041849, -8.835509274224046194, -0.07017451552783579571 ) ) ;
#15236 = VERTEX_POINT ( 'NONE', #21583 ) ;
#15235 = CARTESIAN_POINT ( 'NONE',  ( 25.75999999999999801, -2.208672634433321348E-15, 0.000000000000000000 ) ) ;
#15237 = DIRECTION ( 'NONE',  ( -0.000000000000000000, -0.000000000000000000, -1.000000000000000000 ) ) ;
#15238 = DIRECTION ( 'NONE',  ( 0.000000000000000000, 0.000000000000000000, 1.000000000000000000 ) ) ;
#15239 = CARTESIAN_POINT ( 'NONE',  ( 3.503000659536867900, -17.24537520706771687, 1.500000000000951017 ) ) ;
#15240 = CARTESIAN_POINT ( 'NONE',  ( 7.278212735265215727, -5.482579124930866854, -1.000000000000000000 ) ) ;
#15242 = ORIENTED_EDGE ( 'NONE', *, *, #20764, .F. ) ;
#15241 = CARTESIAN_POINT ( 'NONE',  ( -34.48223484310472031, 0.000000000000000000, 13.00000000000004441 ) ) ;
#15243 = DIRECTION ( 'NONE',  ( -0.9975973382524638833, -0.06927878976713691683, 0.000000000000000000 ) ) ;
#15244 = EDGE_CURVE ( 'NONE', #29424, #15425, #9437, .T. ) ;
#15245 = B_SPLINE_CURVE_WITH_KNOTS ( 'NONE', 3,
 ( #11279, #13768, #13169, #19130, #24146, #1273, #1428, #13924, #21489, #26648, #31701, #8779, #18984, #29170, #11604, #18372 ),
 .UNSPECIFIED., .F., .F.,
 ( 4, 2, 2, 2, 2, 2, 2, 4 ),
 ( 0.01324599089036895827, 0.5000000000000000000, 0.6250000000000000000, 0.7500000000000000000, 0.8125000000000000000, 0.8749999999999998890, 0.9375000000000000000, 1.000000000000000000 ),
 .UNSPECIFIED. ) ;
#15246 = CYLINDRICAL_SURFACE ( 'NONE', #10268, 0.5000000000000000000 ) ;
#15247 = CARTESIAN_POINT ( 'NONE',  ( 24.11000000273118715, 1.573300977624590313, -1.942864903642426144 ) ) ;
#15248 = CARTESIAN_POINT ( 'NONE',  ( 5.139557470515282267E-15, 0.000000000000000000, -4.137834579201380869 ) ) ;
#15249 = DIRECTION ( 'NONE',  ( -1.000000000000000000, 8.574039729943019576E-17, -0.000000000000000000 ) ) ;
#15250 = CARTESIAN_POINT ( 'NONE',  ( -2.672624763096117739, -0.4219952926969700591, -1.725256589882067093 ) ) ;
#15251 = ORIENTED_EDGE ( 'NONE', *, *, #8201, .F. ) ;
#15252 = CARTESIAN_POINT ( 'NONE',  ( 3.499999999999999556, 7.003298780661427969, 4.817032923780590004 ) ) ;
#15253 = CARTESIAN_POINT ( 'NONE',  ( 4.749760686538667009, 6.139290821770327256, -5.151476664237414127 ) ) ;
#15254 = CARTESIAN_POINT ( 'NONE',  ( -7.837550801365593678, 1.088641768524161613, 3.675193018007246959 ) ) ;
#15255 = VERTEX_POINT ( 'NONE', #6515 ) ;
#15256 = PLANE ( 'NONE',  #15126 ) ;
#15257 = CARTESIAN_POINT ( 'NONE',  ( 0.000000000000000000, -4.147285340411747789, -5.698247474649445365 ) ) ;
#15258 = ADVANCED_FACE ( 'NONE', ( #21246 ), #8522, .T. ) ;
#15259 = CARTESIAN_POINT ( 'NONE',  ( 41.06247019076344884, -19.55897407381494091, -1.500000000000000444 ) ) ;
#15260 = ORIENTED_EDGE ( 'NONE', *, *, #17101, .T. ) ;
#15261 = CARTESIAN_POINT ( 'NONE',  ( 10.75691143517498283, -12.51424465391554719, 1.000000000000000000 ) ) ;
#15262 = ORIENTED_EDGE ( 'NONE', *, *, #20033, .T. ) ;
#15263 = CARTESIAN_POINT ( 'NONE',  ( -41.86373177837820236, -16.13513036599589867, 5.128141679950118714 ) ) ;
#15264 = ORIENTED_EDGE ( 'NONE', *, *, #4261, .F. ) ;
#15265 = CARTESIAN_POINT ( 'NONE',  ( 23.61632761762314203, -8.296864917633476111, 2.713652344655544724 ) ) ;
#15267 = ORIENTED_EDGE ( 'NONE', *, *, #7184, .F. ) ;
#15266 = DIRECTION ( 'NONE',  ( -0.000000000000000000, 0.000000000000000000, 1.000000000000000000 ) ) ;
#15268 = ADVANCED_FACE ( 'NONE', ( #2166 ), #4933, .T. ) ;
#15269 = VERTEX_POINT ( 'NONE', #27074 ) ;
#15270 = CARTESIAN_POINT ( 'NONE',  ( -23.85705198072715660, 13.77387538314364335, 1.500000000000000000 ) ) ;
#15271 = VERTEX_POINT ( 'NONE', #11869 ) ;
#15272 = DIRECTION ( 'NONE',  ( 0.000000000000000000, 0.000000000000000000, 1.000000000000000000 ) ) ;
#15274 = ORIENTED_EDGE ( 'NONE', *, *, #11285, .F. ) ;
#15273 = CARTESIAN_POINT ( 'NONE',  ( 0.8174570305809125692, -9.170357625429589987, -1.500000000000000000 ) ) ;
#15275 = CARTESIAN_POINT ( 'NONE',  ( -5.312942406915326821, -3.366872799099910998E-15, -3.000000000000000000 ) ) ;
#15276 = EDGE_CURVE ( 'NONE', #23760, #6020, #18260, .T. ) ;
#15277 = CARTESIAN_POINT ( 'NONE',  ( 56.97280603064898941, -277.2763395528616002, -2.334455007174250696 ) ) ;
#15278 = CARTESIAN_POINT ( 'NONE',  ( 69.18703749905368738, -4.112663945013685485, -4.522129901861162260 ) ) ;
#15279 = CARTESIAN_POINT ( 'NONE',  ( 0.1081011292492479320, -10.52678838719862142, 2.097343412299245369 ) ) ;
#15280 = DIRECTION ( 'NONE',  ( 8.574039729943018344E-17, 1.000000000000000000, 0.000000000000000000 ) ) ;
#15281 = DIRECTION ( 'NONE',  ( -0.000000000000000000, -0.000000000000000000, -1.000000000000000000 ) ) ;
#15282 = CARTESIAN_POINT ( 'NONE',  ( 25.34157222223575445, -17.52646456585306822, 1.103933258152489882 ) ) ;
#15283 = ADVANCED_FACE ( 'NONE', ( #6690 ), #24394, .F. ) ;
#15284 = EDGE_CURVE ( 'NONE', #24285, #20638, #32212, .T. ) ;
#15285 = CARTESIAN_POINT ( 'NONE',  ( 18.53175858344379634, -21.44524224917989130, 1.500000000000000000 ) ) ;
#15286 = CARTESIAN_POINT ( 'NONE',  ( 0.000000000000000000, 6.226349476952025341, -0.5315761383463578627 ) ) ;
#15287 = CARTESIAN_POINT ( 'NONE',  ( 6.880159790065803804, 8.691376398188699781, 0.8322990769132707634 ) ) ;
#15288 = CARTESIAN_POINT ( 'NONE',  ( 47.68482864957696421, -3.825617316378856714, 0.07017451550799964910 ) ) ;
#15289 = CARTESIAN_POINT ( 'NONE',  ( 85.20563808598728883, -3.194259795296060300, 4.522129901861162260 ) ) ;
#15290 = ADVANCED_FACE ( 'NONE', ( #22386 ), #8634, .T. ) ;
#15291 = DIRECTION ( 'NONE',  ( 0.000000000000000000, 0.000000000000000000, -1.000000000000000000 ) ) ;
#15292 = ORIENTED_EDGE ( 'NONE', *, *, #13896, .T. ) ;
#15293 = CARTESIAN_POINT ( 'NONE',  ( -7.087550801365593678, 2.228590825266444142, 2.752080473201636845 ) ) ;
#15294 = CARTESIAN_POINT ( 'NONE',  ( 0.7632845268398871230, 3.174628368996073924, 8.152713396088772768 ) ) ;
#15295 = ORIENTED_EDGE ( 'NONE', *, *, #22819, .T. ) ;
#15296 = CARTESIAN_POINT ( 'NONE',  ( 101.9216173105994443, -5.769792427975428240, -0.07017451552783622593 ) ) ;
#15297 = DIRECTION ( 'NONE',  ( 0.000000000000000000, 0.000000000000000000, 1.000000000000000000 ) ) ;
#15298 = EDGE_CURVE ( 'NONE', #2614, #17163, #22540, .T. ) ;
#15299 = ORIENTED_EDGE ( 'NONE', *, *, #6048, .F. ) ;
#15300 = FACE_OUTER_BOUND ( 'NONE', #5700, .T. ) ;
#15301 = DATE_AND_TIME ( #32544, #14613 ) ;
#15303 = ORIENTED_EDGE ( 'NONE', *, *, #7148, .T. ) ;
#15302 = CARTESIAN_POINT ( 'NONE',  ( 1.624999999999999778, 4.762163868918416476, -9.915734732513170613 ) ) ;
#15304 = EDGE_LOOP ( 'NONE', ( #29611, #5671, #18214, #17548 ) ) ;
#15305 = CARTESIAN_POINT ( 'NONE',  ( 0.08995365929913461123, -14.90597059099496136, 1.745535636305011629 ) ) ;
#15306 = EDGE_LOOP ( 'NONE', ( #18079, #12703, #9185, #20978 ) ) ;
#15307 = CARTESIAN_POINT ( 'NONE',  ( 108.0223616456019471, -18.39136425041039402, -4.509695625108203210 ) ) ;
#15309 = ORIENTED_EDGE ( 'NONE', *, *, #24874, .F. ) ;
#15308 = CARTESIAN_POINT ( 'NONE',  ( -2.767073886773233848, -0.6621507858625358400, 1.748408842879327851 ) ) ;
#15310 = CARTESIAN_POINT ( 'NONE',  ( 41.45057005843676734, -9.239282957736858037, 1.915219082070893863 ) ) ;
#15311 = DIRECTION ( 'NONE',  ( 0.000000000000000000, -0.08715574274765533480, -0.9961946980917457672 ) ) ;
#15312 = EDGE_CURVE ( 'NONE', #1130, #24626, #27837, .T. ) ;
#15313 = CARTESIAN_POINT ( 'NONE',  ( 22.00639167669224960, -21.80013755708282730, -1.499999999999999556 ) ) ;
#15314 = DIRECTION ( 'NONE',  ( 0.000000000000000000, 0.000000000000000000, 1.000000000000000000 ) ) ;
#15315 = EDGE_LOOP ( 'NONE', ( #25234, #32310, #6802, #497 ) ) ;
#15316 = DIRECTION ( 'NONE',  ( 0.000000000000000000, 0.000000000000000000, 1.000000000000000000 ) ) ;
#15317 = CARTESIAN_POINT ( 'NONE',  ( 48.06508596181272708, -7.548662730762578654, 4.522129901861162260 ) ) ;
#15318 = CARTESIAN_POINT ( 'NONE',  ( 4.749760686538667009, -1.391664247347174754, -7.892520144992448472 ) ) ;
#15319 = PLANE ( 'NONE',  #3973 ) ;
#15320 = EDGE_CURVE ( 'NONE', #7656, #6904, #20939, .T. ) ;
#15321 = EDGE_CURVE ( 'NONE', #21704, #4740, #18658, .T. ) ;
#15322 = DIRECTION ( 'NONE',  ( 0.000000000000000000, -0.08715574274764385787, -0.9961946980917467664 ) ) ;
#15323 = CARTESIAN_POINT ( 'NONE',  ( 0.5032039692105046980, -0.7352278974791391919, 9.704418393844074231 ) ) ;
#15324 = FACE_OUTER_BOUND ( 'NONE', #16446, .T. ) ;
#15325 = CARTESIAN_POINT ( 'NONE',  ( -1.176310634206514104E-14, 21.94000000000002260, -1.050000000000000044 ) ) ;
#15326 = ORIENTED_EDGE ( 'NONE', *, *, #1911, .F. ) ;
#15327 = CARTESIAN_POINT ( 'NONE',  ( -5.562550801365593323, 2.752080473201636845, -2.228590825266444142 ) ) ;
#15328 = ORIENTED_EDGE ( 'NONE', *, *, #2633, .F. ) ;
#15329 = CARTESIAN_POINT ( 'NONE',  ( -8.350050799999999995, 3.113457007523260156, -0.9222479816126439855 ) ) ;
#15330 = CARTESIAN_POINT ( 'NONE',  ( 24.17250000136559507, -3.024605502323851169, 0.3178988483021052969 ) ) ;
#15331 = CARTESIAN_POINT ( 'NONE',  ( 107.4927781683577734, 18.16905313753168016, 5.010584227462816287 ) ) ;
#15332 = CARTESIAN_POINT ( 'NONE',  ( 0.2210079091045983601, -7.685141149027079344, 1.773955204205442060 ) ) ;
#15333 = CARTESIAN_POINT ( 'NONE',  ( 11.50505501463784697, -13.50304080202605306, 1.500000000000000000 ) ) ;
#15334 = VERTEX_POINT ( 'NONE', #22077 ) ;
#15335 = DIRECTION ( 'NONE',  ( 0.000000000000000000, 1.598721155460225418E-14, 1.000000000000000000 ) ) ;
#15336 = EDGE_CURVE ( 'NONE', #10493, #3168, #12187, .T. ) ;
#15337 =( BOUNDED_CURVE ( )  B_SPLINE_CURVE ( 2, ( #1105, #31721, #16811, #27011, #16458, #4113, #24475, #1593, #27337, #24831, #27662 ),
 .UNSPECIFIED., .F., .F. ) 
 B_SPLINE_CURVE_WITH_KNOTS ( ( 3, 2, 2, 2, 2, 3 ),
 ( 0.2966116191895003529, 0.2999999999999999889, 0.3250000000000000111, 0.3499999999999999778, 0.3750000000000000000, 0.3966116191895003862 ),
 .UNSPECIFIED. ) 
 CURVE ( )  GEOMETRIC_REPRESENTATION_ITEM ( )  RATIONAL_B_SPLINE_CURVE ( ( 0.9821626249036858880, 0.9896829947469992783, 1.000000000000000000, 0.9238795325112867385, 1.000000000000000000, 0.9238795325112867385, 1.000000000000000000, 0.9238795325112867385, 1.000000000000000000, 0.9341965377642874602, 0.9821626249036858880 ) ) 
 REPRESENTATION_ITEM ( '' )  );
#15338 = PRODUCT_RELATED_PRODUCT_CATEGORY ( 'detail', '', ( #2027 ) ) ;
#15339 = ORIENTED_EDGE ( 'NONE', *, *, #18077, .F. ) ;
#15340 = CARTESIAN_POINT ( 'NONE',  ( 7.249760686538667009, -4.007137495034764463, -6.940565734314639634 ) ) ;
#15341 = APPROVAL_STATUS ( 'not_yet_approved' ) ;
#15342 = CARTESIAN_POINT ( 'NONE',  ( 40.88376184144740222, -6.854209834395733836, 4.053847216738481585 ) ) ;
#15343 = DIRECTION ( 'NONE',  ( 0.000000000000000000, 0.000000000000000000, 1.000000000000000000 ) ) ;
#15345 = CARTESIAN_POINT ( 'NONE',  ( 0.000000000000000000, -6.700937042937042065, 0.8165525598867410251 ) ) ;
#15344 = DIRECTION ( 'NONE',  ( -1.000000000000000000, 0.000000000000000000, -0.000000000000000000 ) ) ;
#15346 = ORIENTED_EDGE ( 'NONE', *, *, #20919, .T. ) ;
#15347 = CARTESIAN_POINT ( 'NONE',  ( -7.750050802731187183, 0.3135853898029611342, -2.983565686104819648 ) ) ;
#15348 = DIRECTION ( 'NONE',  ( 0.4999999999999977796, 0.8660254037844398178, 0.000000000000000000 ) ) ;
#15349 = EDGE_CURVE ( 'NONE', #9882, #29104, #21977, .T. ) ;
#15350 = CARTESIAN_POINT ( 'NONE',  ( 25.17250000136559507, -3.024605502323851169, 0.3178988483021052969 ) ) ;
#15351 = LINE ( 'NONE', #18191, #10243 ) ;
#15353 = ORIENTED_EDGE ( 'NONE', *, *, #9196, .T. ) ;
#15352 = CARTESIAN_POINT ( 'NONE',  ( 6.883866482134012976, 8.691827696555170846, -0.8319830743949774288 ) ) ;
#15354 = CARTESIAN_POINT ( 'NONE',  ( -7.012550801365593500, 3.368539882008727115, 1.828967928396026954 ) ) ;
#15355 = FACE_OUTER_BOUND ( 'NONE', #26308, .T. ) ;
#15356 = CYLINDRICAL_SURFACE ( 'NONE', #22004, 5.010000000000000675 ) ;
#15357 = CARTESIAN_POINT ( 'NONE',  ( 10.00000000000000000, -4.116875700062100130, 2.376879293651050329 ) ) ;
#15358 = ORIENTED_EDGE ( 'NONE', *, *, #18402, .F. ) ;
#15360 = VERTEX_POINT ( 'NONE', #24552 ) ;
#15359 = CARTESIAN_POINT ( 'NONE',  ( 0.6728001046013614150, 3.357496170308760242, -8.512517952453828585 ) ) ;
#15361 = DIRECTION ( 'NONE',  ( 0.000000000000000000, 0.000000000000000000, -1.000000000000000000 ) ) ;
#15362 = CARTESIAN_POINT ( 'NONE',  ( -28.64263641446437347, 5.485000000000014531, 1.500000000000000000 ) ) ;
#15363 = CARTESIAN_POINT ( 'NONE',  ( 23.54750000136559862, 1.913930629741522838, -2.363507492473150062 ) ) ;
#15364 = CARTESIAN_POINT ( 'NONE',  ( 28.69355067553088645, -5.615744008485835437, 3.993434336029700216 ) ) ;
#15365 = CARTESIAN_POINT ( 'NONE',  ( 2.976845726615125809, 2.305279507610603851, 8.871766062375160189 ) ) ;
#15366 = CYLINDRICAL_SURFACE ( 'NONE', #19394, 5.010000000000000675 ) ;
#15367 = CARTESIAN_POINT ( 'NONE',  ( 8.911384905465473238, 0.2172754300402719996, 1.412391582771868492 ) ) ;
#15368 = CARTESIAN_POINT ( 'NONE',  ( 107.9462823452557814, -17.29584125157287744, 3.322807143010101605 ) ) ;
#15369 = VERTEX_POINT ( 'NONE', #19904 ) ;
#15370 = CARTESIAN_POINT ( 'NONE',  ( 101.6441386174529953, -1.774168274679931212, 2.184956718805492581 ) ) ;
#15371 = EDGE_CURVE ( 'NONE', #31221, #3483, #21461, .T. ) ;
#15372 = CARTESIAN_POINT ( 'NONE',  ( 101.8797206818349821, -5.166491396337139719, -2.184956718990371805 ) ) ;
#15373 = ORIENTED_EDGE ( 'NONE', *, *, #29310, .T. ) ;
#15374 = FACE_OUTER_BOUND ( 'NONE', #21779, .T. ) ;
#15375 = ORIENTED_EDGE ( 'NONE', *, *, #17467, .F. ) ;
#15376 = CARTESIAN_POINT ( 'NONE',  ( -22.41343429466623149, 4.100545212957339203, 2.143340414843532660 ) ) ;
#15378 = ORIENTED_EDGE ( 'NONE', *, *, #29744, .T. ) ;
#15377 = CARTESIAN_POINT ( 'NONE',  ( 40.87776742365452520, -5.755143957976294189, -4.003574183526315444 ) ) ;
#15379 = ORIENTED_EDGE ( 'NONE', *, *, #18557, .T. ) ;
#15380 = EDGE_CURVE ( 'NONE', #26222, #21921, #28412, .T. ) ;
#15381 = CARTESIAN_POINT ( 'NONE',  ( 6.655951778521610684, -18.71196003547629516, 1.500000000000000000 ) ) ;
#15382 = CARTESIAN_POINT ( 'NONE',  ( -7.312550801365594211, -1.088641768524163611, -3.675193018007245627 ) ) ;
#15383 = EDGE_CURVE ( 'NONE', #23656, #18044, #28971, .T. ) ;
#15384 = CARTESIAN_POINT ( 'NONE',  ( 5.887530024394195038, -8.008238305624862718, 2.518482652462528115 ) ) ;
#15385 = CARTESIAN_POINT ( 'NONE',  ( 107.5719395156074540, -19.12968270266287618, -4.222684948861750165 ) ) ;
#15387 = ORIENTED_EDGE ( 'NONE', *, *, #13433, .F. ) ;
#15386 = DIRECTION ( 'NONE',  ( 1.000000000000000000, -8.574039729943018344E-17, -0.000000000000000000 ) ) ;
#15388 = CARTESIAN_POINT ( 'NONE',  ( 22.30656763371926843, -0.8852964313267484009, 2.499999999999997780 ) ) ;
#15389 = ADVANCED_FACE ( 'NONE', ( #32943 ), #10667, .F. ) ;
#15390 = CARTESIAN_POINT ( 'NONE',  ( -3.806139276275473105, -9.688921910891492573, 1.499999999999999112 ) ) ;
#15391 = CARTESIAN_POINT ( 'NONE',  ( 24.67250000136559507, 2.363507492473148286, 1.913930629741525058 ) ) ;
#15392 = DIRECTION ( 'NONE',  ( 0.000000000000000000, 0.000000000000000000, 1.000000000000000000 ) ) ;
#15394 = VERTEX_POINT ( 'NONE', #12532 ) ;
#15393 = CARTESIAN_POINT ( 'NONE',  ( 18.60867489490414428, -7.551452029063769444, -0.8134928201658568891 ) ) ;
#15395 = LINE ( 'NONE', #13218, #17834 ) ;
#15396 = CARTESIAN_POINT ( 'NONE',  ( -27.70590053552606591, 16.86946294693127157, 1.811428998031433535 ) ) ;
#15397 = CARTESIAN_POINT ( 'NONE',  ( 22.23500000136559862, -1.570731468192933633, -2.892927487894330074 ) ) ;
#15398 = DIRECTION ( 'NONE',  ( -0.4999999999999981681, -0.8660254037844395958, 0.000000000000000000 ) ) ;
#15399 = CARTESIAN_POINT ( 'NONE',  ( -2.037945749704337831E-16, -2.376879293651093406, 4.116875700062075261 ) ) ;
#15400 = DIRECTION ( 'NONE',  ( -0.1027947991993876653, 0.9947025833170222153, 0.000000000000000000 ) ) ;
#15401 = VERTEX_POINT ( 'NONE', #20571 ) ;
#15402 = CARTESIAN_POINT ( 'NONE',  ( 43.06800534735074137, -24.01680020629799728, 1.500000000000000000 ) ) ;
#15403 = DIRECTION ( 'NONE',  ( 0.000000000000000000, -0.9961946980917442129, -0.08715574274767322327 ) ) ;
#15404 = CARTESIAN_POINT ( 'NONE',  ( 107.4616189337527885, -17.52789370703686345, -4.846792217672044600 ) ) ;
#15405 = ORIENTED_EDGE ( 'NONE', *, *, #19911, .F. ) ;
#15406 = LINE ( 'NONE', #23431, #23676 ) ;
#15407 = DIRECTION ( 'NONE',  ( -1.000000000000000000, 0.000000000000000000, 0.000000000000000000 ) ) ;
#15408 = CARTESIAN_POINT ( 'NONE',  ( 3.529609406779910419, -12.17998485103522199, -1.500000000000000444 ) ) ;
#15409 = CARTESIAN_POINT ( 'NONE',  ( 29.18953645666585217, -9.308308156628569918, 0.07017451552781736601 ) ) ;
#15410 = VERTEX_POINT ( 'NONE', #15016 ) ;
#15411 = EDGE_CURVE ( 'NONE', #26986, #19129, #10170, .T. ) ;
#15412 = CARTESIAN_POINT ( 'NONE',  ( 7.249760686538667009, 0.000000000000000000, 0.000000000000000000 ) ) ;
#15413 = ORIENTED_EDGE ( 'NONE', *, *, #6788, .T. ) ;
#15414 = CARTESIAN_POINT ( 'NONE',  ( 107.4500593345382811, -17.36019228850094720, 4.522129901861156931 ) ) ;
#15416 = ORIENTED_EDGE ( 'NONE', *, *, #27056, .T. ) ;
#15415 = DIRECTION ( 'NONE',  ( 0.000000000000000000, 0.000000000000000000, 1.000000000000000000 ) ) ;
#15417 = B_SPLINE_CURVE_WITH_KNOTS ( 'NONE', 3,
 ( #21590, #31798, #20931, #8239, #14354, #24911, #32613, #4187 ),
 .UNSPECIFIED., .F., .F.,
 ( 4, 2, 2, 4 ),
 ( 2.494123658409239446E-07, 0.001262099805927724113, 0.001893025002708666410, 0.002523950199489608925 ),
 .UNSPECIFIED. ) ;
#15418 = ORIENTED_EDGE ( 'NONE', *, *, #9574, .T. ) ;
#15419 = DIRECTION ( 'NONE',  ( -0.9895623637898895986, 0.1441052676711233327, 0.000000000000000000 ) ) ;
#15420 = ADVANCED_FACE ( 'NONE', ( #17889 ), #15356, .T. ) ;
#15421 = EDGE_CURVE ( 'NONE', #31932, #16406, #10359, .T. ) ;
#15422 = ORIENTED_EDGE ( 'NONE', *, *, #31861, .F. ) ;
#15423 = CARTESIAN_POINT ( 'NONE',  ( 7.249760686538667009, -7.906491560603638113, -3.748318449932378282 ) ) ;
#15425 = VERTEX_POINT ( 'NONE', #7849 ) ;
#15424 = CARTESIAN_POINT ( 'NONE',  ( 41.06247019076344884, -19.55897407381494091, -1.500000000000000000 ) ) ;
#15426 = DIRECTION ( 'NONE',  ( -7.472768010111467553E-18, -0.08715574274766195451, 0.9961946980917452121 ) ) ;
#15427 = CARTESIAN_POINT ( 'NONE',  ( 1.067267558240149850, -2.636048217392937154, -1.760945737653910825 ) ) ;
#15428 = CARTESIAN_POINT ( 'NONE',  ( 1.959487840848906148E-16, 2.285372942704953392, 4.458382051008201508 ) ) ;
#15429 = CARTESIAN_POINT ( 'NONE',  ( 15.81086013898703690, -14.68957282009552756, -1.500000000000274447 ) ) ;
#15430 = DIRECTION ( 'NONE',  ( 0.000000000000000000, -0.2079116908177663092, 0.9781476007338040235 ) ) ;
#15431 = DIRECTION ( 'NONE',  ( 0.9896144216807899463, -0.000000000000000000, 0.1437473352845035635 ) ) ;
#15432 = CARTESIAN_POINT ( 'NONE',  ( 1.624999999999999778, -7.958834565716820464, 7.593217523260554103 ) ) ;
#15433 = CARTESIAN_POINT ( 'NONE',  ( 14.72414172255109222, -15.74544918409871741, 1.500000000000000444 ) ) ;
#15434 = CARTESIAN_POINT ( 'NONE',  ( 18.65791233782558933, -7.001076235494291033, 2.184956778801695254 ) ) ;
#15435 = B_SPLINE_CURVE_WITH_KNOTS ( 'NONE', 3,
 ( #16784, #27299, #21784, #19471, #4083, #11942, #31992, #1253 ),
 .UNSPECIFIED., .F., .F.,
 ( 4, 2, 2, 4 ),
 ( 2.737843117599802759E-07, 0.001261207499628692018, 0.001891674357287159150, 0.002522141214945626715 ),
 .UNSPECIFIED. ) ;
#15436 = CARTESIAN_POINT ( 'NONE',  ( 111.5384102276623395, -20.44549501350944709, 0.9788672205877712029 ) ) ;
#15437 = CARTESIAN_POINT ( 'NONE',  ( 23.58234648083524121, -8.048792613698569909, -0.07017451552783579571 ) ) ;
#15438 = VECTOR ( 'NONE', #19991, 1000.000000000000114 ) ;
#15439 = CARTESIAN_POINT ( 'NONE',  ( 23.73500000000000298, -0.2613211581691358698, -2.486304738420681559 ) ) ;
#15440 = CARTESIAN_POINT ( 'NONE',  ( 109.4269204153489454, 20.46634128985479961, 2.043459224939188967 ) ) ;
#15441 = APPLICATION_CONTEXT ( 'configuration controlled 3d designs of mechanical parts and assemblies' ) ;
#15442 = CARTESIAN_POINT ( 'NONE',  ( 19.03654924710325602, -2.768675503676416572, 2.713652344655542503 ) ) ;
#15443 = CARTESIAN_POINT ( 'NONE',  ( -17.45597128428592981, -25.93932300454937945, 11.00000000000000000 ) ) ;
#15444 = ORIENTED_EDGE ( 'NONE', *, *, #29075, .F. ) ;
#15445 = CARTESIAN_POINT ( 'NONE',  ( -5.937550801365592434, -3.368539882008727115, -1.828967928396028064 ) ) ;
#15446 = EDGE_CURVE ( 'NONE', #18474, #32515, #21790, .T. ) ;
#15447 = DIRECTION ( 'NONE',  ( 0.000000000000000000, 0.000000000000000000, 1.000000000000000000 ) ) ;
#15448 = FACE_OUTER_BOUND ( 'NONE', #16530, .T. ) ;
#15449 = ORIENTED_EDGE ( 'NONE', *, *, #3496, .F. ) ;
#15450 = CARTESIAN_POINT ( 'NONE',  ( 41.43141396789281572, -2.886852813804338780, -0.07017451552781628354 ) ) ;
#15451 = AXIS2_PLACEMENT_3D ( 'NONE', #9951, #30210, #20015 ) ;
#15452 = EDGE_CURVE ( 'NONE', #25811, #13759, #23465, .T. ) ;
#15453 = VECTOR ( 'NONE', #27257, 1000.000000000000000 ) ;
#15454 = EDGE_LOOP ( 'NONE', ( #13124, #3536, #10083, #7894 ) ) ;
#15455 = DIRECTION ( 'NONE',  ( 0.2951703194034057121, -0.3797261271633443069, -0.8767454310646958238 ) ) ;
#15456 = ITEM_DEFINED_TRANSFORMATION ( 'NONE', 'NONE', #11372,  #2865 ) ;
#15458 = VERTEX_POINT ( 'NONE', #23379 ) ;
#15457 = CARTESIAN_POINT ( 'NONE',  ( 35.16139127360178662, -8.400504373793673096, 0.07017451552781736601 ) ) ;
#15460 = EDGE_CURVE ( 'NONE', #3262, #20824, #30421, .T. ) ;
#15459 = ORIENTED_EDGE ( 'NONE', *, *, #4285, .F. ) ;
#15461 = CARTESIAN_POINT ( 'NONE',  ( 2.274274201625327230, 1.464956435139694868, -10.90201369670497122 ) ) ;
#15462 = ORIENTED_EDGE ( 'NONE', *, *, #2402, .T. ) ;
#15463 = AXIS2_PLACEMENT_3D ( 'NONE', #14775, #4755, #2438 ) ;
#15464 = DIRECTION ( 'NONE',  ( 0.000000000000000000, 0.9993908270190956511, 0.03489949670250104552 ) ) ;
#15466 = ORIENTED_EDGE ( 'NONE', *, *, #13719, .F. ) ;
#15465 = CARTESIAN_POINT ( 'NONE',  ( -10.00000000000000000, 0.000000000000000000, 0.000000000000000000 ) ) ;
#15467 = CARTESIAN_POINT ( 'NONE',  ( 22.28390758787569581, 17.05912403623761975, 1.049999999999999822 ) ) ;
#15468 = CYLINDRICAL_SURFACE ( 'NONE', #4784, 8.749000000000002331 ) ;
#15469 = EDGE_CURVE ( 'NONE', #10288, #7687, #5178, .T. ) ;
#15470 = FACE_OUTER_BOUND ( 'NONE', #30885, .T. ) ;
#15471 = FACE_OUTER_BOUND ( 'NONE', #8998, .T. ) ;
#15472 = VERTEX_POINT ( 'NONE', #28231 ) ;
#15473 = PLANE ( 'NONE',  #22441 ) ;
#15474 = LINE ( 'NONE', #25686, #24150 ) ;
#15475 = FACE_OUTER_BOUND ( 'NONE', #16258, .T. ) ;
#15476 = DIRECTION ( 'NONE',  ( -1.000000000000000000, -0.000000000000000000, -0.000000000000000000 ) ) ;
#15477 = EDGE_CURVE ( 'NONE', #9323, #28886, #29483, .T. ) ;
#15478 = CARTESIAN_POINT ( 'NONE',  ( 24.43238093800358968, -17.43085383294892665, 1.450662971657243006 ) ) ;
#15479 = CARTESIAN_POINT ( 'NONE',  ( -7.250050802731188071, -2.331437884370912705, 1.887961173149512062 ) ) ;
#15480 = CARTESIAN_POINT ( 'NONE',  ( -56.31169168320045770, 1.934928713445239489E-05, -1.021773151746335095 ) ) ;
#15481 = CARTESIAN_POINT ( 'NONE',  ( 23.22564502775751194, -21.93932300456764040, 1.023882905580708380 ) ) ;
#15482 = CIRCLE ( 'NONE', #30441, 10.94895958125474245 ) ;
#15483 = ORIENTED_EDGE ( 'NONE', *, *, #16304, .T. ) ;
#15484 = CARTESIAN_POINT ( 'NONE',  ( -6.462550801365593678, 0.3701630799359330593, -3.521866450007987037 ) ) ;
#15485 = VERTEX_POINT ( 'NONE', #8002 ) ;
#15486 = CARTESIAN_POINT ( 'NONE',  ( -3.854531657079157014, -2.846291840500172921, -1.545410377633947618 ) ) ;
#15487 = CIRCLE ( 'NONE', #1061, 297.0265809045899346 ) ;
#15488 = CARTESIAN_POINT ( 'NONE',  ( 108.1273057862948974, 18.88704877543205640, 5.058538142693402406 ) ) ;
#15489 = CARTESIAN_POINT ( 'NONE',  ( 10.69474453358853872, -15.18614050023080608, 1.754319658296275009 ) ) ;
#15490 = CARTESIAN_POINT ( 'NONE',  ( 12.08436850396594409, -13.77779907615654231, 1.500000000000000000 ) ) ;
#15491 = ORIENTED_EDGE ( 'NONE', *, *, #5851, .F. ) ;
#15492 = CARTESIAN_POINT ( 'NONE',  ( 10.00000000000000178, -3.672404558090015758, -3.407865132560221166 ) ) ;
#15493 = B_SPLINE_CURVE_WITH_KNOTS ( 'NONE', 3,
 ( #3889, #14368, #31963, #12065, #9211, #24576, #19440, #26770, #11714, #19745 ),
 .UNSPECIFIED., .F., .F.,
 ( 4, 2, 2, 2, 4 ),
 ( 0.000000000000000000, 0.0005028294029233987402, 0.001005658805846797480, 0.002011317611693595828, 0.004022635223387192524 ),
 .UNSPECIFIED. ) ;
#15494 = EDGE_LOOP ( 'NONE', ( #23674, #4241, #29166, #24762 ) ) ;
#15495 = CARTESIAN_POINT ( 'NONE',  ( 1.184669658563290984, -2.669308969140904431, 1.499999999999999334 ) ) ;
#15496 = PERSON_AND_ORGANIZATION ( #6766, #25292 ) ;
#15497 = ADVANCED_FACE ( 'NONE', ( #483 ), #25732, .T. ) ;
#15498 = VECTOR ( 'NONE', #17686, 1000.000000000000000 ) ;
#15499 = CARTESIAN_POINT ( 'NONE',  ( 69.06945446451673831, -6.096442945251244971, 4.023790688806045956 ) ) ;
#15500 = EDGE_CURVE ( 'NONE', #3034, #8114, #16646, .T. ) ;
#15501 = AXIS2_PLACEMENT_3D ( 'NONE', #6944, #11636, #12291 ) ;
#15502 = CARTESIAN_POINT ( 'NONE',  ( 6.530491482054473273, -8.398420403995359607, -2.114164693852676358 ) ) ;
#15503 = VECTOR ( 'NONE', #7049, 1000.000000000000227 ) ;
#15505 = DIRECTION ( 'NONE',  ( 0.000000000000000000, 0.000000000000000000, 1.000000000000000000 ) ) ;
#15504 = DIRECTION ( 'NONE',  ( 0.000000000000000000, 0.000000000000000000, 1.000000000000000000 ) ) ;
#15506 = ORIENTED_EDGE ( 'NONE', *, *, #2402, .F. ) ;
#15507 = VECTOR ( 'NONE', #301, 1000.000000000000000 ) ;
#15508 = EDGE_CURVE ( 'NONE', #5774, #23867, #10239, .T. ) ;
#15509 = CARTESIAN_POINT ( 'NONE',  ( -7.600050802731185939, 3.113457007523260156, -0.9222479816126439855 ) ) ;
#15510 = CARTESIAN_POINT ( 'NONE',  ( 10.00000000000000000, -3.407865132560156329, -3.672404558090074378 ) ) ;
#15511 = CARTESIAN_POINT ( 'NONE',  ( 2.357330058169011977, -7.915524238820694336, -7.401770933800325913 ) ) ;
#15512 = DIRECTION ( 'NONE',  ( 1.000000000000000000, -0.000000000000000000, 0.000000000000000000 ) ) ;
#15513 = CIRCLE ( 'NONE', #1084, 0.4500000000000000111 ) ;
#15515 = ORIENTED_EDGE ( 'NONE', *, *, #10780, .T. ) ;
#15514 = CARTESIAN_POINT ( 'NONE',  ( 108.1608273670511267, 19.07371016407039122, -3.860697231985633415 ) ) ;
#15516 = CARTESIAN_POINT ( 'NONE',  ( -4.862550801365594033, 0.3701630799359330593, -3.521866450007987037 ) ) ;
#15517 = CARTESIAN_POINT ( 'NONE',  ( 10.00000000000000000, 4.787500056513365188, 1.476463073999653819 ) ) ;
#15518 = DIRECTION ( 'NONE',  ( 1.000000000000000000, 0.000000000000000000, 0.000000000000000000 ) ) ;
#15519 = CARTESIAN_POINT ( 'NONE',  ( 12.44989959798868817, 0.000000000000000000, 13.00000000000004441 ) ) ;
#15520 = ORIENTED_EDGE ( 'NONE', *, *, #7159, .T. ) ;
#15521 = VERTEX_POINT ( 'NONE', #19031 ) ;
#15522 = EDGE_CURVE ( 'NONE', #26215, #22604, #15045, .T. ) ;
#15523 = APPROVAL ( #9799, 'UNKNOWN' ) ;
#15524 = CARTESIAN_POINT ( 'NONE',  ( 17.41559371906258136, 18.02474698348859050, -1.491740999229419273 ) ) ;
#15525 = CARTESIAN_POINT ( 'NONE',  ( 0.6791198416089742063, 4.928602827912397011, -7.715582677071021855 ) ) ;
#15526 = PERSON ( 'NAUO-PER5', 'UNSPECIFIED', 'UNSPECIFIED', ('UNSPECIFIED'), ('UNSPECIFIED'), ('UNSPECIFIED') ) ;
#15527 = AXIS2_PLACEMENT_3D ( 'NONE', #30302, #7881, #2706 ) ;
#15528 = AXIS2_PLACEMENT_3D ( 'NONE', #13619, #23823, #15464 ) ;
#15529 = CARTESIAN_POINT ( 'NONE',  ( 23.86000000136559507, 1.570731468192929858, 2.892927487894329630 ) ) ;
#15530 = AXIS2_PLACEMENT_3D ( 'NONE', #22664, #78, #27654 ) ;
#15531 = VECTOR ( 'NONE', #18155, 1000.000000000000227 ) ;
#15532 = CARTESIAN_POINT ( 'NONE',  ( 0.6728000687415542913, 2.287261066729925574, 8.860258565202251191 ) ) ;
#15533 = FACE_OUTER_BOUND ( 'NONE', #32442, .T. ) ;
#15534 = VECTOR ( 'NONE', #10006, 1000.000000000000000 ) ;
#15535 = DIRECTION ( 'NONE',  ( 0.000000000000000000, 0.9063077870366522681, -0.4226182617406944453 ) ) ;
#15536 = CARTESIAN_POINT ( 'NONE',  ( 55.01832146648882116, -7.980226898950165904, 1.529339875099998913 ) ) ;
#15537 = ORIENTED_EDGE ( 'NONE', *, *, #21198, .F. ) ;
#15538 = CARTESIAN_POINT ( 'NONE',  ( 0.7632845268398871230, -7.360373001730951437, 4.729683950898845524 ) ) ;
#15539 = AXIS2_PLACEMENT_3D ( 'NONE', #8729, #18939, #24086 ) ;
#15540 = PERSON_AND_ORGANIZATION ( #6766, #25292 ) ;
#15541 = EDGE_CURVE ( 'NONE', #13010, #9377, #28927, .T. ) ;
#15542 = CARTESIAN_POINT ( 'NONE',  ( 40.73830215457859794, -6.894995700253241822, -3.993433058221939724 ) ) ;
#15543 = EDGE_LOOP ( 'NONE', ( #25699, #27488 ) ) ;
#15544 = CARTESIAN_POINT ( 'NONE',  ( 26.39808386558502562, 18.58254979424150832, 0.4463807625373201193 ) ) ;
#15545 = ORIENTED_EDGE ( 'NONE', *, *, #8473, .F. ) ;
#15546 = CARTESIAN_POINT ( 'NONE',  ( -17.11424327971897696, 13.04685258179087626, 1.906190955135662168 ) ) ;
#15548 = ORIENTED_EDGE ( 'NONE', *, *, #11670, .F. ) ;
#15547 = CARTESIAN_POINT ( 'NONE',  ( 18.84046687333923131, -4.960482910681117907, -4.215290389445589092 ) ) ;
#15549 = AXIS2_PLACEMENT_3D ( 'NONE', #25997, #10275, #5263 ) ;
#15550 = ORIENTED_EDGE ( 'NONE', *, *, #20235, .F. ) ;
#15551 = CARTESIAN_POINT ( 'NONE',  ( -18.30155664144426453, 0.000000000000000000, -3.895301350492843540 ) ) ;
#15552 = CARTESIAN_POINT ( 'NONE',  ( -6.712550801365592790, -3.675193018007245627, 1.088641768524163389 ) ) ;
#15553 = CARTESIAN_POINT ( 'NONE',  ( 10.00000000000000000, 3.672404558090085036, -3.407865132560141674 ) ) ;
#15554 = AXIS2_PLACEMENT_3D ( 'NONE', #17273, #32489, #9550 ) ;
#15555 = CARTESIAN_POINT ( 'NONE',  ( 85.49734435724779757, -7.913007294147515580, -1.010822989962099960 ) ) ;
#15557 = VERTEX_POINT ( 'NONE', #5818 ) ;
#15556 = CARTESIAN_POINT ( 'NONE',  ( 10.00000000000000000, -3.055657119358777152, -3.641590349731960163 ) ) ;
#15558 = CARTESIAN_POINT ( 'NONE',  ( 10.00000000000000000, 1.625881193364696609, 4.467071865485476856 ) ) ;
#15559 = AXIS2_PLACEMENT_3D ( 'NONE', #26137, #3245, #266 ) ;
#15560 = CARTESIAN_POINT ( 'NONE',  ( 22.25111450864416085, -3.256483526998273983E-15, 2.499999999999998668 ) ) ;
#15561 =( BOUNDED_SURFACE ( )  B_SPLINE_SURFACE ( 3, 2, ( 
 ( #16917, #27111, #4211 ),
 ( #12223, #14381, #17065 ),
 ( #12077, #24592, #32643 ),
 ( #29802, #7053, #14888 ),
 ( #27463, #13213, #28267 ),
 ( #32980, #31140, #10547 ),
 ( #25947, #519, #15745 ),
 ( #10704, #5213, #2553 ),
 ( #12720, #10048, #373 ),
 ( #20262, #23413, #12568 ),
 ( #20920, #15390, #5374 ),
 ( #20758, #5709, #2707 ),
 ( #22922, #30, #30814 ),
 ( #22774, #10215, #20437 ),
 ( #8225, #30656, #30958 ),
 ( #15562, #8040, #7733 ),
 ( #25779, #18074, #13069 ),
 ( #17925, #18425, #12882 ),
 ( #2906, #28615, #30461 ),
 ( #25598, #15889, #23101 ),
 ( #27958, #26099, #28116 ),
 ( #7543, #18238, #28451 ),
 ( #5563, #20607, #17748 ),
 ( #23270, #5062, #3057 ),
 ( #222, #15239, #10398 ),
 ( #25442, #7882, #16230 ),
 ( #13364, #23577, #16035 ),
 ( #29107, #9007, #31788 ),
 ( #5852, #26447, #3860 ),
 ( #8859, #3203, #1184 ),
 ( #31942, #11382, #6196 ),
 ( #8373, #19068, #26588 ),
 ( #13548, #869, #6341 ),
 ( #3545, #18569, #701 ) ),
 .UNSPECIFIED., .F., .F., .F. ) 
 B_SPLINE_SURFACE_WITH_KNOTS ( ( 4, 2, 2, 2, 2, 2, 2, 2, 2, 2, 2, 2, 2, 2, 2, 2, 4 ),
 ( 3, 3 ),
 ( 0.000000000000000000, 0.004360647101759708780, 0.005450808877199635541, 0.006540970652639563170, 0.008721294203519417559, 0.009811455978959344321, 0.01090161775439927108, 0.01199177952983919784, 0.01308194130527912634, 0.01526226485615898160, 0.01635242663159890836, 0.01744258840703883512, 0.02180323550879854216, 0.02398355905967839569, 0.02616388261055825268, 0.03052452971231796319, 0.03488517681407767024 ),
 ( 0.000000000000000000, 1.000000000000000000 ),
 .UNSPECIFIED. ) 
 GEOMETRIC_REPRESENTATION_ITEM ( )  RATIONAL_B_SPLINE_SURFACE ( (
 ( 1.000000000000000000, 0.8508761217583463710, 1.000000000000000000),
 ( 1.000000000000000000, 0.8513495319938002570, 1.000000000000000000),
 ( 1.000000000000000000, 0.8517269884644930178, 1.000000000000000000),
 ( 1.000000000000000000, 0.8525421454182948722, 1.000000000000000000),
 ( 1.000000000000000000, 0.8526809326693643998, 1.000000000000000000),
 ( 1.000000000000000000, 0.8529405002960604998, 1.000000000000000000),
 ( 1.000000000000000000, 0.8530607137251564609, 1.000000000000000000),
 ( 1.000000000000000000, 0.8534148190580183035, 1.000000000000000000),
 ( 1.000000000000000000, 0.8536546399906833615, 1.000000000000000000),
 ( 1.000000000000000000, 0.8539619561405888959, 1.000000000000000000),
 ( 1.000000000000000000, 0.8540316006964270290, 1.000000000000000000),
 ( 1.000000000000000000, 0.8540602160990389269, 1.000000000000000000),
 ( 1.000000000000000000, 0.8540396656596365155, 1.000000000000000000),
 ( 1.000000000000000000, 0.8539811480365533392, 1.000000000000000000),
 ( 1.000000000000000000, 0.8539432201616324880, 1.000000000000000000),
 ( 1.000000000000000000, 0.8538670549725509984, 1.000000000000000000),
 ( 1.000000000000000000, 0.8538286323939511258, 1.000000000000000000),
 ( 1.000000000000000000, 0.8536850005030293120, 1.000000000000000000),
 ( 1.000000000000000000, 0.8533603115986116983, 1.000000000000000000),
 ( 1.000000000000000000, 0.8529655131887596831, 1.000000000000000000),
 ( 1.000000000000000000, 0.8528244803202271740, 1.000000000000000000),
 ( 1.000000000000000000, 0.8525300428278739240, 1.000000000000000000),
 ( 1.000000000000000000, 0.8523762152465480524, 1.000000000000000000),
 ( 1.000000000000000000, 0.8516129968056589394, 1.000000000000000000),
 ( 1.000000000000000000, 0.8513036313371858954, 1.000000000000000000),
 ( 1.000000000000000000, 0.8508287765237684264, 1.000000000000000000),
 ( 1.000000000000000000, 0.8506601442286274573, 1.000000000000000000),
 ( 1.000000000000000000, 0.8503078737455993519, 1.000000000000000000),
 ( 1.000000000000000000, 0.8501262971080763009, 1.000000000000000000),
 ( 1.000000000000000000, 0.8496349502455389224, 1.000000000000000000),
 ( 1.000000000000000000, 0.8494863746679542915, 1.000000000000000000),
 ( 1.000000000000000000, 0.8492518789947639535, 1.000000000000000000),
 ( 1.000000000000000000, 0.8491664934843269341, 1.000000000000000000),
 ( 1.000000000000000000, 0.8490876263417839187, 1.000000000000000000) ) ) 
 REPRESENTATION_ITEM ( '' )  SURFACE ( )  );
#15562 = CARTESIAN_POINT ( 'NONE',  ( -2.454858791982045041, -12.18258820806518372, 1.743819948486679206 ) ) ;
#15563 = CARTESIAN_POINT ( 'NONE',  ( 23.48500000136559862, 2.892927487894327410, -1.570731468192931635 ) ) ;
#15564 = CIRCLE ( 'NONE', #18764, 10.99999999999999822 ) ;
#15565 = DIRECTION ( 'NONE',  ( -0.000000000000000000, -0.000000000000000000, -1.000000000000000000 ) ) ;
#15567 = EDGE_LOOP ( 'NONE', ( #20552, #3762, #21291, #14611, #31850, #11541, #14141, #321, #3711, #7339, #9503, #26046, #27804, #17988, #28783, #20008, #1065, #403, #23190, #11222, #17624, #32123, #20786, #14289, #29998, #1407, #24962, #5706, #7991, #11526, #6752, #29633, #21652, #26816, #29904, #19250, #11158, #20243, #9621, #19248, #27365, #12515, #18784, #14226, #31448, #14790, #33, #26676, #5096, #737, #19796, #28321, #30818, #24391, #18272, #13801, #26745 ) ) ;
#15566 = CARTESIAN_POINT ( 'NONE',  ( -23.35000000000000142, -10.96966150227469505, 4.000000000000000000 ) ) ;
#15568 = DIRECTION ( 'NONE',  ( -1.000000000000000000, 0.000000000000000000, -0.000000000000000000 ) ) ;
#15569 = VECTOR ( 'NONE', #2072, 1000.000000000000000 ) ;
#15570 = EDGE_CURVE ( 'NONE', #8422, #9245, #15998, .T. ) ;
#15571 = AXIS2_PLACEMENT_3D ( 'NONE', #27061, #31429, #26430 ) ;
#15572 = CC_DESIGN_PERSON_AND_ORGANIZATION_ASSIGNMENT ( #2378, #30634, ( #4466 ) ) ;
#15573 = CARTESIAN_POINT ( 'NONE',  ( -26.39604612056346511, 17.76592253751580586, 1.789727549128061757 ) ) ;
#15574 = CARTESIAN_POINT ( 'NONE',  ( 25.48500000273118715, 0.2613211581691317065, 2.486304738420681559 ) ) ;
#15575 = CARTESIAN_POINT ( 'NONE',  ( 7.249760686538667009, 0.000000000000000000, 0.000000000000000000 ) ) ;
#15576 = DIRECTION ( 'NONE',  ( 0.000000000000000000, 0.000000000000000000, -1.000000000000000000 ) ) ;
#15577 = CARTESIAN_POINT ( 'NONE',  ( -56.27770248097862549, 0.4996615022747108448, 1.500000000000000000 ) ) ;
#15578 = VERTEX_POINT ( 'NONE', #3336 ) ;
#15579 = CARTESIAN_POINT ( 'NONE',  ( 108.0281774240363717, -18.47511001308152601, 4.365040738911419638 ) ) ;
#15580 = VECTOR ( 'NONE', #13784, 1000.000000000000000 ) ;
#15581 = FACE_OUTER_BOUND ( 'NONE', #30972, .T. ) ;
#15582 = ORIENTED_EDGE ( 'NONE', *, *, #14747, .F. ) ;
#15583 = EDGE_CURVE ( 'NONE', #2205, #15872, #22221, .T. ) ;
#15584 = AXIS2_PLACEMENT_3D ( 'NONE', #25528, #10323, #5146 ) ;
#15585 = AXIS2_PLACEMENT_3D ( 'NONE', #18082, #2717, #28461 ) ;
#15586 = AXIS2_PLACEMENT_3D ( 'NONE', #9506, #30117, #26926 ) ;
#15587 = DIRECTION ( 'NONE',  ( 0.000000000000000000, 0.2588190451025358940, -0.9659258262890643154 ) ) ;
#15588 = EDGE_CURVE ( 'NONE', #32584, #5774, #31569, .T. ) ;
#15589 = DIRECTION ( 'NONE',  ( 8.574039729943018344E-17, 1.000000000000000000, 0.000000000000000000 ) ) ;
#15590 = CARTESIAN_POINT ( 'NONE',  ( -1.033057378353439804, -8.048844657541355474, -4.522129901861164925 ) ) ;
#15593 = CARTESIAN_POINT ( 'NONE',  ( 107.9808062360839216, -17.79297669103587154, 4.347487705976786465 ) ) ;
#15592 = CARTESIAN_POINT ( 'NONE',  ( 10.00000000000000000, 4.923251879855578162E-14, -4.753758587302147731 ) ) ;
#15591 = AXIS2_PLACEMENT_3D ( 'NONE', #3877, #29623, #21749 ) ;
#15594 = VERTEX_POINT ( 'NONE', #833 ) ;
#15595 = VECTOR ( 'NONE', #32676, 1000.000000000000114 ) ;
#15596 = CIRCLE ( 'NONE', #17192, 298.4532556727467636 ) ;
#15597 = CARTESIAN_POINT ( 'NONE',  ( -41.86373177837820236, -16.13513036599589867, 5.128141679950118714 ) ) ;
#15598 = ORIENTED_EDGE ( 'NONE', *, *, #28515, .F. ) ;
#15599 = CARTESIAN_POINT ( 'NONE',  ( -3.018833153847216622, -0.05660549560302519101, 1.240144350321864763 ) ) ;
#15601 = ORIENTED_EDGE ( 'NONE', *, *, #32175, .F. ) ;
#15600 = DIRECTION ( 'NONE',  ( -1.000000000000000000, 0.000000000000000000, 0.000000000000000000 ) ) ;
#15602 = ORIENTED_EDGE ( 'NONE', *, *, #6548, .T. ) ;
#15603 = CARTESIAN_POINT ( 'NONE',  ( 10.00000000000000000, 1.476463073999702225, -4.787500056513350977 ) ) ;
#15604 = CARTESIAN_POINT ( 'NONE',  ( 6.037141869538512395, -7.104659103919376939, 4.619542287584878615 ) ) ;
#15606 = ORIENTED_EDGE ( 'NONE', *, *, #7611, .T. ) ;
#15605 = DIRECTION ( 'NONE',  ( -0.8896831085035101783, 0.4565785435645562940, 0.000000000000000000 ) ) ;
#15607 = AXIS2_PLACEMENT_3D ( 'NONE', #15763, #3076, #13231 ) ;
#15608 = ORIENTED_EDGE ( 'NONE', *, *, #19625, .T. ) ;
#15609 = CARTESIAN_POINT ( 'NONE',  ( 11.95049951519663978, -15.52103481658239659, -1.754067188414264233 ) ) ;
#15610 = AXIS2_PLACEMENT_3D ( 'NONE', #1247, #11435, #21630 ) ;
#15611 = DIRECTION ( 'NONE',  ( 1.000000000000000000, 0.000000000000000000, 0.000000000000000000 ) ) ;
#15612 = CARTESIAN_POINT ( 'NONE',  ( 108.1300413742128228, -19.95926608421481063, -1.392287898180229133 ) ) ;
#15613 = CARTESIAN_POINT ( 'NONE',  ( -3.356376981307136464, -0.1572233378491262878, 2.999999999999999556 ) ) ;
#15614 = DIRECTION ( 'NONE',  ( 0.03488359650710500665, -0.9989355049964836475, -0.03018263660036204013 ) ) ;
#15615 = AXIS2_PLACEMENT_3D ( 'NONE', #22266, #32477, #30149 ) ;
#15616 = CIRCLE ( 'NONE', #683, 8.500000000000000000 ) ;
#15617 = AXIS2_PLACEMENT_3D ( 'NONE', #25872, #2992, #4795 ) ;
#15618 = CIRCLE ( 'NONE', #144, 0.5000000000000004441 ) ;
#15619 = CARTESIAN_POINT ( 'NONE',  ( 0.9499999999999995115, 0.000000000000000000, 0.000000000000000000 ) ) ;
#15620 = CARTESIAN_POINT ( 'NONE',  ( 1.134906995224885584, -9.027104445734691396, 1.499999999999999334 ) ) ;
#15621 = CARTESIAN_POINT ( 'NONE',  ( 41.35536016469701082, -7.892720495295837857, 2.184957211607506000 ) ) ;
#15622 = CIRCLE ( 'NONE', #6543, 8.500000000000000000 ) ;
#15623 = AXIS2_PLACEMENT_3D ( 'NONE', #19397, #2001, #9662 ) ;
#15624 = DIRECTION ( 'NONE',  ( 0.000000000000000000, -1.000000000000000000, 0.000000000000000000 ) ) ;
#15625 = DIRECTION ( 'NONE',  ( 1.000000000000000000, -0.000000000000000000, -0.000000000000000000 ) ) ;
#15626 = DIRECTION ( 'NONE',  ( -0.000000000000000000, -0.000000000000000000, 1.000000000000000000 ) ) ;
#15627 = CARTESIAN_POINT ( 'NONE',  ( 48.05280571049737404, -6.817569152029394175, 5.695980980372492120 ) ) ;
#15628 = EDGE_CURVE ( 'NONE', #974, #20282, #26289, .T. ) ;
#15629 = CARTESIAN_POINT ( 'NONE',  ( 13.58267262069031922, 21.92668125727452733, -1.161744080134329726 ) ) ;
#15630 = VERTEX_POINT ( 'NONE', #5987 ) ;
#15631 = ADVANCED_FACE ( 'NONE', ( #3813 ), #11010, .F. ) ;
#15632 = CARTESIAN_POINT ( 'NONE',  ( -4.787550801365593856, 3.521866450007987037, 0.3701630799359328372 ) ) ;
#15633 = CIRCLE ( 'NONE', #675, 2.999999999999999112 ) ;
#15634 = VECTOR ( 'NONE', #17546, 1000.000000000000000 ) ;
#15635 = CARTESIAN_POINT ( 'NONE',  ( 25.27346073696792672, -0.6948329026079288484, 2.447823836836187539 ) ) ;
#15636 = CARTESIAN_POINT ( 'NONE',  ( 0.000000000000000000, -7.673322273190749776, 3.656518192455051608 ) ) ;
#15638 = EDGE_LOOP ( 'NONE', ( #14477, #10468, #8847, #10326 ) ) ;
#15637 = AXIS2_PLACEMENT_3D ( 'NONE', #20981, #10947, #20809 ) ;
#15639 = CARTESIAN_POINT ( 'NONE',  ( 47.98568197278775216, -2.821418575600922019, -0.07017451552781628354 ) ) ;
#15640 =( NAMED_UNIT ( * ) SI_UNIT ( $, .STERADIAN. ) SOLID_ANGLE_UNIT ( ) );
#15641 = CONICAL_SURFACE ( 'NONE', #6017, 5.999999999999999112, 0.08726646259971666819 ) ;
#15642 = AXIS2_PLACEMENT_3D ( 'NONE', #13377, #25963, #3217 ) ;
#15643 = VERTEX_POINT ( 'NONE', #21211 ) ;
#15644 = CARTESIAN_POINT ( 'NONE',  ( 29.41391112839824373, -2.700987858903443950, -0.07017451552781585333 ) ) ;
#15645 = PERSON_AND_ORGANIZATION_ROLE ( 'classification_officer' ) ;
#15647 = ORIENTED_EDGE ( 'NONE', *, *, #9943, .F. ) ;
#15646 = CARTESIAN_POINT ( 'NONE',  ( 110.4915906369627123, -18.78144465615449832, -4.522129901861166701 ) ) ;
#15648 = ORIENTED_EDGE ( 'NONE', *, *, #22134, .T. ) ;
#15649 = CARTESIAN_POINT ( 'NONE',  ( -2.767073886773233848, -0.6621507858625358400, 1.748408842879327851 ) ) ;
#15650 = AXIS2_PLACEMENT_3D ( 'NONE', #29321, #21649, #9078 ) ;
#15651 = ORIENTED_EDGE ( 'NONE', *, *, #20020, .F. ) ;
#15652 = CARTESIAN_POINT ( 'NONE',  ( 25.76000000000000512, 0.9093756521784821523, 2.891331917153146858 ) ) ;
#15654 = ORIENTED_EDGE ( 'NONE', *, *, #4999, .T. ) ;
#15653 = CARTESIAN_POINT ( 'NONE',  ( -2.459135176628032049, 0.1657091670264760619, 3.101200306062372292 ) ) ;
#15655 = CARTESIAN_POINT ( 'NONE',  ( 18.53796472816966912, -8.341849780241114232, 1.915219082070893863 ) ) ;
#15656 = CARTESIAN_POINT ( 'NONE',  ( 108.1072762316657219, -19.61411316563674134, 2.020652039824201829 ) ) ;
#15657 = DIRECTION ( 'NONE',  ( -0.000000000000000000, -0.000000000000000000, -1.000000000000000000 ) ) ;
#15658 = DIRECTION ( 'NONE',  ( -0.000000000000000000, -1.000000000000000000, -0.000000000000000000 ) ) ;
#15659 = ORIENTED_EDGE ( 'NONE', *, *, #25283, .T. ) ;
#15660 = AXIS2_PLACEMENT_3D ( 'NONE', #8822, #19027, #29213 ) ;
#15661 = AXIS2_PLACEMENT_3D ( 'NONE', #8153, #3004, #18360 ) ;
#15662 = DIRECTION ( 'NONE',  ( -0.1027947991993877763, 0.9947025833170223263, 0.000000000000000000 ) ) ;
#15663 = CARTESIAN_POINT ( 'NONE',  ( 4.749760686538667009, 8.385837730238846314E-14, -8.014274990069656823 ) ) ;
#15664 = DIRECTION ( 'NONE',  ( 0.1767573132311699713, 0.9842544651762054064, 0.000000000000000000 ) ) ;
#15665 = CARTESIAN_POINT ( 'NONE',  ( 4.749760686538667009, 1.391664247347333294, -7.892520144992419162 ) ) ;
#15666 = AXIS2_PLACEMENT_3D ( 'NONE', #24837, #32536, #14638 ) ;
#15667 = TOROIDAL_SURFACE ( 'NONE', #14044, 10.51776515689528502, 0.5000000000000000000 ) ;
#15668 = AXIS2_PLACEMENT_3D ( 'NONE', #22248, #2180, #29934 ) ;
#15669 = EDGE_CURVE ( 'NONE', #26254, #29588, #58, .T. ) ;
#15670 = CARTESIAN_POINT ( 'NONE',  ( 24.62503378732304071, -17.47108153024710475, 1.492984249781206474 ) ) ;
#15671 = CARTESIAN_POINT ( 'NONE',  ( 10.00000000000000000, -0.6226916219172395905, 4.971152295393299170 ) ) ;
#15672 = CARTESIAN_POINT ( 'NONE',  ( 22.55656763645045615, -0.8852964313267484009, 2.499999999999997780 ) ) ;
#15673 = FACE_OUTER_BOUND ( 'NONE', #3107, .T. ) ;
#15674 = VERTEX_POINT ( 'NONE', #18684 ) ;
#15675 = AXIS2_PLACEMENT_3D ( 'NONE', #20744, #23560, #18901 ) ;
#15676 = LOCAL_TIME ( 16, 7, 10.00000000000000000, #8844 ) ;
#15677 = CARTESIAN_POINT ( 'NONE',  ( -2.512550801365593056, -1.088641768524163389, -3.675193018007246071 ) ) ;
#15678 = EDGE_LOOP ( 'NONE', ( #29228, #12258, #9641, #32229 ) ) ;
#15679 = CARTESIAN_POINT ( 'NONE',  ( -2.954531657079157547, -0.9198621039125872700, -3.105402419394638791 ) ) ;
#15680 = EDGE_CURVE ( 'NONE', #10104, #1079, #5474, .T. ) ;
#15681 = LINE ( 'NONE', #3003, #5010 ) ;
#15682 = CARTESIAN_POINT ( 'NONE',  ( 3.249999999999999556, 9.314797388894893615, 1.239665997526919972 ) ) ;
#15683 = CARTESIAN_POINT ( 'NONE',  ( 9.126991456845855666, -11.32614230912692577, 1.000000000000000000 ) ) ;
#15684 = VERTEX_POINT ( 'NONE', #31751 ) ;
#15685 = CYLINDRICAL_SURFACE ( 'NONE', #25240, 2.999999999999999112 ) ;
#15686 = CIRCLE ( 'NONE', #5559, 9.713116299512234875 ) ;
#15687 = ORIENTED_EDGE ( 'NONE', *, *, #7313, .T. ) ;
#15688 = CARTESIAN_POINT ( 'NONE',  ( 19.03654924710325602, -2.768675503676416572, -2.713652344655543391 ) ) ;
#15689 = PERSON_AND_ORGANIZATION ( #6766, #25292 ) ;
#15690 = ADVANCED_FACE ( 'NONE', ( #6304 ), #11500, .T. ) ;
#15691 = CARTESIAN_POINT ( 'NONE',  ( 18.76345385348679429, -5.821333909315332455, 4.073741754928252412 ) ) ;
#15692 = VECTOR ( 'NONE', #10285, 1000.000000000000114 ) ;
#15693 = TOROIDAL_SURFACE ( 'NONE', #27963, 300.0401151713995773, 0.7999999999999787281 ) ;
#15694 = CARTESIAN_POINT ( 'NONE',  ( 2.342933509396897929, -0.1895978275999547213, -1.757325986342923363 ) ) ;
#15696 = CARTESIAN_POINT ( 'NONE',  ( 6.356382477965130562, 6.947086032709933967, 5.080803740829747284 ) ) ;
#15695 = CARTESIAN_POINT ( 'NONE',  ( 24.80306213860490061, -17.49230408913781787, -1.500000000000000000 ) ) ;
#15697 = VERTEX_POINT ( 'NONE', #26552 ) ;
#15698 = EDGE_CURVE ( 'NONE', #30416, #3718, #18205, .T. ) ;
#15699 = LOCAL_TIME ( 16, 7, 10.00000000000000000, #29057 ) ;
#15700 = FACE_OUTER_BOUND ( 'NONE', #5288, .T. ) ;
#15701 = CARTESIAN_POINT ( 'NONE',  ( 2.382865613620175349, 0.000000000000000000, -1.491740999229418829 ) ) ;
#15702 = DIRECTION ( 'NONE',  ( -1.000000000000000000, 0.000000000000000000, 0.000000000000000000 ) ) ;
#15704 = EDGE_LOOP ( 'NONE', ( #15183, #19761, #15598, #19389 ) ) ;
#15703 = CARTESIAN_POINT ( 'NONE',  ( 24.35832023931450507, -17.33818253687174860, -1.317734466820339900 ) ) ;
#15705 = CARTESIAN_POINT ( 'NONE',  ( -5.562550801365593323, 2.752080473201636845, -2.228590825266444142 ) ) ;
#15706 = EDGE_CURVE ( 'NONE', #11079, #15980, #9739, .T. ) ;
#15707 = CARTESIAN_POINT ( 'NONE',  ( -53.96180052795275373, 5.510921350264005092, 1.087562001069957152 ) ) ;
#15708 = CARTESIAN_POINT ( 'NONE',  ( 85.05927807847527333, -5.579234875939544480, -3.390607678631389010 ) ) ;
#15709 = ORIENTED_EDGE ( 'NONE', *, *, #30660, .F. ) ;
#15710 = ORIENTED_EDGE ( 'NONE', *, *, #24873, .F. ) ;
#15711 = CIRCLE ( 'NONE', #27449, 0.9999999999999983347 ) ;
#15712 = DIRECTION ( 'NONE',  ( 0.000000000000000000, 1.000000000000000000, 0.000000000000000000 ) ) ;
#15713 = CARTESIAN_POINT ( 'NONE',  ( -31.86948564418014485, -21.73221622336745895, -1.500000000000000000 ) ) ;
#15714 = EDGE_CURVE ( 'NONE', #13391, #7656, #4413, .T. ) ;
#15715 = EDGE_CURVE ( 'NONE', #4235, #13159, #27542, .T. ) ;
#15716 = CARTESIAN_POINT ( 'NONE',  ( 22.04750000136559507, -1.913930629741527500, 2.363507492473149618 ) ) ;
#15717 = CARTESIAN_POINT ( 'NONE',  ( 0.7632845268398879002, -8.152713396088778097, 3.174628368996039729 ) ) ;
#15718 = CARTESIAN_POINT ( 'NONE',  ( 68.56906952848774495, -3.255983411058744004, -0.07017451552781628354 ) ) ;
#15719 = DIRECTION ( 'NONE',  ( -1.000000000000000000, 0.000000000000000000, -0.000000000000000000 ) ) ;
#15720 = CARTESIAN_POINT ( 'NONE',  ( 8.901867736793459329, 0.07845480144339982143, 1.317219896051721406 ) ) ;
#15721 = CARTESIAN_POINT ( 'NONE',  ( 29.18336473368350070, -8.306880066003914820, 0.07017451552781851787 ) ) ;
#15722 = ORIENTED_EDGE ( 'NONE', *, *, #29662, .F. ) ;
#15723 = CARTESIAN_POINT ( 'NONE',  ( 7.249760686538667009, 0.000000000000000000, 0.000000000000000000 ) ) ;
#15724 = CALENDAR_DATE ( 2026, 6, 10 ) ;
#15725 = DIRECTION ( 'NONE',  ( 0.2880220749472559572, 0.1662896225033555220, -0.9430753128943462071 ) ) ;
#15726 = EDGE_LOOP ( 'NONE', ( #11563, #25852, #26244 ) ) ;
#15727 = EDGE_CURVE ( 'NONE', #32925, #23049, #14310, .T. ) ;
#15728 = AXIS2_PLACEMENT_3D ( 'NONE', #18832, #29032, #13941 ) ;
#15729 = CARTESIAN_POINT ( 'NONE',  ( -31.85000000000000497, -10.96966150227469505, 1.500000000000000000 ) ) ;
#15730 = ORIENTED_EDGE ( 'NONE', *, *, #15179, .T. ) ;
#15731 = CARTESIAN_POINT ( 'NONE',  ( -5.350050802731187716, 0.3135853898029611342, -2.983565686104819648 ) ) ;
#15733 = ORIENTED_EDGE ( 'NONE', *, *, #24002, .T. ) ;
#15732 = CARTESIAN_POINT ( 'NONE',  ( 84.96912909400775504, -4.116878033481301102, -4.073740955716186996 ) ) ;
#15734 = EDGE_LOOP ( 'NONE', ( #12603, #7945, #6207, #28594 ) ) ;
#15735 = CARTESIAN_POINT ( 'NONE',  ( -17.45597128428592981, -25.93932300454937945, 11.50000000000000000 ) ) ;
#15736 = LINE ( 'NONE', #12713, #25684 ) ;
#15737 = DIRECTION ( 'NONE',  ( -8.281886410780512259E-17, -0.9659258262890680902, -0.2588190451025216277 ) ) ;
#15738 = B_SPLINE_CURVE_WITH_KNOTS ( 'NONE', 3,
 ( #31898, #26548, #21540, #16662, #4295, #1625, #9309, #13978, #8965, #19356 ),
 .UNSPECIFIED., .F., .F.,
 ( 4, 3, 3, 4 ),
 ( 0.000000000000000000, 0.0005352572989639539907, 0.001070514597927907331, 0.002130599681840938692 ),
 .UNSPECIFIED. ) ;
#15739 = CARTESIAN_POINT ( 'NONE',  ( 18.51491971917342028, -8.599446730134173933, -0.07017451552783579571 ) ) ;
#15741 = ORIENTED_EDGE ( 'NONE', *, *, #23544, .F. ) ;
#15740 = DIRECTION ( 'NONE',  ( -0.000000000000000000, 0.000000000000000000, 1.000000000000000000 ) ) ;
#15742 = CARTESIAN_POINT ( 'NONE',  ( 10.00000000000000000, 3.641590349731970822, -3.055657119358763829 ) ) ;
#15743 = CARTESIAN_POINT ( 'NONE',  ( 13.32340444471394569, 6.787188996462521828, 1.050000000000000044 ) ) ;
#15744 = AXIS2_PLACEMENT_3D ( 'NONE', #24043, #28433, #23891 ) ;
#15745 = CARTESIAN_POINT ( 'NONE',  ( -4.555723071052306672, -6.510850216547120262, 1.499999999999999556 ) ) ;
#15746 = CARTESIAN_POINT ( 'NONE',  ( 21.79750000136559507, 0.3178988483021036315, 3.024605502323848949 ) ) ;
#15747 = CARTESIAN_POINT ( 'NONE',  ( 3.286352104298968069, -0.1045966074583460498, 1.312070483712308500 ) ) ;
#15748 = ADVANCED_FACE ( 'NONE', ( #24692 ), #14480, .T. ) ;
#15750 = VERTEX_POINT ( 'NONE', #27377 ) ;
#15749 = CARTESIAN_POINT ( 'NONE',  ( 3.063284526839887167, -3.174628368996133432, 8.152713396088751452 ) ) ;
#15751 = LINE ( 'NONE', #28121, #1306 ) ;
#15752 = CARTESIAN_POINT ( 'NONE',  ( -28.19744467622691175, 16.39278089773672420, 1.823048619078819765 ) ) ;
#15753 = CARTESIAN_POINT ( 'NONE',  ( 22.48500000136559507, 2.892927487894327410, -1.570731468192931635 ) ) ;
#15754 = EDGE_CURVE ( 'NONE', #2105, #27641, #12002, .T. ) ;
#15755 = EDGE_CURVE ( 'NONE', #24602, #25095, #1206, .T. ) ;
#15756 = CARTESIAN_POINT ( 'NONE',  ( 10.00000000000000000, 4.467071865485470639, 1.625881193364712596 ) ) ;
#15757 = CARTESIAN_POINT ( 'NONE',  ( 7.249760686538667009, 8.721381771256204729, -0.7071067811865423547 ) ) ;
#15758 = CARTESIAN_POINT ( 'NONE',  ( -2.863349216192390578, 0.2791979387067957119, -0.7890172491793835396 ) ) ;
#15759 = ORIENTED_EDGE ( 'NONE', *, *, #618, .T. ) ;
#15760 = CARTESIAN_POINT ( 'NONE',  ( -1.082681991931091270, 0.000000000000000000, 4.629213727441584325 ) ) ;
#15761 = CARTESIAN_POINT ( 'NONE',  ( 4.749760686538667009, -2.789499415801756586E-14, 8.014274990069656823 ) ) ;
#15762 = ORIENTED_EDGE ( 'NONE', *, *, #27506, .T. ) ;
#15763 = CARTESIAN_POINT ( 'NONE',  ( 0.000000000000000000, 1.239665997526887109, 9.314797388894895391 ) ) ;
#15764 = CARTESIAN_POINT ( 'NONE',  ( 107.6300413742128228, -19.95926608421483195, 0.000000000000000000 ) ) ;
#15765 = CARTESIAN_POINT ( 'NONE',  ( 12.65465643788354200, -15.70291107026620914, -1.500000000000000444 ) ) ;
#15767 = CARTESIAN_POINT ( 'NONE',  ( 107.9748542853220954, -17.70727008077477649, 5.017937325796186343 ) ) ;
#15766 = CARTESIAN_POINT ( 'NONE',  ( -5.750050799999999462, 0.000000000000000000, 0.000000000000000000 ) ) ;
#15768 = EDGE_LOOP ( 'NONE', ( #14617, #18944, #27098, #20523 ) ) ;
#15769 = EDGE_CURVE ( 'NONE', #26082, #16537, #21057, .T. ) ;
#15770 = CC_DESIGN_PERSON_AND_ORGANIZATION_ASSIGNMENT ( #32391, #3792, ( #32741 ) ) ;
#15771 = CARTESIAN_POINT ( 'NONE',  ( -34.30400690026458221, 19.51744974835125035, 2.412380016372531522 ) ) ;
#15772 = ORIENTED_EDGE ( 'NONE', *, *, #28151, .F. ) ;
#15773 =( BOUNDED_CURVE ( )  B_SPLINE_CURVE ( 3, ( #27283, #4400, #19458, #1723 ),
 .UNSPECIFIED., .F., .F. ) 
 B_SPLINE_CURVE_WITH_KNOTS ( ( 4, 4 ),
 ( 3.141592653589793560, 4.712388980384691450 ),
 .UNSPECIFIED. ) 
 CURVE ( )  GEOMETRIC_REPRESENTATION_ITEM ( )  RATIONAL_B_SPLINE_CURVE ( ( 1.000000000000000000, 0.8047378541243646044, 0.8047378541243646044, 1.000000000000000000 ) ) 
 REPRESENTATION_ITEM ( '' )  );
#15774 = DIRECTION ( 'NONE',  ( -1.000000000000000000, 2.473959037481237219E-13, 0.000000000000000000 ) ) ;
#15776 = ORIENTED_EDGE ( 'NONE', *, *, #19136, .T. ) ;
#15775 = CARTESIAN_POINT ( 'NONE',  ( 107.3476768466458253, -15.88628154573095586, -1.500000000000000000 ) ) ;
#15777 = ORIENTED_EDGE ( 'NONE', *, *, #17978, .T. ) ;
#15778 = CARTESIAN_POINT ( 'NONE',  ( 25.75999999999999801, -2.208672634433321348E-15, 0.000000000000000000 ) ) ;
#15779 = PLANE ( 'NONE',  #12362 ) ;
#15781 = VERTEX_POINT ( 'NONE', #19856 ) ;
#15780 = CARTESIAN_POINT ( 'NONE',  ( -2.523601663466349176, 0.4696231843230803671, -1.500000000000000000 ) ) ;
#15782 = ORIENTED_EDGE ( 'NONE', *, *, #12617, .F. ) ;
#15783 = CARTESIAN_POINT ( 'NONE',  ( 15.81158201665590290, -16.37188494488893298, -1.753542180525299532 ) ) ;
#15784 = CARTESIAN_POINT ( 'NONE',  ( 0.000000000000000000, -7.593217523260636703, 7.958834565716742304 ) ) ;
#15785 = LINE ( 'NONE', #3097, #4808 ) ;
#15786 = CARTESIAN_POINT ( 'NONE',  ( 19.03654924710324892, -2.768675503676413019, -2.713652344655541615 ) ) ;
#15787 = EDGE_CURVE ( 'NONE', #12441, #14119, #19685, .T. ) ;
#15788 = CARTESIAN_POINT ( 'NONE',  ( -6.906376978575949899, 0.1572233378491243172, -2.999999999999999556 ) ) ;
#15789 = CARTESIAN_POINT ( 'NONE',  ( 10.57125986779756843, 0.8254815157535864145, -4.681538312723508177 ) ) ;
#15790 = DIRECTION ( 'NONE',  ( -7.770718973609018100E-17, -0.9063077870366551547, 0.4226182617406882835 ) ) ;
#15791 = CARTESIAN_POINT ( 'NONE',  ( 107.4500593345376558, -17.36019228850485163, -4.522129901861164925 ) ) ;
#15792 = CARTESIAN_POINT ( 'NONE',  ( -7.000050800000001239, 0.000000000000000000, 0.000000000000000000 ) ) ;
#15793 = ORIENTED_EDGE ( 'NONE', *, *, #27611, .F. ) ;
#15794 = DIRECTION ( 'NONE',  ( 0.000000000000000000, 0.000000000000000000, -1.000000000000000000 ) ) ;
#15795 = CARTESIAN_POINT ( 'NONE',  ( 5.612718383992090665, -8.123482740191962037, -1.229942497144119296 ) ) ;
#15796 = FACE_OUTER_BOUND ( 'NONE', #27527, .T. ) ;
#15797 = ORIENTED_EDGE ( 'NONE', *, *, #31668, .F. ) ;
#15798 = CARTESIAN_POINT ( 'NONE',  ( -2.550050802731187005, -0.3135853898029607456, 2.983565686104819648 ) ) ;
#15799 = CARTESIAN_POINT ( 'NONE',  ( 18.06874303396881132, -21.14907373874090979, -1.751201621421682120 ) ) ;
#15800 = ORIENTED_EDGE ( 'NONE', *, *, #31917, .F. ) ;
#15801 = LINE ( 'NONE', #25500, #6908 ) ;
#15802 = ADVANCED_FACE ( 'NONE', ( #16993 ), #25014, .T. ) ;
#15803 = ORIENTED_EDGE ( 'NONE', *, *, #3773, .F. ) ;
#15804 = CARTESIAN_POINT ( 'NONE',  ( 23.95058674323864523, -2.449331254355788356, -1.010822989962086416 ) ) ;
#15805 = CALENDAR_DATE ( 2026, 6, 10 ) ;
#15807 = ORIENTED_EDGE ( 'NONE', *, *, #19612, .T. ) ;
#15806 = CARTESIAN_POINT ( 'NONE',  ( -3.827997810773342557, -10.69410007036992560, -0.9788672205760856615 ) ) ;
#15808 = ORIENTED_EDGE ( 'NONE', *, *, #13616, .F. ) ;
#15809 = FACE_OUTER_BOUND ( 'NONE', #16472, .T. ) ;
#15810 = ORIENTED_EDGE ( 'NONE', *, *, #11205, .F. ) ;
#15811 = LINE ( 'NONE', #2793, #29953 ) ;
#15813 = ORIENTED_EDGE ( 'NONE', *, *, #26791, .F. ) ;
#15812 = CARTESIAN_POINT ( 'NONE',  ( -2.374773405519150504, 0.7814962286037724359, 3.198731613255573425 ) ) ;
#15814 = CARTESIAN_POINT ( 'NONE',  ( 85.45070076415389337, -7.158483446636730640, 2.713652344655544724 ) ) ;
#15815 = CYLINDRICAL_SURFACE ( 'NONE', #9635, 2.099999999999994316 ) ;
#15816 = EDGE_CURVE ( 'NONE', #22652, #12927, #7457, .T. ) ;
#15817 = CARTESIAN_POINT ( 'NONE',  ( -12.44989959798873791, 0.5174497483512729978, -12.99999999999999645 ) ) ;
#15818 = PLANE ( 'NONE',  #24164 ) ;
#15819 = EDGE_CURVE ( 'NONE', #26682, #10466, #29429, .T. ) ;
#15820 = VERTEX_POINT ( 'NONE', #307 ) ;
#15821 = EDGE_CURVE ( 'NONE', #293, #18598, #18730, .T. ) ;
#15822 = CARTESIAN_POINT ( 'NONE',  ( -3.712942406915326288, 4.884725290497410777E-15, -2.999999999999999556 ) ) ;
#15823 = CARTESIAN_POINT ( 'NONE',  ( -1.033057378353319677, -8.048844657541355474, -4.522129901861164925 ) ) ;
#15824 = CARTESIAN_POINT ( 'NONE',  ( 35.27668332986648636, -7.991339570346063681, -1.873789188797430727 ) ) ;
#15825 = CARTESIAN_POINT ( 'NONE',  ( 2.619288827430985567, 0.4094970184090461762, -1.491740999229418829 ) ) ;
#15826 = CARTESIAN_POINT ( 'NONE',  ( 24.59223457117506229, -17.46620485449347271, 1.489769045320403551 ) ) ;
#15827 = CARTESIAN_POINT ( 'NONE',  ( 23.07496344424409784, -21.92049039159586954, 1.202267146568063660 ) ) ;
#15828 = CARTESIAN_POINT ( 'NONE',  ( 9.350000000000001421, 0.000000000000000000, 1.500000000000000000 ) ) ;
#15829 = CARTESIAN_POINT ( 'NONE',  ( 21.31323116099372328, -21.82417724537273074, 1.319197765239640718 ) ) ;
#15830 = CARTESIAN_POINT ( 'NONE',  ( -7.650050802731187538, 2.331437884370912705, -1.887961173149511618 ) ) ;
#15831 = VERTEX_POINT ( 'NONE', #20532 ) ;
#15832 = CARTESIAN_POINT ( 'NONE',  ( -3.454531657079157103, 2.846291840500173365, 1.545410377633946952 ) ) ;
#15833 = CARTESIAN_POINT ( 'NONE',  ( 107.6764431011533816, 19.22343047903795465, 4.860991410050878869 ) ) ;
#15834 = CARTESIAN_POINT ( 'NONE',  ( -4.013969549054187630E-16, -4.681538312723522388, 0.8254815157535098091 ) ) ;
#15835 = CARTESIAN_POINT ( 'NONE',  ( 20.69346795579748388, -16.15118080677402190, 1.499999999999722444 ) ) ;
#15836 = VERTEX_POINT ( 'NONE', #5142 ) ;
#15837 = DIRECTION ( 'NONE',  ( 0.000000000000000000, 0.000000000000000000, 1.000000000000000000 ) ) ;
#15838 = ORIENTED_EDGE ( 'NONE', *, *, #15879, .F. ) ;
#15839 = CARTESIAN_POINT ( 'NONE',  ( 17.75999999999999801, -2.208672634433321348E-15, 0.000000000000000000 ) ) ;
#15840 = COORDINATED_UNIVERSAL_TIME_OFFSET ( 0, 0, .AHEAD. ) ;
#15841 = CARTESIAN_POINT ( 'NONE',  ( 102.4203624159291195, -3.957500511122341358, 4.053847705490468911 ) ) ;
#15842 = ADVANCED_FACE ( 'NONE', ( #7814 ), #32743, .F. ) ;
#15843 = CARTESIAN_POINT ( 'NONE',  ( 8.924010941014284271, 0.4014965238409368142, 1.499999999990832666 ) ) ;
#15845 = CARTESIAN_POINT ( 'NONE',  ( 6.530491627857225367, 8.330327812606292071, -2.368289848745672277 ) ) ;
#15844 = DIRECTION ( 'NONE',  ( 0.000000000000000000, 0.000000000000000000, 1.000000000000000000 ) ) ;
#15846 = ORIENTED_EDGE ( 'NONE', *, *, #21738, .F. ) ;
#15847 = DIRECTION ( 'NONE',  ( 1.000000000000000000, -0.000000000000000000, -0.000000000000000000 ) ) ;
#15848 = DIRECTION ( 'NONE',  ( 1.000000000000000000, -0.000000000000000000, -0.000000000000000000 ) ) ;
#15849 = CARTESIAN_POINT ( 'NONE',  ( 22.17250000136559507, -3.024605502323851169, 0.3178988483021052969 ) ) ;
#15851 = ORIENTED_EDGE ( 'NONE', *, *, #1519, .T. ) ;
#15850 = DIRECTION ( 'NONE',  ( 1.000000000000000000, -0.000000000000000000, -0.000000000000000000 ) ) ;
#15852 = CARTESIAN_POINT ( 'NONE',  ( -5.012550801365594388, -3.368539882008727115, -1.828967928396028064 ) ) ;
#15853 = B_SPLINE_SURFACE_WITH_KNOTS ( 'NONE', 1, 3, ( 
 ( #6069, #25980, #23786, #21129, #31327, #8886, #5884, #16074 ),
 ( #26131, #6220, #898, #26305, #8552, #11075, #8405, #3415 ) ),
 .UNSPECIFIED., .F., .F., .F.,
 ( 2, 2 ),
 ( 4, 2, 2, 4 ),
 ( 0.000000000000000000, 1.000000000000000000 ),
 ( 0.000000000000000000, 0.5000000000000000000, 0.7500000000000000000, 1.000000000000000000 ),
 .UNSPECIFIED. ) ;
#15854 = CARTESIAN_POINT ( 'NONE',  ( 108.3527734911110088, 20.14254192115948072, 1.595847809240644288 ) ) ;
#15855 = LINE ( 'NONE', #834, #6984 ) ;
#15856 = ORIENTED_EDGE ( 'NONE', *, *, #24520, .F. ) ;
#15857 = ORIENTED_EDGE ( 'NONE', *, *, #20442, .F. ) ;
#15858 = CARTESIAN_POINT ( 'NONE',  ( 22.17354848663237732, -17.00157258782005343, -1.495009212619101246 ) ) ;
#15859 = DIRECTION ( 'NONE',  ( 0.000000000000000000, 0.000000000000000000, -1.000000000000000000 ) ) ;
#15860 = CARTESIAN_POINT ( 'NONE',  ( 85.20563808598728883, -3.194259795296060300, 4.522129901861162260 ) ) ;
#15861 = DIRECTION ( 'NONE',  ( 0.000000000000000000, -0.4067366430757888840, -0.9135454576426059736 ) ) ;
#15862 = CARTESIAN_POINT ( 'NONE',  ( 23.84714171513401126, -3.444070612163515843, -0.07017451552781626967 ) ) ;
#15863 = CARTESIAN_POINT ( 'NONE',  ( 56.97280603064898941, -277.2763395528616002, -1.491740999229417941 ) ) ;
#15864 = CARTESIAN_POINT ( 'NONE',  ( 85.14283307489681363, -6.932413485865820846, 0.4367664097854566663 ) ) ;
#15865 = ORIENTED_EDGE ( 'NONE', *, *, #4088, .T. ) ;
#15866 = CARTESIAN_POINT ( 'NONE',  ( 2.970200481232438516, -7.729547851449594553, -4.917777846806449915 ) ) ;
#15867 = EDGE_CURVE ( 'NONE', #3662, #23049, #30561, .T. ) ;
#15869 = EDGE_CURVE ( 'NONE', #32554, #30955, #9848, .T. ) ;
#15868 = ORIENTED_EDGE ( 'NONE', *, *, #17121, .T. ) ;
#15870 = CALENDAR_DATE ( 2026, 6, 10 ) ;
#15871 = CARTESIAN_POINT ( 'NONE',  ( 101.8933637717057223, -5.362948496501876328, -1.868788700206728048 ) ) ;
#15872 = VERTEX_POINT ( 'NONE', #7303 ) ;
#15873 = CARTESIAN_POINT ( 'NONE',  ( 0.7632845268398871230, 0.000000000000000000, 8.749000000000002331 ) ) ;
#15874 = ORIENTED_EDGE ( 'NONE', *, *, #13337, .F. ) ;
#15875 = FACE_OUTER_BOUND ( 'NONE', #29960, .T. ) ;
#15877 = VERTEX_POINT ( 'NONE', #15165 ) ;
#15876 = CARTESIAN_POINT ( 'NONE',  ( 18.85537384076560841, -4.793852932768607467, -4.073741754935396919 ) ) ;
#15878 = ORIENTED_EDGE ( 'NONE', *, *, #24682, .T. ) ;
#15879 = EDGE_CURVE ( 'NONE', #30480, #2170, #3008, .T. ) ;
#15880 = EDGE_CURVE ( 'NONE', #18631, #19567, #25424, .T. ) ;
#15881 = CARTESIAN_POINT ( 'NONE',  ( -0.3880080537174158128, -2.647099810593990465, -4.522129901861164925 ) ) ;
#15882 = CARTESIAN_POINT ( 'NONE',  ( -3.662550801365593411, -0.3701630799359326152, 3.521866450007987037 ) ) ;
#15883 = CARTESIAN_POINT ( 'NONE',  ( 3.499999999999999556, -6.200809695932770538, -0.7745709230445805282 ) ) ;
#15884 = LINE ( 'NONE', #23265, #12386 ) ;
#15886 = EDGE_LOOP ( 'NONE', ( #13261, #25465, #20284, #11450 ) ) ;
#15885 = CARTESIAN_POINT ( 'NONE',  ( 16.36487458112951643, 19.37645981759113312, -4.612695725900422872 ) ) ;
#15887 = CARTESIAN_POINT ( 'NONE',  ( 107.6033161557439115, -19.58148931974192664, 3.296621981446858918 ) ) ;
#15888 = CARTESIAN_POINT ( 'NONE',  ( 16.87315779138724992, 12.21951710860944473, 1.050000000000000044 ) ) ;
#15889 = CARTESIAN_POINT ( 'NONE',  ( -0.4074492901130932210, -14.65424174162825999, 1.499999999999921174 ) ) ;
#15891 = DIRECTION ( 'NONE',  ( 0.9947025833170223263, 0.1027947991993880261, -0.000000000000000000 ) ) ;
#15890 = APPLICATION_CONTEXT ( 'configuration controlled 3d designs of mechanical parts and assemblies' ) ;
#15892 = DIRECTION ( 'NONE',  ( -0.4999999999999981126, -0.8660254037844395958, 0.000000000000000000 ) ) ;
#15895 = EDGE_CURVE ( 'NONE', #21513, #28748, #7963, .T. ) ;
#15894 = ORIENTED_EDGE ( 'NONE', *, *, #27058, .F. ) ;
#15893 = LINE ( 'NONE', #3384, #7511 ) ;
#15896 = CARTESIAN_POINT ( 'NONE',  ( 101.7619443659971950, -3.470541747333645954, 3.636029349014984202 ) ) ;
#15897 = CARTESIAN_POINT ( 'NONE',  ( 2.692650308882783783, 9.794433827820187233, 2.271349672997489577 ) ) ;
#15898 = CARTESIAN_POINT ( 'NONE',  ( 24.23500000273118715, 2.486304738420679783, -0.2613211581691337604 ) ) ;
#15899 = CARTESIAN_POINT ( 'NONE',  ( -20.21556244645115541, 4.906976360849258256, 2.121007814587539286 ) ) ;
#15900 = ADVANCED_FACE ( 'NONE', ( #2477 ), #18154, .T. ) ;
#15901 = DIRECTION ( 'NONE',  ( 0.000000000000000000, 0.9063077870366462729, 0.4226182617407076014 ) ) ;
#15902 = CARTESIAN_POINT ( 'NONE',  ( -2.861038829132525496, 0.01832029024615380863, -1.013940918434634186 ) ) ;
#15903 = CARTESIAN_POINT ( 'NONE',  ( 107.9870691068026076, -17.88316047137711351, 4.509750785975439769 ) ) ;
#15904 = DIRECTION ( 'NONE',  ( 1.000000000000000000, 0.000000000000000000, 0.000000000000000000 ) ) ;
#15905 = EDGE_LOOP ( 'NONE', ( #30499, #17783, #919, #11694 ) ) ;
#15906 = CARTESIAN_POINT ( 'NONE',  ( 25.75999999999999801, 0.8512451026088739825, 2.902758476911987628 ) ) ;
#15907 = CARTESIAN_POINT ( 'NONE',  ( 5.885541736258995904, -8.006759975090634640, -2.519172009312012683 ) ) ;
#15908 = CARTESIAN_POINT ( 'NONE',  ( 2.857987970437215086, 8.861329655870090249, -3.588272043371362408 ) ) ;
#15910 = CARTESIAN_POINT ( 'NONE',  ( 108.0529998774959353, -18.83254716784343330, 4.756559617914289717 ) ) ;
#15909 = DIRECTION ( 'NONE',  ( -1.000000000000000000, 0.000000000000000000, 0.000000000000000000 ) ) ;
#15911 = EDGE_LOOP ( 'NONE', ( #28758, #8511, #15066, #23238 ) ) ;
#15912 = PLANE ( 'NONE',  #4856 ) ;
#15913 = EDGE_LOOP ( 'NONE', ( #12840, #31362, #20167, #3513 ) ) ;
#15914 = LINE ( 'NONE', #733, #5467 ) ;
#15916 = VERTEX_POINT ( 'NONE', #12793 ) ;
#15915 = DIRECTION ( 'NONE',  ( 1.000000000000000000, 0.000000000000000000, 7.709882115452493155E-15 ) ) ;
#15917 = ORIENTED_EDGE ( 'NONE', *, *, #10856, .T. ) ;
#15918 = CARTESIAN_POINT ( 'NONE',  ( 10.00000000000000000, -1.946309384392561626, -4.616489984850552730 ) ) ;
#15919 = EDGE_CURVE ( 'NONE', #8879, #22005, #5471, .T. ) ;
#15920 = EDGE_CURVE ( 'NONE', #7812, #32996, #15474, .T. ) ;
#15921 = PLANE ( 'NONE',  #7017 ) ;
#15923 = VERTEX_POINT ( 'NONE', #27691 ) ;
#15922 = DIRECTION ( 'NONE',  ( 1.000000000000000000, 0.000000000000000000, 0.000000000000000000 ) ) ;
#15924 = VERTEX_POINT ( 'NONE', #2808 ) ;
#15925 = LINE ( 'NONE', #16573, #17051 ) ;
#15926 = CARTESIAN_POINT ( 'NONE',  ( 22.01492382912217849, -21.80158502930435915, -1.372788961214118197 ) ) ;
#15927 = CARTESIAN_POINT ( 'NONE',  ( -53.62634062816648139, 4.812476404579010492, 5.128141679950119602 ) ) ;
#15928 = ADVANCED_FACE ( 'NONE', ( #25187 ), #12986, .T. ) ;
#15929 = CARTESIAN_POINT ( 'NONE',  ( 34.57258968893669504, -0.01303574654798587279, -3.062543865805531951 ) ) ;
#15930 = DIRECTION ( 'NONE',  ( 0.000000000000000000, 0.9945218953682729568, 0.1045284632676571068 ) ) ;
#15931 = CARTESIAN_POINT ( 'NONE',  ( 8.519413124347837041, -14.04790626066225023, 1.499999999999999334 ) ) ;
#15932 = DIRECTION ( 'NONE',  ( -0.000000000000000000, -0.000000000000000000, -1.000000000000000000 ) ) ;
#15933 = EDGE_CURVE ( 'NONE', #11141, #30909, #14973, .T. ) ;
#15934 = CARTESIAN_POINT ( 'NONE',  ( -3.312942406915326377, -5.022711880624455567E-15, 2.999999999999999556 ) ) ;
#15935 = PLANE ( 'NONE',  #6538 ) ;
#15936 = VERTEX_POINT ( 'NONE', #32906 ) ;
#15937 = CARTESIAN_POINT ( 'NONE',  ( 25.75999999999999801, -1.902510934646483477E-15, 2.499999999999997780 ) ) ;
#15938 = PLANE ( 'NONE',  #21479 ) ;
#15939 = CARTESIAN_POINT ( 'NONE',  ( 13.61463604683894069, 21.93665163297713150, -1.110659530650990323 ) ) ;
#15940 = VERTEX_POINT ( 'NONE', #11294 ) ;
#15941 = CARTESIAN_POINT ( 'NONE',  ( 22.79750000136559862, 2.363507492473148286, 1.913930629741525058 ) ) ;
#15942 = CARTESIAN_POINT ( 'NONE',  ( -15.06907680150159656, -25.68921844201283022, 1.340913934978426258 ) ) ;
#15943 = CARTESIAN_POINT ( 'NONE',  ( 0.000000000000000000, 6.704570150426983233, 5.172265885002680363 ) ) ;
#15944 = VERTEX_POINT ( 'NONE', #31374 ) ;
#15945 = CARTESIAN_POINT ( 'NONE',  ( 1.867614357912406930, -10.11604448560295744, -1.500000000000000444 ) ) ;
#15946 = VERTEX_POINT ( 'NONE', #8789 ) ;
#15947 = CARTESIAN_POINT ( 'NONE',  ( 41.43219399711119877, -3.145521524155372006, -1.915219082070890755 ) ) ;
#15948 = DATE_AND_TIME ( #5449, #13578 ) ;
#15950 = ORIENTED_EDGE ( 'NONE', *, *, #647, .T. ) ;
#15949 = CARTESIAN_POINT ( 'NONE',  ( 0.000000000000000000, 9.314797388894909602, -1.239665997526784746 ) ) ;
#15951 = ORIENTED_EDGE ( 'NONE', *, *, #29718, .T. ) ;
#15952 = CARTESIAN_POINT ( 'NONE',  ( 24.54750000136559507, 3.024605502323846729, -0.3178988483021056854 ) ) ;
#15953 = ADVANCED_FACE ( 'NONE', ( #26517 ), #21323, .T. ) ;
#15954 = ORIENTED_EDGE ( 'NONE', *, *, #23890, .F. ) ;
#15955 = CARTESIAN_POINT ( 'NONE',  ( 3.499999999999999556, 5.241389472434724084, -4.711457988287002685 ) ) ;
#15957 = VERTEX_POINT ( 'NONE', #16308 ) ;
#15956 = CARTESIAN_POINT ( 'NONE',  ( 29.33517104213873239, -3.852857368063288046, -1.169950485888521463 ) ) ;
#15958 = CARTESIAN_POINT ( 'NONE',  ( 85.49734435724778336, -7.913007294147514692, 0.07017451552781803215 ) ) ;
#15959 = CARTESIAN_POINT ( 'NONE',  ( 5.489343806296445472, 1.307372367723745654, -8.012901424861395228 ) ) ;
#15960 = LINE ( 'NONE', #21011, #21867 ) ;
#15961 = DIRECTION ( 'NONE',  ( -1.000000000000000000, 8.574039729943022041E-17, 1.232595164407830946E-32 ) ) ;
#15962 = ORIENTED_EDGE ( 'NONE', *, *, #13779, .F. ) ;
#15963 = CARTESIAN_POINT ( 'NONE',  ( -4.112942406915325755, -5.022711880624455567E-15, 2.999999999999999556 ) ) ;
#15964 = CARTESIAN_POINT ( 'NONE',  ( 42.13509523489886277, -21.36880892310108138, -5.485967528433937979 ) ) ;
#15965 = CARTESIAN_POINT ( 'NONE',  ( 18.62691943105446057, -7.347514731314632286, -1.529339877378613100 ) ) ;
#15966 = CARTESIAN_POINT ( 'NONE',  ( 7.249760686538667009, 0.000000000000000000, 0.000000000000000000 ) ) ;
#15967 = EDGE_CURVE ( 'NONE', #17163, #25473, #3472, .T. ) ;
#15968 = CARTESIAN_POINT ( 'NONE',  ( 3.063284526839887167, 0.000000000000000000, 0.000000000000000000 ) ) ;
#15969 = DIRECTION ( 'NONE',  ( -0.000000000000000000, -0.000000000000000000, -1.000000000000000000 ) ) ;
#15970 = CARTESIAN_POINT ( 'NONE',  ( 24.24290772321993970, 0.1310194482076003919, 2.499999999999998668 ) ) ;
#15971 = DIRECTION ( 'NONE',  ( 3.469446951953478110E-15, -0.000000000000000000, -1.000000000000000000 ) ) ;
#15972 = CARTESIAN_POINT ( 'NONE',  ( -27.61335648245702501, 5.440830098941747295, 2.106297401565270011 ) ) ;
#15973 = CARTESIAN_POINT ( 'NONE',  ( -3.062550801365593323, 3.521866450007987037, 0.3701630799359328372 ) ) ;
#15974 = VERTEX_POINT ( 'NONE', #31526 ) ;
#15975 = CARTESIAN_POINT ( 'NONE',  ( -4.404531657079157725, 2.325406398514293205, -1.883076972206379374 ) ) ;
#15976 = CIRCLE ( 'NONE', #4776, 10.01776515689528502 ) ;
#15977 = CARTESIAN_POINT ( 'NONE',  ( 10.56183597391177464, 5.003758587302147731, -0.2499999999999991951 ) ) ;
#15978 = CARTESIAN_POINT ( 'NONE',  ( -5.250050800000000351, 1.549418761218566143, -2.853674364686379583 ) ) ;
#15979 = CARTESIAN_POINT ( 'NONE',  ( 8.789577373539158245, -11.69574158658721252, 1.500000000000000000 ) ) ;
#15980 = VERTEX_POINT ( 'NONE', #21178 ) ;
#15981 = CARTESIAN_POINT ( 'NONE',  ( 40.87760899951555160, -5.748707280016356336, -3.993433839269025842 ) ) ;
#15982 = ADVANCED_FACE ( 'NONE', ( #13629 ), #31635, .T. ) ;
#15983 = CIRCLE ( 'NONE', #5846, 0.5000000000000000000 ) ;
#15984 = ORIENTED_EDGE ( 'NONE', *, *, #1021, .T. ) ;
#15985 = CARTESIAN_POINT ( 'NONE',  ( -29.86426557179348507, 4.845260731991870351, 5.128141679950118714 ) ) ;
#15986 = EDGE_CURVE ( 'NONE', #8919, #27372, #27269, .T. ) ;
#15987 = DATE_TIME_ROLE ( 'classification_date' ) ;
#15988 = CARTESIAN_POINT ( 'NONE',  ( 102.3526732589231898, -2.980372452608875733, 4.155404932455299516 ) ) ;
#15989 = CARTESIAN_POINT ( 'NONE',  ( 5.489321486716459475, -7.976795196726676807, -1.512021494499669716 ) ) ;
#15990 = CARTESIAN_POINT ( 'NONE',  ( 7.064632918400242545, 8.437262856154193358, -2.318425219014147665 ) ) ;
#15991 = ORIENTED_EDGE ( 'NONE', *, *, #15522, .F. ) ;
#15992 = CARTESIAN_POINT ( 'NONE',  ( 7.064423600674403225, -8.466096581344336514, 2.210816291637388797 ) ) ;
#15993 = CARTESIAN_POINT ( 'NONE',  ( 25.39414263582314746, 18.98424558132892770, -1.448744400657052234 ) ) ;
#15994 = CARTESIAN_POINT ( 'NONE',  ( 21.54750000136559507, 1.913930629741522838, -2.363507492473150062 ) ) ;
#15995 = TOROIDAL_SURFACE ( 'NONE', #30969, 6.923700951379997193, 9.000000000000000000 ) ;
#15996 = EDGE_LOOP ( 'NONE', ( #20221, #12132, #736, #5745 ) ) ;
#15997 = CARTESIAN_POINT ( 'NONE',  ( -2.262550801365593056, 3.521866450007987037, 0.3701630799359328372 ) ) ;
#15998 = LINE ( 'NONE', #21061, #11342 ) ;
#15999 = DIRECTION ( 'NONE',  ( 0.000000000000000000, -0.9510565162951504226, -0.3090169943749573322 ) ) ;
#16000 = EDGE_LOOP ( 'NONE', ( #20962, #17336 ) ) ;
#16001 = EDGE_LOOP ( 'NONE', ( #15444, #18615, #26126, #20857 ) ) ;
#16002 = AXIS2_PLACEMENT_3D ( 'NONE', #8604, #3467, #23670 ) ;
#16003 = FACE_OUTER_BOUND ( 'NONE', #385, .T. ) ;
#16004 = DIRECTION ( 'NONE',  ( 0.000000000000000000, 1.000000000000000000, 0.000000000000000000 ) ) ;
#16005 = ORIENTED_EDGE ( 'NONE', *, *, #13975, .T. ) ;
#16006 = CARTESIAN_POINT ( 'NONE',  ( 7.249760686538667009, -7.892520144992443143, 1.391664247347202288 ) ) ;
#16007 = DIRECTION ( 'NONE',  ( 0.8247831655431905329, -0.5654491399202531410, 0.000000000000000000 ) ) ;
#16008 = CARTESIAN_POINT ( 'NONE',  ( 0.7632845268398871230, 8.152713396088806519, -3.174628368995990879 ) ) ;
#16009 = CARTESIAN_POINT ( 'NONE',  ( -2.787550801365593411, -3.521866450007987037, -0.3701630799359323931 ) ) ;
#16010 = AXIS2_PLACEMENT_3D ( 'NONE', #11523, #11366, #29908 ) ;
#16011 = CARTESIAN_POINT ( 'NONE',  ( 0.6728000631899151429, -9.133409206477399067, -0.5626559339043897268 ) ) ;
#16012 = CARTESIAN_POINT ( 'NONE',  ( 21.32535692059145660, -21.82495604402121003, -1.318256435726663955 ) ) ;
#16013 = VERTEX_POINT ( 'NONE', #13776 ) ;
#16014 = ADVANCED_FACE ( 'NONE', ( #13145 ), #18646, .T. ) ;
#16015 = CARTESIAN_POINT ( 'NONE',  ( -5.762942409646513831, 3.284080845023683730E-15, 3.000000000000000000 ) ) ;
#16016 = EDGE_CURVE ( 'NONE', #29157, #18318, #26596, .T. ) ;
#16017 = AXIS2_PLACEMENT_3D ( 'NONE', #20796, #22346, #10438 ) ;
#16018 = ORIENTED_EDGE ( 'NONE', *, *, #15522, .T. ) ;
#16019 = PERSON_AND_ORGANIZATION ( #6766, #25292 ) ;
#16020 = CARTESIAN_POINT ( 'NONE',  ( 101.9038547928002316, -5.514016590425875997, -1.527295561052322892 ) ) ;
#16021 = CIRCLE ( 'NONE', #3759, 10.51776515689528502 ) ;
#16022 = LINE ( 'NONE', #16214, #3961 ) ;
#16023 = ORIENTED_EDGE ( 'NONE', *, *, #11968, .F. ) ;
#16024 = DIRECTION ( 'NONE',  ( 0.000000000000000000, 0.000000000000000000, -1.000000000000000000 ) ) ;
#16025 = ORIENTED_EDGE ( 'NONE', *, *, #17942, .T. ) ;
#16026 = ORIENTED_EDGE ( 'NONE', *, *, #24585, .F. ) ;
#16027 = CYLINDRICAL_SURFACE ( 'NONE', #17228, 0.5000000000000000000 ) ;
#16028 = CARTESIAN_POINT ( 'NONE',  ( -5.612550801365594033, 1.828967928396027398, -3.368539882008727115 ) ) ;
#16029 = CARTESIAN_POINT ( 'NONE',  ( 0.000000000000000000, 19.51744974835125035, 0.000000000000000000 ) ) ;
#16030 = CARTESIAN_POINT ( 'NONE',  ( 0.8232120717395272624, -3.227314771018384487, -1.762270855091927491 ) ) ;
#16032 = VERTEX_POINT ( 'NONE', #3617 ) ;
#16031 = DIRECTION ( 'NONE',  ( -1.000000000000000000, -0.000000000000000000, -0.000000000000000000 ) ) ;
#16033 = CARTESIAN_POINT ( 'NONE',  ( -7.887550801365593500, 2.228590825266444142, 2.752080473201636845 ) ) ;
#16034 = CARTESIAN_POINT ( 'NONE',  ( 11.66870695124253743, 3.948484734076533442, 1.499999999999881650 ) ) ;
#16035 = CARTESIAN_POINT ( 'NONE',  ( 6.069864835170823980, -18.63409169915096442, 1.499999999999999112 ) ) ;
#16036 = CARTESIAN_POINT ( 'NONE',  ( 22.04750000136559507, -3.024605502323851169, 0.3178988483021052969 ) ) ;
#16037 = VECTOR ( 'NONE', #23336, 1000.000000000000000 ) ;
#16038 = LINE ( 'NONE', #13072, #13869 ) ;
#16040 = ORIENTED_EDGE ( 'NONE', *, *, #16053, .F. ) ;
#16039 = CARTESIAN_POINT ( 'NONE',  ( 24.13073845333548206, -17.43243825926032642, 1.517345177934881439 ) ) ;
#16041 = CIRCLE ( 'NONE', #27244, 5.010000000000000675 ) ;
#16042 = VECTOR ( 'NONE', #15348, 1000.000000000000114 ) ;
#16043 = CARTESIAN_POINT ( 'NONE',  ( -25.33717935682962619, 4.262548611904803053, 2.138841724730499827 ) ) ;
#16044 = CARTESIAN_POINT ( 'NONE',  ( 22.42250000273118715, 1.291182301015469047, 2.378061970571981654 ) ) ;
#16045 = CARTESIAN_POINT ( 'NONE',  ( -18.33450643518137113, 6.805598625771001942, 1.500000000000411893 ) ) ;
#16046 = CYLINDRICAL_SURFACE ( 'NONE', #28916, 0.5000000000000004441 ) ;
#16047 = DIRECTION ( 'NONE',  ( 1.000000000000000000, -0.000000000000000000, -0.000000000000000000 ) ) ;
#16048 = AXIS2_PLACEMENT_3D ( 'NONE', #31282, #25930, #28746 ) ;
#16049 = EDGE_CURVE ( 'NONE', #18044, #26528, #13460, .T. ) ;
#16050 = DIRECTION ( 'NONE',  ( -0.000000000000000000, -0.8191520442889868026, -0.5735764363510532649 ) ) ;
#16051 = CARTESIAN_POINT ( 'NONE',  ( 9.296291922083815606, 0.2373464012013740410, 1.049642900790956901 ) ) ;
#16052 = ORIENTED_EDGE ( 'NONE', *, *, #24435, .F. ) ;
#16053 = EDGE_CURVE ( 'NONE', #18491, #31391, #28434, .T. ) ;
#16054 = B_SPLINE_CURVE_WITH_KNOTS ( 'NONE', 3,
 ( #6265, #6121, #21808, #32015, #16805, #29328, #26361, #21317, #16618, #4105 ),
 .UNSPECIFIED., .F., .F.,
 ( 4, 2, 2, 2, 4 ),
 ( 1.968338519012285137E-07, 0.0005467926089500458166, 0.001093388384048190427, 0.001639984159146335146, 0.002186579934244479648 ),
 .UNSPECIFIED. ) ;
#16055 = B_SPLINE_CURVE_WITH_KNOTS ( 'NONE', 3,
 ( #15749, #28619, #8524, #3694, #24062, #18728, #28932, #28454 ),
 .UNSPECIFIED., .F., .F.,
 ( 4, 2, 2, 4 ),
 ( 2.213836054437087486E-07, 0.001261154818855359178, 0.001891621536480315915, 0.002522088254105272868 ),
 .UNSPECIFIED. ) ;
#16056 = DIRECTION ( 'NONE',  ( 1.000000000000000000, 0.000000000000000000, 0.000000000000000000 ) ) ;
#16057 = CIRCLE ( 'NONE', #17143, 302.1720608278465079 ) ;
#16058 = CARTESIAN_POINT ( 'NONE',  ( 6.880159540721329847, -8.414807581959442118, -2.328896285337273664 ) ) ;
#16059 = ADVANCED_FACE ( 'NONE', ( #8453 ), #3175, .T. ) ;
#16060 = CARTESIAN_POINT ( 'NONE',  ( -42.46793790805478608, 24.51887538314362658, -1.050000000000000044 ) ) ;
#16062 = CARTESIAN_POINT ( 'NONE',  ( 107.9488651208191357, -17.33303257717642154, 4.540600388780822172 ) ) ;
#16061 = DIRECTION ( 'NONE',  ( 0.000000000000000000, 0.000000000000000000, 1.000000000000000000 ) ) ;
#16063 = ORIENTED_EDGE ( 'NONE', *, *, #5555, .T. ) ;
#16064 = AXIS2_PLACEMENT_3D ( 'NONE', #20972, #31189, #9012 ) ;
#16065 = CIRCLE ( 'NONE', #11806, 5.010000000000000675 ) ;
#16066 = CARTESIAN_POINT ( 'NONE',  ( -4.700050800000001416, -2.983565686104819648, -0.3135853898029605791 ) ) ;
#16067 = CIRCLE ( 'NONE', #12359, 6.818740222761507042 ) ;
#16068 = ORIENTED_EDGE ( 'NONE', *, *, #11259, .F. ) ;
#16069 = DIRECTION ( 'NONE',  ( -1.000000000000000000, 0.000000000000000000, 0.000000000000000000 ) ) ;
#16071 = VERTEX_POINT ( 'NONE', #6423 ) ;
#16070 = DIRECTION ( 'NONE',  ( 0.000000000000000000, 0.000000000000000000, -1.000000000000000000 ) ) ;
#16072 = EDGE_CURVE ( 'NONE', #25185, #3234, #26836, .T. ) ;
#16073 = VERTEX_POINT ( 'NONE', #22161 ) ;
#16074 = CARTESIAN_POINT ( 'NONE',  ( 18.68265047573912341, -6.724553502642427461, -4.522129901861164036 ) ) ;
#16076 = CIRCLE ( 'NONE', #1688, 0.5000000000000004441 ) ;
#16075 = DIRECTION ( 'NONE',  ( -1.000000000000000000, 8.574039729943022041E-17, 1.232595164407830946E-32 ) ) ;
#16077 = B_SPLINE_CURVE_WITH_KNOTS ( 'NONE', 3,
 ( #19604, #30462, #2398, #1905, #9723, #10049, #30159, #12078 ),
 .UNSPECIFIED., .F., .F.,
 ( 4, 2, 2, 4 ),
 ( 2.049880227661072435E-07, 0.001261138121172438592, 0.001891604687747274784, 0.002522071254322110975 ),
 .UNSPECIFIED. ) ;
#16079 = ORIENTED_EDGE ( 'NONE', *, *, #19980, .F. ) ;
#16078 = CARTESIAN_POINT ( 'NONE',  ( 6.037141869538513284, -3.843044125430119529, 7.552970526864677403 ) ) ;
#16080 = CARTESIAN_POINT ( 'NONE',  ( 13.87075382807543988, 7.736340727907119685, -1.499999999999170441 ) ) ;
#16081 = CARTESIAN_POINT ( 'NONE',  ( -3.765825760583550785, -9.391035046880782389, -1.743616693177291843 ) ) ;
#16082 = ADVANCED_FACE ( 'NONE', ( #27004 ), #29843, .T. ) ;
#16083 = CARTESIAN_POINT ( 'NONE',  ( 0.000000000000000000, 0.000000000000000000, 0.000000000000000000 ) ) ;
#16084 = CARTESIAN_POINT ( 'NONE',  ( 20.69346795579692255, -16.15118080677321188, -1.499999999998890887 ) ) ;
#16085 = CARTESIAN_POINT ( 'NONE',  ( 107.9802354097229369, -17.78475693344107711, -4.325021386167422044 ) ) ;
#16086 = CARTESIAN_POINT ( 'NONE',  ( 56.97280603064898941, -277.2763395528616002, -4.999054092451819642 ) ) ;
#16087 = ADVANCED_FACE ( 'NONE', ( #32018 ), #9431, .T. ) ;
#16088 = VECTOR ( 'NONE', #18467, 1000.000000000000000 ) ;
#16089 = CARTESIAN_POINT ( 'NONE',  ( -6.850050799999999995, 1.549418761218566143, -2.853674364686379583 ) ) ;
#16090 = CARTESIAN_POINT ( 'NONE',  ( 0.8609591700481805665, -8.439992987522430212, 1.499999999999999334 ) ) ;
#16091 = CARTESIAN_POINT ( 'NONE',  ( 23.64679384717597443, -7.447389048103699061, 2.184956778805557498 ) ) ;
#16092 = AXIS2_PLACEMENT_3D ( 'NONE', #29474, #9233, #18778 ) ;
#16093 = CARTESIAN_POINT ( 'NONE',  ( 25.75999999999999801, -2.208672634433321348E-15, 0.000000000000000000 ) ) ;
#16094 = CARTESIAN_POINT ( 'NONE',  ( 7.249760686538667009, 5.064320921489914973, -7.135485519861949122 ) ) ;
#16095 = ORIENTED_EDGE ( 'NONE', *, *, #30633, .T. ) ;
#16096 = CARTESIAN_POINT ( 'NONE',  ( 41.19430503359222939, -3.886431767407559246, 0.07017451552849453267 ) ) ;
#16097 = VECTOR ( 'NONE', #6727, 1000.000000000000000 ) ;
#16098 = ADVANCED_FACE ( 'NONE', ( #17116 ), #13211, .T. ) ;
#16099 = VECTOR ( 'NONE', #23571, 1000.000000000000000 ) ;
#16100 = CARTESIAN_POINT ( 'NONE',  ( 107.7451628514262723, 16.75912612768599885, 1.294109110054813661 ) ) ;
#16101 = ADVANCED_FACE ( 'NONE', ( #7926 ), #29956, .F. ) ;
#16102 = CARTESIAN_POINT ( 'NONE',  ( 25.75999999999999801, -1.902510934646483477E-15, 2.499999999999997780 ) ) ;
#16103 = ORIENTED_EDGE ( 'NONE', *, *, #21010, .T. ) ;
#16104 = CARTESIAN_POINT ( 'NONE',  ( 22.48500000136559507, 0.9349337715887185984, -3.156283516753368268 ) ) ;
#16105 = AXIS2_PLACEMENT_3D ( 'NONE', #6360, #20944, #31641 ) ;
#16106 = VECTOR ( 'NONE', #30259, 1000.000000000000000 ) ;
#16107 = CARTESIAN_POINT ( 'NONE',  ( 10.00000000000000000, -2.376879293651037006, -4.116875700062107235 ) ) ;
#16108 = CARTESIAN_POINT ( 'NONE',  ( 0.7632845268398879002, -8.152713396088778097, 3.174628368996039729 ) ) ;
#16109 = ORIENTED_EDGE ( 'NONE', *, *, #1497, .T. ) ;
#16110 = CARTESIAN_POINT ( 'NONE',  ( 0.5630814792739097241, -7.170012529492013620, -1.499999999999999556 ) ) ;
#16111 = EDGE_CURVE ( 'NONE', #10948, #3034, #28007, .T. ) ;
#16112 = ORIENTED_EDGE ( 'NONE', *, *, #14787, .T. ) ;
#16113 = AXIS2_PLACEMENT_3D ( 'NONE', #4371, #29943, #30137 ) ;
#16114 = ORIENTED_EDGE ( 'NONE', *, *, #21956, .F. ) ;
#16115 = CARTESIAN_POINT ( 'NONE',  ( 25.38393466668145493, -17.54878733605299601, -1.232996826557628545 ) ) ;
#16116 = B_SPLINE_SURFACE_WITH_KNOTS ( 'NONE', 3, 1, ( 
 ( #13726, #6214 ),
 ( #20948, #31809 ),
 ( #18446, #8253 ),
 ( #31167, #5589 ) ),
 .UNSPECIFIED., .F., .F., .F.,
 ( 4, 4 ),
 ( 2, 2 ),
 ( 0.000000000000000000, 0.9914900096613892266 ),
 ( 0.000000000000000000, 1.000000000000000000 ),
 .UNSPECIFIED. ) ;
#16117 = COORDINATED_UNIVERSAL_TIME_OFFSET ( 0, 0, .AHEAD. ) ;
#16118 = AXIS2_PLACEMENT_3D ( 'NONE', #9406, #11742, #27633 ) ;
#16120 = ORIENTED_EDGE ( 'NONE', *, *, #14839, .F. ) ;
#16119 = CARTESIAN_POINT ( 'NONE',  ( -1.331261126404138517, -14.27417440010677652, -0.9788672205760856615 ) ) ;
#16121 = ORIENTED_EDGE ( 'NONE', *, *, #8507, .T. ) ;
#16122 = CARTESIAN_POINT ( 'NONE',  ( 10.56870887191539587, 4.787500056513386504, -1.476463073999588538 ) ) ;
#16123 = AXIS2_PLACEMENT_3D ( 'NONE', #9328, #20051, #9145 ) ;
#16124 = CIRCLE ( 'NONE', #17208, 8.750000000000000000 ) ;
#16125 = EDGE_CURVE ( 'NONE', #6480, #29275, #19810, .T. ) ;
#16126 = VERTEX_POINT ( 'NONE', #30194 ) ;
#16127 = FACE_OUTER_BOUND ( 'NONE', #15678, .T. ) ;
#16129 = ORIENTED_EDGE ( 'NONE', *, *, #3302, .T. ) ;
#16128 = CARTESIAN_POINT ( 'NONE',  ( 23.87614828266624301, -3.446665583135119171, -0.07017451552781975299 ) ) ;
#16130 = AXIS2_PLACEMENT_3D ( 'NONE', #3166, #8654, #29219 ) ;
#16131 = CYLINDRICAL_SURFACE ( 'NONE', #5505, 4.000000000000001776 ) ;
#16132 = CARTESIAN_POINT ( 'NONE',  ( 6.038144483126824724, -0.4487862922133833421, 8.463061282283012687 ) ) ;
#16133 = CIRCLE ( 'NONE', #14531, 3.499999999999999556 ) ;
#16134 = CARTESIAN_POINT ( 'NONE',  ( 7.249760686538667009, 8.437262856154195134, -2.318425219014145444 ) ) ;
#16135 = CARTESIAN_POINT ( 'NONE',  ( 0.7212197624752703096, 8.661246924783327472, -2.263408446298125654 ) ) ;
#16137 = CARTESIAN_POINT ( 'NONE',  ( 108.0271851702406138, -18.46082180526434513, 4.398261384118815620 ) ) ;
#16136 = TOROIDAL_SURFACE ( 'NONE', #20431, 10.51999999999999957, 0.4500000000000000111 ) ;
#16138 = CARTESIAN_POINT ( 'NONE',  ( -5.338982705821066855E-17, -0.6226916219172391465, 4.971152295393299170 ) ) ;
#16139 = CARTESIAN_POINT ( 'NONE',  ( -2.767073886773233848, -0.6621507858625382825, -1.748408842879326075 ) ) ;
#16140 = DIRECTION ( 'NONE',  ( -0.000000000000000000, -0.000000000000000000, -1.000000000000000000 ) ) ;
#16141 = CARTESIAN_POINT ( 'NONE',  ( 3.500000000000000000, 7.347880794884119736E-16, -6.000000000000000000 ) ) ;
#16142 = EDGE_CURVE ( 'NONE', #21273, #685, #14205, .T. ) ;
#16143 = DIRECTION ( 'NONE',  ( -0.000000000000000000, -0.000000000000000000, -1.000000000000000000 ) ) ;
#16144 = CIRCLE ( 'NONE', #3871, 8.500000000000000000 ) ;
#16145 = DIRECTION ( 'NONE',  ( -1.000000000000000000, 0.000000000000000000, 0.000000000000000000 ) ) ;
#16146 = DIRECTION ( 'NONE',  ( -1.000000000000000000, 0.000000000000000000, -0.000000000000000000 ) ) ;
#16147 = LINE ( 'NONE', #5649, #21454 ) ;
#16148 = AXIS2_PLACEMENT_3D ( 'NONE', #26114, #3875, #15904 ) ;
#16149 = ADVANCED_FACE ( 'NONE', ( #7415 ), #28954, .T. ) ;
#16150 = CIRCLE ( 'NONE', #32190, 8.500000000000000000 ) ;
#16151 = CARTESIAN_POINT ( 'NONE',  ( 21.30656763371926132, -0.8852964313267484009, 2.499999999999997780 ) ) ;
#16152 = CARTESIAN_POINT ( 'NONE',  ( -2.812550801365592879, -1.828967928396026510, 3.368539882008728004 ) ) ;
#16153 = VERTEX_POINT ( 'NONE', #32866 ) ;
#16154 = AXIS2_PLACEMENT_3D ( 'NONE', #5863, #16047, #23766 ) ;
#16155 = CIRCLE ( 'NONE', #1758, 0.5000000000000000000 ) ;
#16156 = CARTESIAN_POINT ( 'NONE',  ( -4.900050799999999818, -0.3135853898029607456, 2.983565686104819648 ) ) ;
#16157 = CARTESIAN_POINT ( 'NONE',  ( 108.1033190409114155, 18.75348111242300320, 4.532405430181406736 ) ) ;
#16158 = DIRECTION ( 'NONE',  ( 0.000000000000000000, 1.000000000000000000, 0.000000000000000000 ) ) ;
#16159 = CARTESIAN_POINT ( 'NONE',  ( 7.845473912040171527, -1.949903631124794146, 1.500000000000000000 ) ) ;
#16160 = ORIENTED_EDGE ( 'NONE', *, *, #15452, .T. ) ;
#16161 = CARTESIAN_POINT ( 'NONE',  ( 28.70307564580845749, -5.239617037334318717, -3.390608483621579516 ) ) ;
#16162 = AXIS2_PLACEMENT_3D ( 'NONE', #14878, #25080, #14566 ) ;
#16163 = VERTEX_POINT ( 'NONE', #10088 ) ;
#16164 = CARTESIAN_POINT ( 'NONE',  ( 0.2476201786951250650, -6.180873974445452390, 1.500000000000142997 ) ) ;
#16165 = PERSON_AND_ORGANIZATION_ROLE ( 'design_supplier' ) ;
#16166 = CARTESIAN_POINT ( 'NONE',  ( 18.85603800621453630, -4.786428896025966218, 4.074610069492402786 ) ) ;
#16167 = EDGE_CURVE ( 'NONE', #4208, #18809, #32636, .T. ) ;
#16168 = B_SPLINE_CURVE_WITH_KNOTS ( 'NONE', 3,
 ( #9868, #30276, #7199, #19727, #29925, #27736, #2364, #22083, #9187, #29613, #19570, #17538, #22242, #19414, #25245, #6695, #32792, #17393 ),
 .UNSPECIFIED., .F., .F.,
 ( 4, 2, 2, 2, 2, 2, 2, 2, 4 ),
 ( 0.0006071315980451493302, 0.003701157179670942245, 0.006795182761296735159, 0.009889208342922527206, 0.01298323392454832012, 0.01607725950617410957, 0.01917128508779990248, 0.02226531066942568846, 0.02535933625105148137 ),
 .UNSPECIFIED. ) ;
#16169 = CARTESIAN_POINT ( 'NONE',  ( 9.302055952158307051, 0.2457637072682087309, 1.499999999976339371 ) ) ;
#16170 = AXIS2_PLACEMENT_3D ( 'NONE', #5814, #3506, #30772 ) ;
#16171 = CYLINDRICAL_SURFACE ( 'NONE', #27276, 5.010000000000000675 ) ;
#16172 = DIRECTION ( 'NONE',  ( 0.000000000000000000, 0.9510565162951544194, -0.3090169943749449533 ) ) ;
#16173 = AXIS2_PLACEMENT_3D ( 'NONE', #17364, #17185, #3832 ) ;
#16174 = VERTEX_POINT ( 'NONE', #2592 ) ;
#16175 = VECTOR ( 'NONE', #3440, 1000.000000000000000 ) ;
#16176 = CARTESIAN_POINT ( 'NONE',  ( 5.885541615502094537, -8.193643496140865068, 1.821712961073320480 ) ) ;
#16177 = DIRECTION ( 'NONE',  ( 1.224646799147353207E-16, 1.000000000000000000, -0.000000000000000000 ) ) ;
#16178 = CIRCLE ( 'NONE', #25287, 0.4499999999999999001 ) ;
#16179 = CARTESIAN_POINT ( 'NONE',  ( 2.976845970491565296, -7.079702685456837230, -5.822399416825385643 ) ) ;
#16180 = VECTOR ( 'NONE', #24406, 1000.000000000000000 ) ;
#16182 = ORIENTED_EDGE ( 'NONE', *, *, #27552, .F. ) ;
#16181 = CARTESIAN_POINT ( 'NONE',  ( 1.565787006715318563, -2.348723853601413669, 0.9788672205888330202 ) ) ;
#16183 = CARTESIAN_POINT ( 'NONE',  ( -3.262550801365593056, 0.3701630799359330593, -3.521866450007987037 ) ) ;
#16184 = AXIS2_PLACEMENT_3D ( 'NONE', #32407, #14308, #14161 ) ;
#16185 = CARTESIAN_POINT ( 'NONE',  ( 108.2963978243841296, 19.82861996404848881, 2.265613416507222144 ) ) ;
#16186 = CARTESIAN_POINT ( 'NONE',  ( 47.94941403272093083, -7.827919050457508909, -2.184956529774258804 ) ) ;
#16187 = LOCAL_TIME ( 16, 7, 10.00000000000000000, #18217 ) ;
#16188 = ORIENTED_EDGE ( 'NONE', *, *, #8449, .T. ) ;
#16189 = ORIENTED_EDGE ( 'NONE', *, *, #3702, .T. ) ;
#16190 = EDGE_CURVE ( 'NONE', #30204, #2520, #14526, .T. ) ;
#16191 = LINE ( 'NONE', #32067, #23620 ) ;
#16192 = FACE_OUTER_BOUND ( 'NONE', #32138, .T. ) ;
#16193 = LINE ( 'NONE', #26417, #16732 ) ;
#16194 = CARTESIAN_POINT ( 'NONE',  ( 0.004027955751649570440, -11.10248303872730169, 5.485967528433933538 ) ) ;
#16195 = EDGE_CURVE ( 'NONE', #10544, #7488, #4354, .T. ) ;
#16196 = CARTESIAN_POINT ( 'NONE',  ( 18.93617721851659041, -3.890633339435721982, 4.522129901861162260 ) ) ;
#16197 = CARTESIAN_POINT ( 'NONE',  ( 4.749760686538667009, 2.741043480754926875, 7.530955069117522882 ) ) ;
#16198 = VECTOR ( 'NONE', #11923, 1000.000000000000000 ) ;
#16199 = LINE ( 'NONE', #9481, #26284 ) ;
#16200 = VECTOR ( 'NONE', #5728, 1000.000000000000114 ) ;
#16201 = CARTESIAN_POINT ( 'NONE',  ( 107.4763673390317962, -17.74216696756428391, -5.015857065170183482 ) ) ;
#16202 = CIRCLE ( 'NONE', #5535, 8.750000000000000000 ) ;
#16203 = CARTESIAN_POINT ( 'NONE',  ( 0.9801757370192288876, 20.00000000000000000, -6.747923662139670320 ) ) ;
#16204 = DIRECTION ( 'NONE',  ( 0.000000000000000000, 0.000000000000000000, 1.000000000000000000 ) ) ;
#16205 = ORIENTED_EDGE ( 'NONE', *, *, #427, .T. ) ;
#16206 = DIRECTION ( 'NONE',  ( 0.000000000000000000, 6.938893903907228378E-15, 1.000000000000000000 ) ) ;
#16207 = CIRCLE ( 'NONE', #23171, 8.749000000000002331 ) ;
#16208 = CIRCLE ( 'NONE', #19334, 8.749000000000002331 ) ;
#16209 = B_SPLINE_CURVE_WITH_KNOTS ( 'NONE', 3,
 ( #5067, #14482, #19182, #1478, #21849, #29882, #706, #4145 ),
 .UNSPECIFIED., .F., .F.,
 ( 4, 2, 2, 4 ),
 ( 2.494123658409239446E-07, 0.001262099805927711102, 0.001893025002708644509, 0.002523950199489578133 ),
 .UNSPECIFIED. ) ;
#16210 = VERTEX_POINT ( 'NONE', #14778 ) ;
#16211 = PERSON_AND_ORGANIZATION_ROLE ( 'design_supplier' ) ;
#16213 = CARTESIAN_POINT ( 'NONE',  ( 24.39659513448100725, -17.41072360183587264, -1.416990234759457401 ) ) ;
#16212 = LOCAL_TIME ( 16, 7, 10.00000000000000000, #29201 ) ;
#16214 = CARTESIAN_POINT ( 'NONE',  ( 1.750000000000000222, 4.438567988583182355, -7.249076783337631724 ) ) ;
#16215 = ORIENTED_EDGE ( 'NONE', *, *, #7251, .T. ) ;
#16216 = CARTESIAN_POINT ( 'NONE',  ( -3.103992766986577667, 8.326672684866362132E-14, -1.052556072988602986 ) ) ;
#16217 = ORIENTED_EDGE ( 'NONE', *, *, #2811, .F. ) ;
#16218 = ORIENTED_EDGE ( 'NONE', *, *, #25213, .T. ) ;
#16219 = LINE ( 'NONE', #26255, #24162 ) ;
#16220 = CARTESIAN_POINT ( 'NONE',  ( -4.462550801365592790, -0.3701630799359326152, 3.521866450007987037 ) ) ;
#16221 = CARTESIAN_POINT ( 'NONE',  ( 26.04750000000000298, 2.594547506269380133, 0.7685399846772031918 ) ) ;
#16222 = CARTESIAN_POINT ( 'NONE',  ( 1.635938383118674677, -1.437486021841400730, -1.758786398149086327 ) ) ;
#16223 =( BOUNDED_SURFACE ( )  B_SPLINE_SURFACE ( 1, 2, ( 
 ( #988, #11168, #21372, #12016, #27879, #25024, #4993, #27701, #14825, #1833, #15176, #7316, #32266, #17667, #9327, #30244, #7168, #25381, #17506, #2138, #4317, #12318, #32757, #19871, #4651, #32575, #22538, #17361, #29737, #9833, #6815, #32419, #20050, #2489, #4807, #22714, #14983, #19540, #27204, #25202, #9986, #14494, #14677, #27554, #12658, #24707, #2325, #19695, #17003, #22210, #9645, #12507, #4503, #9480, #29893, #32917, #7466, #6974, #20197, #30393, #17181, #27392, #24877, #1989, #12162, #22360, #30085, #33063, #5798, #10137, #30753, #30576, #21032, #20849, #31060, #23510, #7825, #142, #20359, #5488, #10489, #20702, #15975, #26198, #18019, #462, #25700, #28206, #5308, #28555, #23020, #18357, #5652, #15486, #8315, #2826, #13002, #23212, #26042, #621, #317, #15832, #18511, #30903, #28057, #3144, #13155, #13302, #10330, #20543, #10817, #15679, #22861, #31240, #7974, #28705, #28372, #3306, #7660, #18167, #17858 ),
 ( #25888, #10642, #5154, #15329, #3002, #25535, #2641, #23355, #8149, #12806, #23989, #11476, #19007, #29341, #29193, #11134, #26850, #31878, #3967, #26529, #6623, #16463, #31540, #16816, #29047, #1297, #8945, #9101, #16320, #21333, #6136, #14137, #21671, #23844, #5957, #24337, #1449, #16638, #32030, #955, #3628, #8624, #18845, #13641, #809, #19152, #13787, #10987, #11626, #13477, #1111, #6433, #21821, #19328, #27015, #29536, #23693, #21189, #11306, #31387, #3485, #21515, #31727, #8801, #8462, #6280, #26670, #3783, #18656, #13952, #28857, #24174, #16156, #26384, #24654, #14791, #30030, #9599, #4616, #27165, #1784, #12464, #27342, #4770, #19823, #2276, #21990, #4462, #6933, #22677, #17132, #11977, #19504, #7427, #22173, #32383, #14444, #12278, #2099, #22492, #14944, #9442, #19660, #14285, #7125, #24836, #1954, #20159, #30358, #29852, #24988, #14636, #12126, #22323, #9789, #4269, #32707, #20010, #32535, #32879, #30205 ),
 ( #17321, #17625, #27515, #7277, #17468, #27667, #4117, #25156, #9946, #24480, #1598, #11787, #32220, #9287, #29697, #6778, #16966, #5438, #20663, #281, #28322, #17817, #15293, #3557, #17981, #28949, #10453, #26458, #12621, #28169, #30716, #13717, #7788, #2602, #10101, #31631, #25495, #12767, #5116, #2965, #10282, #22976, #5271, #31458, #6054, #15445, #882, #23918, #95, #33026, #23769, #18128, #21260, #20504, #25655, #8537, #30868, #27830, #18743, #2776, #1028, #7939, #16245, #4947, #12953, #25343, #23172, #11214, #15632, #25848, #13562, #11060, #22822, #21419, #8719, #15134, #20318, #2452, #30528, #7610, #28020, #16892, #24409, #1691, #1526, #16548, #32309, #4191, #9369, #31955, #12054, #21904, #3876, #22250, #1375, #6703, #14358, #14549, #21748, #26758, #11551, #24567, #24759, #14053, #24074, #11889, #9199, #22097, #29268, #24259, #19579, #11702, #18931, #29776, #9019, #4367, #32122, #6854, #29121, #16738, #16390 ) ),
 .UNSPECIFIED., .F., .F., .F. ) 
 B_SPLINE_SURFACE_WITH_KNOTS ( ( 2, 1, 2 ),
 ( 3, 2, 2, 2, 2, 2, 2, 2, 2, 2, 2, 2, 2, 2, 2, 2, 2, 2, 2, 2, 2, 2, 2, 2, 2, 2, 2, 2, 2, 2, 2, 2, 2, 2, 2, 2, 2, 2, 2, 2, 2, 2, 2, 2, 2, 2, 2, 2, 2, 2, 2, 2, 2, 2, 2, 2, 2, 2, 2, 2, 3 ),
 ( -0.01433874271596183303, 0.000000000000000000, 1.000000000000000000 ),
 ( 0.000000000000000000, 0.01562500000000000000, 0.03125000000000000000, 0.04687500000000000000, 0.06250000000000000000, 0.07812500000000000000, 0.09375000000000000000, 0.1093750000000000000, 0.1250000000000000000, 0.1406250000000000000, 0.1562500000000000000, 0.1718750000000000000, 0.1875000000000000000, 0.2031250000000000000, 0.2187500000000000000, 0.2343750000000000000, 0.2500000000000000000, 0.2656250000000000000, 0.2812500000000000000, 0.2968750000000000000, 0.3125000000000000000, 0.3281250000000000000, 0.3437500000000000000, 0.3593750000000000000, 0.3750000000000000000, 0.3906250000000000000, 0.4062500000000000000, 0.4218750000000000000, 0.4375000000000000000, 0.4531250000000000000, 0.4687500000000000000, 0.4843750000000000000, 0.5000000000000000000, 0.5156250000000000000, 0.5312500000000000000, 0.5468750000000000000, 0.5625000000000000000, 0.5781250000000000000, 0.5937500000000000000, 0.6093750000000000000, 0.6250000000000000000, 0.6406250000000000000, 0.6562500000000000000, 0.6718750000000000000, 0.6875000000000000000, 0.7031250000000000000, 0.7187500000000000000, 0.7343750000000000000, 0.7500000000000000000, 0.7656250000000000000, 0.7812500000000000000, 0.7968750000000000000, 0.8125000000000000000, 0.8281250000000000000, 0.8437500000000000000, 0.8593750000000000000, 0.8750000000000000000, 0.8906250000000000000, 0.9062500000000000000, 0.9218750000000000000, 0.9375000000000000000 ),
 .UNSPECIFIED. ) 
 GEOMETRIC_REPRESENTATION_ITEM ( )  RATIONAL_B_SPLINE_SURFACE ( (
 ( 1.000000000000000000, 0.9238795325112867385, 1.000000000000000000, 0.9238795325112867385, 1.000000000000000000, 0.9238795325112867385, 1.000000000000000000, 0.9238795325112867385, 1.000000000000000000, 0.9238795325112867385, 1.000000000000000000, 0.9238795325112867385, 1.000000000000000000, 0.9238795325112867385, 1.000000000000000000, 0.9238795325112867385, 1.000000000000000000, 0.9238795325112867385, 1.000000000000000000, 0.9238795325112867385, 1.000000000000000000, 0.9238795325112867385, 1.000000000000000000, 0.9238795325112867385, 1.000000000000000000, 0.9238795325112867385, 1.000000000000000000, 0.9238795325112867385, 1.000000000000000000, 0.9238795325112867385, 1.000000000000000000, 0.9238795325112867385, 1.000000000000000000, 0.9238795325112867385, 1.000000000000000000, 0.9238795325112867385, 1.000000000000000000, 0.9238795325112867385, 1.000000000000000000, 0.9238795325112867385, 1.000000000000000000, 0.9238795325112867385, 1.000000000000000000, 0.9238795325112867385, 1.000000000000000000, 0.9238795325112867385, 1.000000000000000000, 0.9238795325112867385, 1.000000000000000000, 0.9238795325112867385, 1.000000000000000000, 0.9238795325112867385, 1.000000000000000000, 0.9238795325112867385, 1.000000000000000000, 0.9238795325112867385, 1.000000000000000000, 0.9238795325112867385, 1.000000000000000000, 0.9238795325112867385, 1.000000000000000000, 0.9238795325112867385, 1.000000000000000000, 0.9238795325112867385, 1.000000000000000000, 0.9238795325112867385, 1.000000000000000000, 0.9238795325112867385, 1.000000000000000000, 0.9238795325112867385, 1.000000000000000000, 0.9238795325112867385, 1.000000000000000000, 0.9238795325112867385, 1.000000000000000000, 0.9238795325112867385, 1.000000000000000000, 0.9238795325112867385, 1.000000000000000000, 0.9238795325112867385, 1.000000000000000000, 0.9238795325112867385, 1.000000000000000000, 0.9238795325112867385, 1.000000000000000000, 0.9238795325112867385, 1.000000000000000000, 0.9238795325112867385, 1.000000000000000000, 0.9238795325112867385, 1.000000000000000000, 0.9238795325112867385, 1.000000000000000000, 0.9238795325112867385, 1.000000000000000000, 0.9238795325112867385, 1.000000000000000000, 0.9238795325112867385, 1.000000000000000000, 0.9238795325112867385, 1.000000000000000000, 0.9238795325112867385, 1.000000000000000000, 0.9238795325112867385, 1.000000000000000000, 0.9238795325112867385, 1.000000000000000000, 0.9238795325112867385, 1.000000000000000000, 0.9238795325112867385, 1.000000000000000000, 0.9238795325112867385, 1.000000000000000000, 0.9238795325112867385, 1.000000000000000000, 0.9238795325112867385, 1.000000000000000000, 0.9238795325112867385, 1.000000000000000000, 0.9238795325112867385, 1.000000000000000000),
 ( 1.000000000000000000, 0.9238795325112867385, 1.000000000000000000, 0.9238795325112867385, 1.000000000000000000, 0.9238795325112867385, 1.000000000000000000, 0.9238795325112867385, 1.000000000000000000, 0.9238795325112867385, 1.000000000000000000, 0.9238795325112867385, 1.000000000000000000, 0.9238795325112867385, 1.000000000000000000, 0.9238795325112867385, 1.000000000000000000, 0.9238795325112867385, 1.000000000000000000, 0.9238795325112867385, 1.000000000000000000, 0.9238795325112867385, 1.000000000000000000, 0.9238795325112867385, 1.000000000000000000, 0.9238795325112867385, 1.000000000000000000, 0.9238795325112867385, 1.000000000000000000, 0.9238795325112867385, 1.000000000000000000, 0.9238795325112867385, 1.000000000000000000, 0.9238795325112867385, 1.000000000000000000, 0.9238795325112867385, 1.000000000000000000, 0.9238795325112867385, 1.000000000000000000, 0.9238795325112867385, 1.000000000000000000, 0.9238795325112867385, 1.000000000000000000, 0.9238795325112867385, 1.000000000000000000, 0.9238795325112867385, 1.000000000000000000, 0.9238795325112867385, 1.000000000000000000, 0.9238795325112867385, 1.000000000000000000, 0.9238795325112867385, 1.000000000000000000, 0.9238795325112867385, 1.000000000000000000, 0.9238795325112867385, 1.000000000000000000, 0.9238795325112867385, 1.000000000000000000, 0.9238795325112867385, 1.000000000000000000, 0.9238795325112867385, 1.000000000000000000, 0.9238795325112867385, 1.000000000000000000, 0.9238795325112867385, 1.000000000000000000, 0.9238795325112867385, 1.000000000000000000, 0.9238795325112867385, 1.000000000000000000, 0.9238795325112867385, 1.000000000000000000, 0.9238795325112867385, 1.000000000000000000, 0.9238795325112867385, 1.000000000000000000, 0.9238795325112867385, 1.000000000000000000, 0.9238795325112867385, 1.000000000000000000, 0.9238795325112867385, 1.000000000000000000, 0.9238795325112867385, 1.000000000000000000, 0.9238795325112867385, 1.000000000000000000, 0.9238795325112867385, 1.000000000000000000, 0.9238795325112867385, 1.000000000000000000, 0.9238795325112867385, 1.000000000000000000, 0.9238795325112867385, 1.000000000000000000, 0.9238795325112867385, 1.000000000000000000, 0.9238795325112867385, 1.000000000000000000, 0.9238795325112867385, 1.000000000000000000, 0.9238795325112867385, 1.000000000000000000, 0.9238795325112867385, 1.000000000000000000, 0.9238795325112867385, 1.000000000000000000, 0.9238795325112867385, 1.000000000000000000, 0.9238795325112867385, 1.000000000000000000, 0.9238795325112867385, 1.000000000000000000, 0.9238795325112867385, 1.000000000000000000, 0.9238795325112867385, 1.000000000000000000, 0.9238795325112867385, 1.000000000000000000, 0.9238795325112867385, 1.000000000000000000),
 ( 1.000000000000000000, 0.9238795325112867385, 1.000000000000000000, 0.9238795325112867385, 1.000000000000000000, 0.9238795325112867385, 1.000000000000000000, 0.9238795325112867385, 1.000000000000000000, 0.9238795325112867385, 1.000000000000000000, 0.9238795325112867385, 1.000000000000000000, 0.9238795325112867385, 1.000000000000000000, 0.9238795325112867385, 1.000000000000000000, 0.9238795325112867385, 1.000000000000000000, 0.9238795325112867385, 1.000000000000000000, 0.9238795325112867385, 1.000000000000000000, 0.9238795325112867385, 1.000000000000000000, 0.9238795325112867385, 1.000000000000000000, 0.9238795325112867385, 1.000000000000000000, 0.9238795325112867385, 1.000000000000000000, 0.9238795325112867385, 1.000000000000000000, 0.9238795325112867385, 1.000000000000000000, 0.9238795325112867385, 1.000000000000000000, 0.9238795325112867385, 1.000000000000000000, 0.9238795325112867385, 1.000000000000000000, 0.9238795325112867385, 1.000000000000000000, 0.9238795325112867385, 1.000000000000000000, 0.9238795325112867385, 1.000000000000000000, 0.9238795325112867385, 1.000000000000000000, 0.9238795325112867385, 1.000000000000000000, 0.9238795325112867385, 1.000000000000000000, 0.9238795325112867385, 1.000000000000000000, 0.9238795325112867385, 1.000000000000000000, 0.9238795325112867385, 1.000000000000000000, 0.9238795325112867385, 1.000000000000000000, 0.9238795325112867385, 1.000000000000000000, 0.9238795325112867385, 1.000000000000000000, 0.9238795325112867385, 1.000000000000000000, 0.9238795325112867385, 1.000000000000000000, 0.9238795325112867385, 1.000000000000000000, 0.9238795325112867385, 1.000000000000000000, 0.9238795325112867385, 1.000000000000000000, 0.9238795325112867385, 1.000000000000000000, 0.9238795325112867385, 1.000000000000000000, 0.9238795325112867385, 1.000000000000000000, 0.9238795325112867385, 1.000000000000000000, 0.9238795325112867385, 1.000000000000000000, 0.9238795325112867385, 1.000000000000000000, 0.9238795325112867385, 1.000000000000000000, 0.9238795325112867385, 1.000000000000000000, 0.9238795325112867385, 1.000000000000000000, 0.9238795325112867385, 1.000000000000000000, 0.9238795325112867385, 1.000000000000000000, 0.9238795325112867385, 1.000000000000000000, 0.9238795325112867385, 1.000000000000000000, 0.9238795325112867385, 1.000000000000000000, 0.9238795325112867385, 1.000000000000000000, 0.9238795325112867385, 1.000000000000000000, 0.9238795325112867385, 1.000000000000000000, 0.9238795325112867385, 1.000000000000000000, 0.9238795325112867385, 1.000000000000000000, 0.9238795325112867385, 1.000000000000000000, 0.9238795325112867385, 1.000000000000000000, 0.9238795325112867385, 1.000000000000000000, 0.9238795325112867385, 1.000000000000000000) ) ) 
 REPRESENTATION_ITEM ( '' )  SURFACE ( )  );
#16225 = ORIENTED_EDGE ( 'NONE', *, *, #19577, .F. ) ;
#16224 = CARTESIAN_POINT ( 'NONE',  ( 0.6791198416090081791, -4.928602827912263784, 7.715582677070920603 ) ) ;
#16226 = AXIS2_PLACEMENT_3D ( 'NONE', #24694, #9472, #19532 ) ;
#16227 = AXIS2_PLACEMENT_3D ( 'NONE', #2986, #791, #18333 ) ;
#16228 = CARTESIAN_POINT ( 'NONE',  ( -7.587550801365593678, -3.521866450007987037, -0.3701630799359323931 ) ) ;
#16229 = DIRECTION ( 'NONE',  ( 0.000000000000000000, 0.000000000000000000, 1.000000000000000000 ) ) ;
#16230 = CARTESIAN_POINT ( 'NONE',  ( 5.388021529391686215, -18.36754117723517510, 1.500000000000001332 ) ) ;
#16231 = DIRECTION ( 'NONE',  ( -1.000000000000000000, 0.000000000000000000, -0.000000000000000000 ) ) ;
#16232 = EDGE_CURVE ( 'NONE', #12355, #25433, #4205, .T. ) ;
#16234 = VERTEX_POINT ( 'NONE', #28156 ) ;
#16233 = CARTESIAN_POINT ( 'NONE',  ( 0.000000000000000000, 0.000000000000000000, 0.000000000000000000 ) ) ;
#16235 = EDGE_CURVE ( 'NONE', #26576, #1557, #10441, .T. ) ;
#16236 = EDGE_CURVE ( 'NONE', #593, #21890, #4603, .T. ) ;
#16237 = LINE ( 'NONE', #18921, #22003 ) ;
#16238 = CARTESIAN_POINT ( 'NONE',  ( 23.11000000273118715, 1.573300977624590313, -1.942864903642426144 ) ) ;
#16239 = CC_DESIGN_APPROVAL ( #27393, ( #6102 ) ) ;
#16240 = CARTESIAN_POINT ( 'NONE',  ( -21.81615113095794101, 4.185543752813694063, 2.140960162089520669 ) ) ;
#16241 = CARTESIAN_POINT ( 'NONE',  ( 101.8538325601235783, -4.793708883847108915, -2.784893846770871040 ) ) ;
#16242 = DIRECTION ( 'NONE',  ( 0.000000000000000000, 0.000000000000000000, 1.000000000000000000 ) ) ;
#16243 = CARTESIAN_POINT ( 'NONE',  ( 14.23800746264082839, 22.11259878822726321, -1.491740999229417941 ) ) ;
#16244 = DIRECTION ( 'NONE',  ( 1.000000000000000000, 0.000000000000000000, 0.000000000000000000 ) ) ;
#16245 = CARTESIAN_POINT ( 'NONE',  ( -5.087550801365593678, -2.228590825266444586, -2.752080473201636401 ) ) ;
#16246 = ORIENTED_EDGE ( 'NONE', *, *, #14493, .T. ) ;
#16247 = AXIS2_PLACEMENT_3D ( 'NONE', #14128, #32206, #8613 ) ;
#16248 = DIRECTION ( 'NONE',  ( 1.000000000000000000, -0.000000000000000000, -0.000000000000000000 ) ) ;
#16249 = CARTESIAN_POINT ( 'NONE',  ( 84.65816297383780409, -6.961284151106491791, -0.07017451552783603164 ) ) ;
#16251 = DIRECTION ( 'NONE',  ( -1.000000000000000000, 8.574039729943018344E-17, -0.000000000000000000 ) ) ;
#16250 = CARTESIAN_POINT ( 'NONE',  ( 0.000000000000000000, 1.106368468154430129, 8.427689411260576691 ) ) ;
#16252 = ORIENTED_EDGE ( 'NONE', *, *, #31726, .T. ) ;
#16253 = CARTESIAN_POINT ( 'NONE',  ( -4.650050800000000706, -2.853674364686378695, -1.549418761218566809 ) ) ;
#16254 = VERTEX_POINT ( 'NONE', #12266 ) ;
#16255 = DIRECTION ( 'NONE',  ( -1.000000000000000000, 0.000000000000000000, 0.000000000000000000 ) ) ;
#16257 = ORIENTED_EDGE ( 'NONE', *, *, #8759, .F. ) ;
#16256 = CARTESIAN_POINT ( 'NONE',  ( 108.3926549169586764, 20.36461743673850577, -1.408140718819804738 ) ) ;
#16258 = EDGE_LOOP ( 'NONE', ( #6712, #10383, #11975, #30527, #16103, #12599, #4274, #5115 ) ) ;
#16259 = DIRECTION ( 'NONE',  ( 0.000000000000000000, 1.000000000000000000, 0.000000000000000000 ) ) ;
#16260 = CARTESIAN_POINT ( 'NONE',  ( 102.6421141555943706, -1.710335469228581484, -0.07017451552783579571 ) ) ;
#16261 = ADVANCED_FACE ( 'NONE', ( #17456 ), #17614, .F. ) ;
#16263 = VERTEX_POINT ( 'NONE', #6522 ) ;
#16262 = CARTESIAN_POINT ( 'NONE',  ( 107.8715728503188842, 17.46302688052359287, 2.802307197317986720 ) ) ;
#16264 = CARTESIAN_POINT ( 'NONE',  ( -2.096054051514731231, 1.210157370878028882, 1.500000000000000000 ) ) ;
#16265 = CARTESIAN_POINT ( 'NONE',  ( 34.31843563627104743, 19.51744974835125035, 1.818740222761737302 ) ) ;
#16266 = DIRECTION ( 'NONE',  ( 0.000000000000000000, 0.000000000000000000, 1.000000000000000000 ) ) ;
#16267 = CARTESIAN_POINT ( 'NONE',  ( 9.126991455997314873, -11.32614230997805471, -1.500000000000000000 ) ) ;
#16268 = CARTESIAN_POINT ( 'NONE',  ( 107.9476224718558939, -17.31513874123385932, -4.492091147515819394 ) ) ;
#16269 = DIRECTION ( 'NONE',  ( 1.000000000000000000, -8.574039729943018344E-17, -0.000000000000000000 ) ) ;
#16270 = VECTOR ( 'NONE', #29475, 999.9999999999998863 ) ;
#16271 = FACE_OUTER_BOUND ( 'NONE', #22985, .T. ) ;
#16272 = DIRECTION ( 'NONE',  ( 0.000000000000000000, 1.000000000000000000, 0.000000000000000000 ) ) ;
#16273 = DIRECTION ( 'NONE',  ( 0.000000000000000000, 0.000000000000000000, -1.000000000000000000 ) ) ;
#16274 = CARTESIAN_POINT ( 'NONE',  ( 2.913020537602753368, 0.09936728819756490694, 1.050862340634253211 ) ) ;
#16275 = VERTEX_POINT ( 'NONE', #18116 ) ;
#16276 = CARTESIAN_POINT ( 'NONE',  ( 107.8806307222008627, -16.35047421165092985, -1.384330804613826293 ) ) ;
#16277 = DIRECTION ( 'NONE',  ( -0.000000000000000000, 1.000000000000000000, 1.224646799147353207E-16 ) ) ;
#16278 = CARTESIAN_POINT ( 'NONE',  ( 2.357329895872533054, 10.75444571268654848, 1.335530315079542563 ) ) ;
#16279 = ORIENTED_EDGE ( 'NONE', *, *, #17906, .T. ) ;
#16280 = CARTESIAN_POINT ( 'NONE',  ( 25.44184412664977657, -2.526879277147909164, -0.9860087766846566959 ) ) ;
#16281 = EDGE_CURVE ( 'NONE', #1567, #32424, #16594, .T. ) ;
#16282 = APPLICATION_CONTEXT ( 'configuration controlled 3d designs of mechanical parts and assemblies' ) ;
#16283 = DIRECTION ( 'NONE',  ( 1.000000000000000000, 0.000000000000000000, 0.000000000000000000 ) ) ;
#16284 = ORIENTED_EDGE ( 'NONE', *, *, #27024, .F. ) ;
#16285 = CARTESIAN_POINT ( 'NONE',  ( 15.98710106916323781, -15.99254912437086240, -1.500000000000000222 ) ) ;
#16286 = DIRECTION ( 'NONE',  ( 0.000000000000000000, 0.000000000000000000, 1.000000000000000000 ) ) ;
#16287 = VERTEX_POINT ( 'NONE', #10937 ) ;
#16288 = EDGE_LOOP ( 'NONE', ( #4440, #24905, #2581, #8926 ) ) ;
#16289 = CARTESIAN_POINT ( 'NONE',  ( 5.377543748152549874, 2.741043480755029016, -7.530955069117485579 ) ) ;
#16290 = EDGE_CURVE ( 'NONE', #19663, #25011, #13591, .T. ) ;
#16291 = COORDINATED_UNIVERSAL_TIME_OFFSET ( 0, 0, .AHEAD. ) ;
#16293 = ORIENTED_EDGE ( 'NONE', *, *, #17517, .F. ) ;
#16292 = CARTESIAN_POINT ( 'NONE',  ( 0.2409471776115470198, 0.000000000000000000, 5.412820279296879811 ) ) ;
#16294 = ORIENTED_EDGE ( 'NONE', *, *, #9279, .F. ) ;
#16295 = LINE ( 'NONE', #16122, #10744 ) ;
#16296 = VERTEX_POINT ( 'NONE', #13256 ) ;
#16297 = DIRECTION ( 'NONE',  ( 0.000000000000000000, 1.000000000000000000, 0.000000000000000000 ) ) ;
#16299 = EDGE_LOOP ( 'NONE', ( #29719, #18896, #18366, #18422 ) ) ;
#16298 = CARTESIAN_POINT ( 'NONE',  ( 3.249999999999999556, 0.4999240074894433228, 8.734705317681628500 ) ) ;
#16300 = CARTESIAN_POINT ( 'NONE',  ( 7.249760686538667009, -2.789499415801756586E-14, 8.014274990069656823 ) ) ;
#16301 = DIRECTION ( 'NONE',  ( -1.000000000000000000, 0.000000000000000000, 0.000000000000000000 ) ) ;
#16302 = EDGE_CURVE ( 'NONE', #22652, #11, #6223, .T. ) ;
#16303 = FACE_OUTER_BOUND ( 'NONE', #30690, .T. ) ;
#16304 = EDGE_CURVE ( 'NONE', #19070, #20542, #26898, .T. ) ;
#16305 = CARTESIAN_POINT ( 'NONE',  ( 3.020080204141757374, 4.831795131260099296, -7.542713057980071412 ) ) ;
#16306 = CARTESIAN_POINT ( 'NONE',  ( 12.44989959798868817, 18.00000000000000355, 13.00000000000004441 ) ) ;
#16307 = B_SPLINE_CURVE_WITH_KNOTS ( 'NONE', 3,
 ( #13276, #31695, #23482, #8290, #18484, #5773 ),
 .UNSPECIFIED., .F., .F.,
 ( 4, 2, 4 ),
 ( 0.009541643435016143593, 0.5047708217175082002, 1.000000000000000000 ),
 .UNSPECIFIED. ) ;
#16308 = CARTESIAN_POINT ( 'NONE',  ( -31.35000000000000142, -10.96966150227469328, 4.500000000000000888 ) ) ;
#16309 = CARTESIAN_POINT ( 'NONE',  ( 41.35712849199997265, -8.497574858407940468, -0.4367667074098299795 ) ) ;
#16310 = LINE ( 'NONE', #32021, #1861 ) ;
#16311 = EDGE_CURVE ( 'NONE', #3200, #17057, #26322, .T. ) ;
#16312 = PLANE ( 'NONE',  #19279 ) ;
#16313 = CARTESIAN_POINT ( 'NONE',  ( 23.12748563068209151, -21.92617699668438291, 1.175810100957690008 ) ) ;
#16314 = CARTESIAN_POINT ( 'NONE',  ( 0.7632845268398871230, -6.772677083992345359, -5.538577986808975062 ) ) ;
#16315 = CARTESIAN_POINT ( 'NONE',  ( 0.000000000000000000, -1.975651141462316351, 10.82112760146735297 ) ) ;
#16316 = CARTESIAN_POINT ( 'NONE',  ( 18.51491971917340607, -8.599446730134173933, 0.07017451552781736601 ) ) ;
#16317 = CARTESIAN_POINT ( 'NONE',  ( -3.962550801365593234, 2.752080473201636845, -2.228590825266444142 ) ) ;
#16318 = ORIENTED_EDGE ( 'NONE', *, *, #2209, .F. ) ;
#16319 = EDGE_CURVE ( 'NONE', #12410, #979, #909, .T. ) ;
#16320 = CARTESIAN_POINT ( 'NONE',  ( -7.100050799999999995, -2.983565686104819648, -0.3135853898029605791 ) ) ;
#16321 = B_SPLINE_CURVE_WITH_KNOTS ( 'NONE', 3,
 ( #14121, #15959, #1433, #23668, #11609, #21804, #789, #32011, #5782, #27651 ),
 .UNSPECIFIED., .F., .F.,
 ( 4, 2, 2, 2, 4 ),
 ( 3.032460776716650747E-07, 0.0005479053915603972853, 0.001095507537043122767, 0.001643109682525848358, 0.002190711828008574166 ),
 .UNSPECIFIED. ) ;
#16322 = LINE ( 'NONE', #21336, #19949 ) ;
#16323 = CYLINDRICAL_SURFACE ( 'NONE', #14040, 8.749000000000002331 ) ;
#16324 = CARTESIAN_POINT ( 'NONE',  ( 6.669411210322924610, -6.378078458905314108, 1.500000000000000000 ) ) ;
#16325 = VERTEX_POINT ( 'NONE', #24399 ) ;
#16326 = CARTESIAN_POINT ( 'NONE',  ( 28.72212596679750263, -4.487363129039004583, -2.184956778818292200 ) ) ;
#16327 = VERTEX_POINT ( 'NONE', #25993 ) ;
#16328 = CARTESIAN_POINT ( 'NONE',  ( 0.9576657675042646867, -9.536988708453836949, 1.767396803601621214 ) ) ;
#16329 = PERSON_AND_ORGANIZATION_ROLE ( 'design_owner' ) ;
#16330 = CARTESIAN_POINT ( 'NONE',  ( 40.88155443523169197, -6.447799953524727457, 4.312042181580753031 ) ) ;
#16331 = CARTESIAN_POINT ( 'NONE',  ( 16.73992168104834377, 12.07607160919255840, -1.050000000000000266 ) ) ;
#16332 = CARTESIAN_POINT ( 'NONE',  ( 2.864530875629062390, -0.6595692664038241837, 9.539603485476151334 ) ) ;
#16333 = CARTESIAN_POINT ( 'NONE',  ( 2.274274201625327230, 5.222868219166857173, 9.680994141368788775 ) ) ;
#16334 = ORIENTED_EDGE ( 'NONE', *, *, #7146, .T. ) ;
#16335 = ADVANCED_FACE ( 'NONE', ( #21739 ), #31947, .T. ) ;
#16336 = CARTESIAN_POINT ( 'NONE',  ( 0.5704039292222262691, 6.124150562935539277, 7.316743080999650317 ) ) ;
#16337 = EDGE_CURVE ( 'NONE', #18033, #20676, #10206, .T. ) ;
#16338 = DIRECTION ( 'NONE',  ( 1.000000000000000000, 0.000000000000000000, 0.000000000000000000 ) ) ;
#16339 = CARTESIAN_POINT ( 'NONE',  ( 1.624999999999999778, 9.680994141368847394, -5.222868219166750592 ) ) ;
#16341 = ORIENTED_EDGE ( 'NONE', *, *, #30202, .T. ) ;
#16340 = DIRECTION ( 'NONE',  ( -1.000000000000000000, -0.000000000000000000, -0.000000000000000000 ) ) ;
#16342 = CARTESIAN_POINT ( 'NONE',  ( -4.262550801365594388, -3.521866450007987037, -0.3701630799359323931 ) ) ;
#16343 = DIRECTION ( 'NONE',  ( -7.770718973608988517E-17, -0.9063077870366522681, 0.4226182617406944453 ) ) ;
#16344 = DIRECTION ( 'NONE',  ( -1.000000000000000000, 0.000000000000000000, 0.000000000000000000 ) ) ;
#16345 = VERTEX_POINT ( 'NONE', #18463 ) ;
#16346 = B_SPLINE_CURVE_WITH_KNOTS ( 'NONE', 3,
 ( #8498, #10862, #31586, #5828, #8839, #23882 ),
 .UNSPECIFIED., .F., .F.,
 ( 4, 2, 4 ),
 ( -1.393633244722569653E-05, 0.0003803243175954409668, 0.0007745849676381076979 ),
 .UNSPECIFIED. ) ;
#16347 = CARTESIAN_POINT ( 'NONE',  ( -3.122314033877847442E-16, -3.641590349731908649, -3.055657119358837992 ) ) ;
#16348 = CARTESIAN_POINT ( 'NONE',  ( 0.7212197813410882175, -3.259817272377325992, 8.337493976400230267 ) ) ;
#16349 = DIRECTION ( 'NONE',  ( -3.028893931825485746E-17, -8.673617379884035472E-16, -1.000000000000000000 ) ) ;
#16350 = CARTESIAN_POINT ( 'NONE',  ( 73.45519860865672968, -21.36028973287419674, 4.522129901861159595 ) ) ;
#16351 = DIRECTION ( 'NONE',  ( -1.000000000000000000, 0.000000000000000000, 0.000000000000000000 ) ) ;
#16352 = VERTEX_POINT ( 'NONE', #25832 ) ;
#16353 = ADVANCED_FACE ( 'NONE', ( #2955 ), #29427, .T. ) ;
#16354 = CARTESIAN_POINT ( 'NONE',  ( 10.56870887191539587, 4.616489984850558059, -1.946309384392544972 ) ) ;
#16355 = CC_DESIGN_PERSON_AND_ORGANIZATION_ASSIGNMENT ( #17872, #20058, ( #22028 ) ) ;
#16356 = DIRECTION ( 'NONE',  ( 1.000000000000000000, -0.000000000000000000, -0.000000000000000000 ) ) ;
#16357 = CARTESIAN_POINT ( 'NONE',  ( -2.887550801365593500, -2.752080473201636845, 2.228590825266444586 ) ) ;
#16358 = CARTESIAN_POINT ( 'NONE',  ( 3.569153896158649086, -0.01695480042954932223, -1.144240241240434441 ) ) ;
#16359 = CARTESIAN_POINT ( 'NONE',  ( 7.077711312404847644E-17, 0.8254815157535873027, -4.681538312723508177 ) ) ;
#16360 = ORIENTED_EDGE ( 'NONE', *, *, #25747, .T. ) ;
#16361 = CARTESIAN_POINT ( 'NONE',  ( -15.12340757463330476, -27.93932300454937590, -1.000000000000000000 ) ) ;
#16362 = VERTEX_POINT ( 'NONE', #31338 ) ;
#16363 = CALENDAR_DATE ( 2026, 6, 10 ) ;
#16364 = CARTESIAN_POINT ( 'NONE',  ( 40.88398291294785025, -6.895006614273913925, 3.995970210903281750 ) ) ;
#16365 = ADVANCED_FACE ( 'NONE', ( #8417 ), #18610, .F. ) ;
#16366 = DIRECTION ( 'NONE',  ( 0.000000000000000000, 0.000000000000000000, 1.000000000000000000 ) ) ;
#16367 = ORIENTED_EDGE ( 'NONE', *, *, #20703, .F. ) ;
#16368 = FACE_OUTER_BOUND ( 'NONE', #20509, .T. ) ;
#16369 = ORIENTED_EDGE ( 'NONE', *, *, #18370, .T. ) ;
#16370 = EDGE_LOOP ( 'NONE', ( #17418, #16114, #24538, #22717 ) ) ;
#16371 = LINE ( 'NONE', #8515, #7508 ) ;
#16372 = CARTESIAN_POINT ( 'NONE',  ( -5.962550801365593678, -2.752080473201636845, 2.228590825266444586 ) ) ;
#16373 = CARTESIAN_POINT ( 'NONE',  ( 22.79750000000000654, 0.7685399846772009713, -2.594547506269381909 ) ) ;
#16374 = CARTESIAN_POINT ( 'NONE',  ( 0.2073616445840893718, -5.485889181658371250, -1.769987010377963355 ) ) ;
#16376 = VERTEX_POINT ( 'NONE', #1518 ) ;
#16375 = CARTESIAN_POINT ( 'NONE',  ( 3.499999999999999556, -6.200809695932780308, 0.7745709230444962623 ) ) ;
#16377 = CARTESIAN_POINT ( 'NONE',  ( -6.787550801365593856, -3.521866450007987037, -0.3701630799359323931 ) ) ;
#16378 = DIRECTION ( 'NONE',  ( -1.000000000000000000, 0.000000000000000000, 0.000000000000000000 ) ) ;
#16379 = CYLINDRICAL_SURFACE ( 'NONE', #27881, 4.000000000000001776 ) ;
#16380 = LINE ( 'NONE', #26100, #29561 ) ;
#16382 = ORIENTED_EDGE ( 'NONE', *, *, #16546, .T. ) ;
#16381 = PLANE ( 'NONE',  #581 ) ;
#16383 = CARTESIAN_POINT ( 'NONE',  ( 22.48500000273118715, 0.2613211581691317065, 2.486304738420681559 ) ) ;
#16384 = EDGE_CURVE ( 'NONE', #17287, #32109, #7534, .T. ) ;
#16385 = CYLINDRICAL_SURFACE ( 'NONE', #5483, 5.010000000000000675 ) ;
#16386 = FACE_OUTER_BOUND ( 'NONE', #29129, .T. ) ;
#16387 = CARTESIAN_POINT ( 'NONE',  ( -3.562847368662853231, -10.36282323065911370, -1.499999999999920286 ) ) ;
#16388 = CARTESIAN_POINT ( 'NONE',  ( 0.000000000000000000, 0.000000000000000000, 0.000000000000000000 ) ) ;
#16389 = CARTESIAN_POINT ( 'NONE',  ( 9.301477900249441433, 0.2449194893134349904, 1.049999999999945643 ) ) ;
#16390 = CARTESIAN_POINT ( 'NONE',  ( -2.187550801365593767, -0.3701630799359326152, 3.521866450007987037 ) ) ;
#16391 = ORIENTED_EDGE ( 'NONE', *, *, #10247, .T. ) ;
#16392 = CARTESIAN_POINT ( 'NONE',  ( 20.58436699794813052, -21.58689779341593251, 1.578270943419565420 ) ) ;
#16393 = DIRECTION ( 'NONE',  ( -0.000000000000000000, 0.2588190451025172423, 0.9659258262890692004 ) ) ;
#16395 = CARTESIAN_POINT ( 'NONE',  ( 5.377543748152548098, -6.940565734314625423, 4.007137495034787555 ) ) ;
#16394 = CARTESIAN_POINT ( 'NONE',  ( -1.082681991931091270, 0.000000000000000000, 4.629213727441584325 ) ) ;
#16396 = EDGE_CURVE ( 'NONE', #11936, #15394, #18294, .T. ) ;
#16397 = VERTEX_POINT ( 'NONE', #22744 ) ;
#16398 = EDGE_CURVE ( 'NONE', #7325, #19201, #16168, .T. ) ;
#16399 =( BOUNDED_SURFACE ( )  B_SPLINE_SURFACE ( 3, 2, ( 
 ( #28897, #5826, #11351 ),
 ( #6170, #16504, #29084 ),
 ( #18888, #989, #11170 ),
 ( #26420, #26712, #844 ),
 ( #31582, #3522, #24371 ),
 ( #4005, #11021, #3353 ),
 ( #13518, #6316, #14172 ),
 ( #24027, #1488, #11664 ) ),
 .UNSPECIFIED., .F., .F., .F. ) 
 B_SPLINE_SURFACE_WITH_KNOTS ( ( 4, 2, 2, 4 ),
 ( 3, 3 ),
 ( 0.000000000000000000, 0.001031706651898130385, 0.002063413303796260770, 0.004126826607592521540 ),
 ( 0.000000000000000000, 1.000000000000000000 ),
 .UNSPECIFIED. ) 
 GEOMETRIC_REPRESENTATION_ITEM ( )  RATIONAL_B_SPLINE_SURFACE ( (
 ( 1.000000000000000000, 0.7660444431189777914, 1.000000000000000000),
 ( 1.000000000000000000, 0.8085210103976964158, 1.000000000000000000),
 ( 1.000000000000000000, 0.8435318601836696573, 1.000000000000000000),
 ( 1.000000000000000000, 0.9022997401206489521, 1.000000000000000000),
 ( 1.000000000000000000, 0.9260936007027089634, 1.000000000000000000),
 ( 1.000000000000000000, 0.9823303353968980689, 1.000000000000000000),
 ( 1.000000000000000000, 0.9997933690882994107, 1.000000000000000000),
 ( 1.000000000000000000, 1.000000000000000000, 1.000000000000000000) ) ) 
 REPRESENTATION_ITEM ( '' )  SURFACE ( )  );
#16400 = CARTESIAN_POINT ( 'NONE',  ( 0.000000000000000000, 3.771202944355708020, 4.982773259188384429 ) ) ;
#16401 = ORIENTED_EDGE ( 'NONE', *, *, #1944, .F. ) ;
#16402 = DIRECTION ( 'NONE',  ( 0.000000000000000000, 0.000000000000000000, 1.000000000000000000 ) ) ;
#16403 = EDGE_CURVE ( 'NONE', #3662, #10864, #11805, .T. ) ;
#16405 = ORIENTED_EDGE ( 'NONE', *, *, #32875, .F. ) ;
#16404 = CARTESIAN_POINT ( 'NONE',  ( 102.3440491116951563, -2.855879258563742251, -3.995006639038339191 ) ) ;
#16406 = VERTEX_POINT ( 'NONE', #4841 ) ;
#16407 = DIRECTION ( 'NONE',  ( 1.000000000000000000, -8.574039729943018344E-17, -0.000000000000000000 ) ) ;
#16408 = CARTESIAN_POINT ( 'NONE',  ( 10.52034268205830259, 3.672404558090037963, 3.407865132560194077 ) ) ;
#16410 = ORIENTED_EDGE ( 'NONE', *, *, #9879, .F. ) ;
#16409 = CARTESIAN_POINT ( 'NONE',  ( 107.8039775135429750, 17.08662937350926825, 1.995979254009180082 ) ) ;
#16411 = DIRECTION ( 'NONE',  ( -0.8660254037844399289, 0.4999999999999978906, 0.000000000000000000 ) ) ;
#16412 = CARTESIAN_POINT ( 'NONE',  ( 12.23764924856644143, -13.51220073293806223, 1.000000000000000000 ) ) ;
#16413 = B_SPLINE_CURVE_WITH_KNOTS ( 'NONE', 3,
 ( #25720, #7678, #5506, #7330 ),
 .UNSPECIFIED., .F., .F.,
 ( 4, 4 ),
 ( 3.740497495074990297E-18, 0.0002608162019139872436 ),
 .UNSPECIFIED. ) ;
#16414 = CYLINDRICAL_SURFACE ( 'NONE', #24087, 0.5000000000000007772 ) ;
#16415 = CARTESIAN_POINT ( 'NONE',  ( 8.486535498731882399, -10.66169397748177161, -1.000000000000000000 ) ) ;
#16416 = CARTESIAN_POINT ( 'NONE',  ( -3.007304909706596696, -1.062355717592093463, -3.000000000000000888 ) ) ;
#16417 = PLANE ( 'NONE',  #31712 ) ;
#16418 = CARTESIAN_POINT ( 'NONE',  ( 2.661997781067684699, 3.981025027156612772, -9.315861390595046032 ) ) ;
#16419 = DIRECTION ( 'NONE',  ( 0.000000000000000000, -0.9271838545667856479, -0.3746065934159163446 ) ) ;
#16420 = CARTESIAN_POINT ( 'NONE',  ( 17.97422212134408781, -19.86246923125032282, 4.522129901861158707 ) ) ;
#16421 = CARTESIAN_POINT ( 'NONE',  ( 0.000000000000000000, 6.704570150427012543, -2.172265885002588437 ) ) ;
#16422 = ORIENTED_EDGE ( 'NONE', *, *, #17575, .F. ) ;
#16423 = CARTESIAN_POINT ( 'NONE',  ( -6.200050800000000528, -1.887961173149512062, -2.331437884370912261 ) ) ;
#16424 = LINE ( 'NONE', #13747, #7061 ) ;
#16425 = FACE_OUTER_BOUND ( 'NONE', #31010, .T. ) ;
#16426 = EDGE_LOOP ( 'NONE', ( #19846, #4627, #6320, #8433 ) ) ;
#16427 = CARTESIAN_POINT ( 'NONE',  ( 0.000000000000000000, 0.000000000000000000, 0.000000000000000000 ) ) ;
#16428 = CARTESIAN_POINT ( 'NONE',  ( 78.40736801748178664, 24.56822898102832653, -4.612695725900423760 ) ) ;
#16429 = ORIENTED_EDGE ( 'NONE', *, *, #1022, .F. ) ;
#16430 = CARTESIAN_POINT ( 'NONE',  ( 5.612974441954677651, 6.420536856480007160, -5.126870824538697136 ) ) ;
#16431 = CARTESIAN_POINT ( 'NONE',  ( 0.000000000000000000, 0.000000000000000000, 0.000000000000000000 ) ) ;
#16432 = EDGE_CURVE ( 'NONE', #18655, #7759, #7836, .T. ) ;
#16433 = EDGE_CURVE ( 'NONE', #31391, #9461, #30517, .T. ) ;
#16434 = ORIENTED_EDGE ( 'NONE', *, *, #21763, .F. ) ;
#16435 = EDGE_CURVE ( 'NONE', #18983, #27498, #31579, .T. ) ;
#16436 = ORIENTED_EDGE ( 'NONE', *, *, #17503, .T. ) ;
#16437 = CARTESIAN_POINT ( 'NONE',  ( 24.55820472632857232, -17.37661330403883397, -1.293157874817485231 ) ) ;
#16439 = ORIENTED_EDGE ( 'NONE', *, *, #32453, .F. ) ;
#16438 = CARTESIAN_POINT ( 'NONE',  ( 10.57125986779756843, 4.971152295393300946, 0.6226916219172224931 ) ) ;
#16440 = EDGE_LOOP ( 'NONE', ( #5821, #27621, #18447 ) ) ;
#16441 = DIRECTION ( 'NONE',  ( -1.000000000000000000, 0.000000000000000000, 0.000000000000000000 ) ) ;
#16442 = VERTEX_POINT ( 'NONE', #17031 ) ;
#16443 = CARTESIAN_POINT ( 'NONE',  ( 0.000000000000000000, -5.222868219166785231, -9.680994141368824302 ) ) ;
#16444 = CARTESIAN_POINT ( 'NONE',  ( 10.00000000000000178, -8.574039729943018837E-16, 0.000000000000000000 ) ) ;
#16446 = EDGE_LOOP ( 'NONE', ( #4432, #7444, #19298, #30684 ) ) ;
#16445 = CARTESIAN_POINT ( 'NONE',  ( 102.2233072702345282, -1.127920370132907024, -0.4367666012504502482 ) ) ;
#16447 = DIRECTION ( 'NONE',  ( 0.000000000000000000, 0.000000000000000000, 1.000000000000000000 ) ) ;
#16448 = CARTESIAN_POINT ( 'NONE',  ( 56.97280603064898941, -277.2763395528616002, 0.4463807625373348298 ) ) ;
#16449 = CARTESIAN_POINT ( 'NONE',  ( -56.77604778592783674, 0.4588835684945939963, 1.891358768140224633 ) ) ;
#16450 = CARTESIAN_POINT ( 'NONE',  ( -50.81000000000000227, -10.96999999999998643, 8.628141679950115162 ) ) ;
#16451 = CARTESIAN_POINT ( 'NONE',  ( 107.5622803136338490, -18.99091296950214769, 4.502146529677950149 ) ) ;
#16452 = DIRECTION ( 'NONE',  ( 0.000000000000000000, 0.4067366430758009299, -0.9135454576426005335 ) ) ;
#16453 = CARTESIAN_POINT ( 'NONE',  ( 41.35698357845723905, -8.446179956401207889, -0.8105618903102438377 ) ) ;
#16454 = CARTESIAN_POINT ( 'NONE',  ( -15.12340757463330654, -27.93932300454937590, -1.000000000000000000 ) ) ;
#16455 = CARTESIAN_POINT ( 'NONE',  ( 6.883866557622098092, 7.943335131955005401, 3.625395379390111916 ) ) ;
#16456 = DIRECTION ( 'NONE',  ( -1.000000000000000000, 0.000000000000000000, 0.000000000000000000 ) ) ;
#16457 = CARTESIAN_POINT ( 'NONE',  ( 107.9638161812112003, 20.82655351785253472, -1.472934137033776736 ) ) ;
#16458 = CARTESIAN_POINT ( 'NONE',  ( 23.86000000273118715, -1.942864903642428587, -1.573300977624592756 ) ) ;
#16459 = ADVANCED_FACE ( 'NONE', ( #17225 ), #24906, .T. ) ;
#16460 = DIRECTION ( 'NONE',  ( 1.000000000000000000, -0.000000000000000000, -0.000000000000000000 ) ) ;
#16461 = CARTESIAN_POINT ( 'NONE',  ( -7.300050802731188782, -1.549418761218565477, 2.853674364686380471 ) ) ;
#16462 = VERTEX_POINT ( 'NONE', #14350 ) ;
#16463 = CARTESIAN_POINT ( 'NONE',  ( -7.450050800000001416, 2.853674364686379583, 1.549418761218565921 ) ) ;
#16464 = EDGE_CURVE ( 'NONE', #20076, #15630, #9681, .T. ) ;
#16465 = CARTESIAN_POINT ( 'NONE',  ( 107.5818156268159669, -17.35116702072363637, 4.522076865625765940 ) ) ;
#16466 = EDGE_CURVE ( 'NONE', #10433, #32858, #20885, .T. ) ;
#16467 = CARTESIAN_POINT ( 'NONE',  ( 3.063284526839887167, 0.000000000000000000, 0.000000000000000000 ) ) ;
#16468 = CARTESIAN_POINT ( 'NONE',  ( 7.192400643299417418, -7.644771086296574758, 1.000000000000000000 ) ) ;
#16469 = ORIENTED_EDGE ( 'NONE', *, *, #7132, .F. ) ;
#16470 = CARTESIAN_POINT ( 'NONE',  ( -7.150050800000000706, -3.113457007523259268, 0.9222479816126455399 ) ) ;
#16472 = EDGE_LOOP ( 'NONE', ( #20126, #30173, #30274 ) ) ;
#16471 = B_SPLINE_CURVE_WITH_KNOTS ( 'NONE', 3,
 ( #31752, #29220, #6305, #13988, #24205, #26699, #20187, #2311 ),
 .UNSPECIFIED., .F., .F.,
 ( 4, 2, 2, 4 ),
 ( 2.049880227769566238E-07, 0.001261138121172460493, 0.001891604687747302106, 0.002522071254322143935 ),
 .UNSPECIFIED. ) ;
#16473 = CARTESIAN_POINT ( 'NONE',  ( 0.3472807118842683449, -7.723390615030998774, 1.499999999999999778 ) ) ;
#16474 = DATE_AND_TIME ( #6289, #16212 ) ;
#16475 = EDGE_CURVE ( 'NONE', #32977, #23825, #25785, .T. ) ;
#16476 = ORIENTED_EDGE ( 'NONE', *, *, #11058, .F. ) ;
#16477 = CARTESIAN_POINT ( 'NONE',  ( 69.02444692756159839, -5.195103839446206351, 4.215290682826566382 ) ) ;
#16478 = CARTESIAN_POINT ( 'NONE',  ( 15.47903418055154390, 10.33214376877492846, -1.050000000000000044 ) ) ;
#16479 = CARTESIAN_POINT ( 'NONE',  ( 28.68776846592777829, -5.841437261377540047, -4.215290389454363407 ) ) ;
#16480 = DIRECTION ( 'NONE',  ( 0.000000000000000000, 1.000000000000000000, 0.000000000000000000 ) ) ;
#16481 = CARTESIAN_POINT ( 'NONE',  ( 7.249760686538667009, -2.741043480754977946, 7.530955069117504230 ) ) ;
#16482 = ORIENTED_EDGE ( 'NONE', *, *, #14434, .F. ) ;
#16483 = ADVANCED_FACE ( 'NONE', ( #9683 ), #32608, .T. ) ;
#16484 = CARTESIAN_POINT ( 'NONE',  ( 10.56870887191539587, -4.467071865485462645, -1.625881193364742572 ) ) ;
#16485 = CARTESIAN_POINT ( 'NONE',  ( 23.24965665534714176, -21.93932291342295215, -1.034606501595533024 ) ) ;
#16486 = CARTESIAN_POINT ( 'NONE',  ( 15.82680059085170221, 20.06867288585792863, 4.148259000770580407 ) ) ;
#16487 = EDGE_CURVE ( 'NONE', #19582, #29588, #24608, .T. ) ;
#16489 = ORIENTED_EDGE ( 'NONE', *, *, #12893, .F. ) ;
#16488 = CARTESIAN_POINT ( 'NONE',  ( 4.749760686538667009, -7.892520144992426268, -1.391664247347309535 ) ) ;
#16490 = CARTESIAN_POINT ( 'NONE',  ( 18.51491971917340607, -8.599446730134173933, -0.07017451552781736601 ) ) ;
#16491 = DIRECTION ( 'NONE',  ( 1.000000000000000000, 0.000000000000000000, 0.000000000000000000 ) ) ;
#16492 = LINE ( 'NONE', #19181, #84 ) ;
#16493 = LINE ( 'NONE', #19366, #11964 ) ;
#16494 = EDGE_CURVE ( 'NONE', #23747, #10694, #25566, .T. ) ;
#16495 = CARTESIAN_POINT ( 'NONE',  ( 7.249760686538667009, 7.892520144992453801, -1.391664247347147443 ) ) ;
#16496 = DIRECTION ( 'NONE',  ( -1.000000000000000000, 0.000000000000000000, 0.000000000000000000 ) ) ;
#16497 = CARTESIAN_POINT ( 'NONE',  ( 42.13509523493340936, -21.36880892310108493, 5.485967528433933538 ) ) ;
#16498 = ORIENTED_EDGE ( 'NONE', *, *, #25504, .T. ) ;
#16499 = EDGE_CURVE ( 'NONE', #9377, #18687, #32110, .T. ) ;
#16500 = CARTESIAN_POINT ( 'NONE',  ( -34.98193025661426248, 0.5174497483512504603, 3.000000000000004441 ) ) ;
#16501 = ORIENTED_EDGE ( 'NONE', *, *, #31484, .T. ) ;
#16502 = DIRECTION ( 'NONE',  ( 0.000000000000000000, -0.9659258262890716429, 0.2588190451025081940 ) ) ;
#16503 = CONICAL_SURFACE ( 'NONE', #11169, 11.99878165403819352, 0.03490658503988666728 ) ;
#16504 = CARTESIAN_POINT ( 'NONE',  ( -57.39838859230419388, -3.103981716530615387, 5.547394276431782956 ) ) ;
#16505 = CARTESIAN_POINT ( 'NONE',  ( -3.737550801365593589, -1.828967928396026732, 3.368539882008728004 ) ) ;
#16506 = EDGE_CURVE ( 'NONE', #292, #29424, #14992, .T. ) ;
#16507 = DIRECTION ( 'NONE',  ( 0.000000000000000000, 0.9945218953682734009, -0.1045284632676536235 ) ) ;
#16508 = ORIENTED_EDGE ( 'NONE', *, *, #2458, .T. ) ;
#16509 = DIRECTION ( 'NONE',  ( 0.000000000000000000, 0.000000000000000000, 1.000000000000000000 ) ) ;
#16510 = EDGE_CURVE ( 'NONE', #12775, #31261, #2762, .T. ) ;
#16511 = ORIENTED_EDGE ( 'NONE', *, *, #29137, .T. ) ;
#16512 = APPROVAL_ROLE ( '' ) ;
#16513 = CARTESIAN_POINT ( 'NONE',  ( 28.66414223207782896, -6.763717812351308645, 3.995970707797161570 ) ) ;
#16514 = ADVANCED_FACE ( 'NONE', ( #17894 ), #30427, .T. ) ;
#16515 = VECTOR ( 'NONE', #20576, 1000.000000000000227 ) ;
#16516 = CARTESIAN_POINT ( 'NONE',  ( 7.211599578357735574, -7.804913758300354054, -1.000000000000000222 ) ) ;
#16517 = AXIS2_PLACEMENT_3D ( 'NONE', #7604, #27660, #4940 ) ;
#16518 = ORIENTED_EDGE ( 'NONE', *, *, #3103, .T. ) ;
#16519 = CARTESIAN_POINT ( 'NONE',  ( 5.699736881468946414, 11.99440202994180993, 2.572806452144735356 ) ) ;
#16520 = ORIENTED_EDGE ( 'NONE', *, *, #10654, .T. ) ;
#16521 = ORIENTED_EDGE ( 'NONE', *, *, #27133, .T. ) ;
#16522 = DIRECTION ( 'NONE',  ( 0.000000000000000000, 1.000000000000000000, 0.000000000000000000 ) ) ;
#16523 = CARTESIAN_POINT ( 'NONE',  ( -4.612550801365594921, 3.368539882008727115, 1.828967928396027176 ) ) ;
#16524 = CARTESIAN_POINT ( 'NONE',  ( 24.73499999999999943, -0.2613211581691358698, -2.486304738420681559 ) ) ;
#16525 = ADVANCED_FACE ( 'NONE', ( #5525 ), #14272, .T. ) ;
#16526 = CARTESIAN_POINT ( 'NONE',  ( 2.053744806908957887, -0.9196371613258790267, -1.500000000000420552 ) ) ;
#16527 = AXIS2_PLACEMENT_3D ( 'NONE', #12395, #9394, #17422 ) ;
#16528 = APPROVAL ( #5924, 'UNKNOWN' ) ;
#16530 = EDGE_LOOP ( 'NONE', ( #15405, #6945, #32548, #6023 ) ) ;
#16529 = DIRECTION ( 'NONE',  ( 0.000000000000000000, 0.9510565162951544194, -0.3090169943749448977 ) ) ;
#16531 = CARTESIAN_POINT ( 'NONE',  ( -6.337550801365593678, 3.368539882008727115, 1.828967928396026954 ) ) ;
#16532 = DIRECTION ( 'NONE',  ( -0.000000000000000000, -1.000000000000000000, -0.000000000000000000 ) ) ;
#16533 = CARTESIAN_POINT ( 'NONE',  ( 25.76000000000000512, 2.749440278475487442, 1.299952413566024756 ) ) ;
#16534 = DIRECTION ( 'NONE',  ( -1.000000000000000000, 0.000000000000000000, -0.000000000000000000 ) ) ;
#16535 = ORIENTED_EDGE ( 'NONE', *, *, #9825, .F. ) ;
#16537 = VERTEX_POINT ( 'NONE', #28086 ) ;
#16536 = CARTESIAN_POINT ( 'NONE',  ( 10.56183597391177464, 4.753758587302147731, 0.000000000000000000 ) ) ;
#16538 = CARTESIAN_POINT ( 'NONE',  ( 15.28872660057389155, 20.76088595412472415, 4.629213727441584325 ) ) ;
#16539 = EDGE_CURVE ( 'NONE', #11692, #10028, #606, .T. ) ;
#16540 = CARTESIAN_POINT ( 'NONE',  ( -4.075891499408641642E-16, -4.753758587302147731, 0.000000000000000000 ) ) ;
#16541 = AXIS2_PLACEMENT_3D ( 'NONE', #19028, #21541, #11648 ) ;
#16542 = CARTESIAN_POINT ( 'NONE',  ( -29.24806983202759625, 15.94212570950531038, 1.500000000000000000 ) ) ;
#16543 = DIRECTION ( 'NONE',  ( 1.000000000000000000, 0.000000000000000000, 0.000000000000000000 ) ) ;
#16544 = DIRECTION ( 'NONE',  ( 1.387778780781445676E-14, 0.000000000000000000, 1.000000000000000000 ) ) ;
#16545 = AXIS2_PLACEMENT_3D ( 'NONE', #22306, #26997, #9081 ) ;
#16546 = EDGE_CURVE ( 'NONE', #5629, #22098, #185, .T. ) ;
#16547 = LINE ( 'NONE', #11059, #22588 ) ;
#16548 = CARTESIAN_POINT ( 'NONE',  ( -3.937550801365593323, 3.368539882008727115, 1.828967928396026954 ) ) ;
#16549 = CARTESIAN_POINT ( 'NONE',  ( -56.27770248097862549, -0.0003384977252891612984, 1.500000000000000000 ) ) ;
#16550 = VERTEX_POINT ( 'NONE', #344 ) ;
#16551 = VECTOR ( 'NONE', #19855, 1000.000000000000000 ) ;
#16552 = CARTESIAN_POINT ( 'NONE',  ( 21.07900179210102820, -21.69205259094532678, 1.492586111083458400 ) ) ;
#16553 = CARTESIAN_POINT ( 'NONE',  ( 2.795120570939530591, 9.022485053488420448, -3.714272345039503431 ) ) ;
#16555 = CARTESIAN_POINT ( 'NONE',  ( 25.75999999999999801, -2.208672634433321348E-15, 0.000000000000000000 ) ) ;
#16554 = DIRECTION ( 'NONE',  ( 1.000000000000000000, 0.000000000000000000, 0.000000000000000000 ) ) ;
#16556 = ORIENTED_EDGE ( 'NONE', *, *, #24471, .F. ) ;
#16557 = CARTESIAN_POINT ( 'NONE',  ( 7.249760686538667009, -7.530955069117495349, -2.741043480755002371 ) ) ;
#16558 = VERTEX_POINT ( 'NONE', #26068 ) ;
#16559 = FACE_BOUND ( 'NONE', #13831, .T. ) ;
#16561 = EDGE_LOOP ( 'NONE', ( #23338, #23135, #30811, #12597, #20482, #29696, #28571, #13927, #9902, #2964, #24735, #24172, #5317, #18524, #16943 ) ) ;
#16560 = CARTESIAN_POINT ( 'NONE',  ( 84.96565083440447097, -4.060156691890333569, -3.995335864730365394 ) ) ;
#16562 = CIRCLE ( 'NONE', #8085, 8.749000000000002331 ) ;
#16563 = ORIENTED_EDGE ( 'NONE', *, *, #21227, .F. ) ;
#16564 = LINE ( 'NONE', #32433, #122 ) ;
#16565 = VECTOR ( 'NONE', #18672, 1000.000000000000000 ) ;
#16566 = EDGE_CURVE ( 'NONE', #26528, #23643, #2522, .T. ) ;
#16567 = DIRECTION ( 'NONE',  ( -1.000000000000000000, 0.000000000000000000, 0.000000000000000000 ) ) ;
#16568 = APPROVAL ( #677, 'UNSPECIFIED' ) ;
#16570 = ORIENTED_EDGE ( 'NONE', *, *, #16396, .F. ) ;
#16569 = CARTESIAN_POINT ( 'NONE',  ( -3.424298583717175800E-16, -3.993798362933329127, 3.024842911000676704 ) ) ;
#16571 = CARTESIAN_POINT ( 'NONE',  ( 15.54097886440126963, 11.19125261692687268, -1.500000000000000000 ) ) ;
#16572 = AXIS2_PLACEMENT_3D ( 'NONE', #25943, #10886, #515 ) ;
#16573 = CARTESIAN_POINT ( 'NONE',  ( 3.499999999999999556, -6.700937042937042065, 0.8165525598867410251 ) ) ;
#16574 = CARTESIAN_POINT ( 'NONE',  ( 108.1106105794459609, -19.66212694419082396, -1.922248489706470664 ) ) ;
#16575 = CARTESIAN_POINT ( 'NONE',  ( 9.851448551969891554, -11.91728849095333231, -1.500000000000000000 ) ) ;
#16577 = ORIENTED_EDGE ( 'NONE', *, *, #25932, .T. ) ;
#16576 = CARTESIAN_POINT ( 'NONE',  ( 107.4493004345435878, -17.34926456629034419, -4.492266965380428800 ) ) ;
#16578 = CARTESIAN_POINT ( 'NONE',  ( 7.064423637759001728, 3.647351267792902529, 7.953573330858847434 ) ) ;
#16579 = VECTOR ( 'NONE', #25075, 1000.000000000000000 ) ;
#16580 = DIRECTION ( 'NONE',  ( 1.000000000000000000, -0.000000000000000000, -0.000000000000000000 ) ) ;
#16581 = PLANE ( 'NONE',  #24816 ) ;
#16582 = ADVANCED_FACE ( 'NONE', ( #12689 ), #3170, .T. ) ;
#16583 = DESIGN_CONTEXT ( 'detailed design', #18239, 'design' ) ;
#16584 = CARTESIAN_POINT ( 'NONE',  ( -3.306376978575949366, -0.1572233378491262878, 2.999999999999999556 ) ) ;
#16585 = CARTESIAN_POINT ( 'NONE',  ( 0.5640493910588681992, -6.134141009809383149, 7.306425354229878266 ) ) ;
#16586 = ORIENTED_EDGE ( 'NONE', *, *, #12186, .F. ) ;
#16587 = CARTESIAN_POINT ( 'NONE',  ( -17.35000000000000142, -10.96966150227469505, -11.50000000000000000 ) ) ;
#16588 = EDGE_CURVE ( 'NONE', #29938, #11560, #5405, .T. ) ;
#16589 = VECTOR ( 'NONE', #14628, 999.9999999999998863 ) ;
#16590 = CIRCLE ( 'NONE', #29421, 8.750000000000000000 ) ;
#16591 = CARTESIAN_POINT ( 'NONE',  ( 107.4362021328091288, -17.16097444018121365, -4.113685213696737897 ) ) ;
#16592 = DIRECTION ( 'NONE',  ( -1.000000000000000000, 0.000000000000000000, 0.000000000000000000 ) ) ;
#16593 = EDGE_LOOP ( 'NONE', ( #31026, #12717 ) ) ;
#16594 = CIRCLE ( 'NONE', #13935, 6.248999999999998778 ) ;
#16595 = VECTOR ( 'NONE', #17656, 1000.000000000000000 ) ;
#16596 = CONICAL_SURFACE ( 'NONE', #2740, 297.0265809045899346, 0.4915790642873721361 ) ;
#16597 = CARTESIAN_POINT ( 'NONE',  ( 25.17250000273118715, 2.378061970571979433, -1.291182301015470602 ) ) ;
#16598 = CARTESIAN_POINT ( 'NONE',  ( 17.39502519978889694, -21.04076415203780925, 1.751145182513948351 ) ) ;
#16599 = ORIENTED_EDGE ( 'NONE', *, *, #4653, .T. ) ;
#16600 = DIRECTION ( 'NONE',  ( 0.9151824489413823427, -0.4030398059120888776, 0.000000000000000000 ) ) ;
#16601 = ORIENTED_EDGE ( 'NONE', *, *, #16628, .T. ) ;
#16602 = B_SPLINE_CURVE_WITH_KNOTS ( 'NONE', 3,
 ( #12495, #12154, #22352, #12648, #10126, #20350, #7648, #10804 ),
 .UNSPECIFIED., .F., .F.,
 ( 4, 2, 2, 4 ),
 ( 0.000000000000000000, 0.5000000000000000000, 0.7500000000000000000, 1.000000000000000000 ),
 .UNSPECIFIED. ) ;
#16603 = ORIENTED_EDGE ( 'NONE', *, *, #24477, .F. ) ;
#16604 = CARTESIAN_POINT ( 'NONE',  ( 24.76851591958248378, -17.41692718791852812, -1.262548836151033305 ) ) ;
#16606 = ORIENTED_EDGE ( 'NONE', *, *, #2626, .F. ) ;
#16605 = DIRECTION ( 'NONE',  ( -1.000000000000000000, 0.000000000000000000, 0.000000000000000000 ) ) ;
#16607 = ORIENTED_EDGE ( 'NONE', *, *, #27973, .F. ) ;
#16608 = CARTESIAN_POINT ( 'NONE',  ( 3.249999999999999556, -5.538577986808947529, 6.772677083992368452 ) ) ;
#16609 = ORIENTED_EDGE ( 'NONE', *, *, #24501, .T. ) ;
#16610 = CARTESIAN_POINT ( 'NONE',  ( 14.89337309020629085, 18.05463290658611442, 1.508259000770581837 ) ) ;
#16611 = CARTESIAN_POINT ( 'NONE',  ( 5.887530024394193262, -7.753515897409866575, -3.218326717262334657 ) ) ;
#16613 = EDGE_LOOP ( 'NONE', ( #24742, #13881, #7209, #23325 ) ) ;
#16612 = DIRECTION ( 'NONE',  ( -1.348670067729972350E-16, 0.9848077530122080203, 0.1736481776669307198 ) ) ;
#16614 = CARTESIAN_POINT ( 'NONE',  ( -2.037945749704288773E-16, -2.376879293651036118, -4.116875700062107235 ) ) ;
#16615 = DIRECTION ( 'NONE',  ( 0.5150380749100547106, 1.049727191138618326E-16, 0.8571673007021120005 ) ) ;
#16616 = VECTOR ( 'NONE', #21940, 1000.000000000000114 ) ;
#16617 = CYLINDRICAL_SURFACE ( 'NONE', #2139, 5.010000000000000675 ) ;
#16618 = CARTESIAN_POINT ( 'NONE',  ( 5.489321708267612898, 5.138670926724898003, 6.285661071314490478 ) ) ;
#16619 = CARTESIAN_POINT ( 'NONE',  ( 108.0598809612459519, -18.93163306209645214, 4.567750811147567092 ) ) ;
#16620 = CIRCLE ( 'NONE', #26768, 0.5000000000000004441 ) ;
#16621 = B_SPLINE_CURVE_WITH_KNOTS ( 'NONE', 3,
 ( #19331, #17323, #19154, #4118, #27517, #14792, #11478, #16639, #11627, #1956 ),
 .UNSPECIFIED., .F., .F.,
 ( 4, 3, 3, 4 ),
 ( 2.562756726049955231E-17, 0.001785006303531573362, 0.002677509960260540146, 0.003454325209724627699 ),
 .UNSPECIFIED. ) ;
#16622 = VECTOR ( 'NONE', #14472, 1000.000000000000227 ) ;
#16623 =( BOUNDED_SURFACE ( )  B_SPLINE_SURFACE ( 3, 3, ( 
 ( #21201, #4133, #31398, #24005 ),
 ( #8644, #3803, #8475, #21687 ),
 ( #21349, #18673, #28874, #19170 ),
 ( #31892, #29362, #3985, #9459 ) ),
 .UNSPECIFIED., .F., .F., .F. ) 
 B_SPLINE_SURFACE_WITH_KNOTS ( ( 4, 4 ),
 ( 4, 4 ),
 ( 0.000000000000000000, 1.000000000000000000 ),
 ( 0.000000000000000000, 1.000000000000000000 ),
 .UNSPECIFIED. ) 
 GEOMETRIC_REPRESENTATION_ITEM ( )  RATIONAL_B_SPLINE_SURFACE ( (
 ( 1.000000000000000000, 0.9321687722090974404, 0.9321687722090974404, 1.000000000000000000),
 ( 0.6539698177806696489, 0.6096102421024139906, 0.6096102421024139906, 0.6539698177806696489),
 ( 0.6539698177806696489, 0.6096102421024139906, 0.6096102421024139906, 0.6539698177806696489),
 ( 1.000000000000000000, 0.9321687722090974404, 0.9321687722090974404, 1.000000000000000000) ) ) 
 REPRESENTATION_ITEM ( '' )  SURFACE ( )  );
#16624 = CARTESIAN_POINT ( 'NONE',  ( 110.4915906369627123, -18.78144465615449832, -4.522129901861166701 ) ) ;
#16625 = CARTESIAN_POINT ( 'NONE',  ( 85.14283307489681363, -6.932413485865820846, -0.4367664097874476292 ) ) ;
#16626 = FACE_OUTER_BOUND ( 'NONE', #2788, .T. ) ;
#16627 = AXIS2_PLACEMENT_3D ( 'NONE', #10431, #18106, #25822 ) ;
#16628 = EDGE_CURVE ( 'NONE', #15401, #22172, #24931, .T. ) ;
#16629 = EDGE_CURVE ( 'NONE', #13759, #25811, #17709, .T. ) ;
#16630 = VECTOR ( 'NONE', #13872, 1000.000000000000000 ) ;
#16631 = VECTOR ( 'NONE', #21435, 1000.000000000000000 ) ;
#16632 = LINE ( 'NONE', #26839, #1673 ) ;
#16633 = DIRECTION ( 'NONE',  ( 0.000000000000000000, 0.4067366430758010964, -0.9135454576426006446 ) ) ;
#16634 = DIRECTION ( 'NONE',  ( -0.03489949670250104552, -0.9993908270190956511, 0.000000000000000000 ) ) ;
#16635 = CARTESIAN_POINT ( 'NONE',  ( 3.499999999999999556, 2.429606751577119805, -5.757344182232886354 ) ) ;
#16636 = CARTESIAN_POINT ( 'NONE',  ( -6.750050802731187183, 2.983565686104819648, 0.3135853898029609677 ) ) ;
#16637 = ORIENTED_EDGE ( 'NONE', *, *, #7936, .T. ) ;
#16638 = CARTESIAN_POINT ( 'NONE',  ( -6.650050800000002482, 2.853674364686379583, 1.549418761218565921 ) ) ;
#16639 = CARTESIAN_POINT ( 'NONE',  ( 107.2161092216380212, 16.62048478722980960, -1.959702381427974149 ) ) ;
#16640 = CARTESIAN_POINT ( 'NONE',  ( -5.600050802731187716, -3.113457007523259268, 0.9222479816126455399 ) ) ;
#16641 = CARTESIAN_POINT ( 'NONE',  ( 8.060276135842133982, -2.738905749622256636, 1.499999999999713785 ) ) ;
#16642 = ORIENTED_EDGE ( 'NONE', *, *, #1222, .F. ) ;
#16643 = CARTESIAN_POINT ( 'NONE',  ( 13.10266514559061868, -14.23637329403187479, -1.500000000000000000 ) ) ;
#16644 = AXIS2_PLACEMENT_3D ( 'NONE', #13149, #20190, #27869 ) ;
#16645 = CIRCLE ( 'NONE', #27350, 0.4999999999999997780 ) ;
#16646 = CIRCLE ( 'NONE', #4379, 5.009999999999999787 ) ;
#16647 = ORIENTED_EDGE ( 'NONE', *, *, #2015, .T. ) ;
#16648 = CARTESIAN_POINT ( 'NONE',  ( 3.334879154417976554, -11.42275455914650095, 1.500000000000000000 ) ) ;
#16649 = APPROVAL_ROLE ( '' ) ;
#16650 = DIRECTION ( 'NONE',  ( 0.000000000000000000, 0.000000000000000000, 1.000000000000000000 ) ) ;
#16651 = ORIENTED_EDGE ( 'NONE', *, *, #32867, .T. ) ;
#16652 = CARTESIAN_POINT ( 'NONE',  ( 102.3439814245663655, -2.854902261462827884, 3.993434327364640435 ) ) ;
#16653 = CIRCLE ( 'NONE', #18787, 5.009999999999999787 ) ;
#16654 = AXIS2_PLACEMENT_3D ( 'NONE', #11756, #27308, #19479 ) ;
#16655 = DIRECTION ( 'NONE',  ( 1.000000000000000000, -8.574039729943018344E-17, -0.000000000000000000 ) ) ;
#16656 = CARTESIAN_POINT ( 'NONE',  ( 54.94707873175313750, -5.417356489197679537, -4.073741752274519179 ) ) ;
#16657 = CARTESIAN_POINT ( 'NONE',  ( 24.07542780979855834, -17.38801686517327738, -1.438486003925340428 ) ) ;
#16658 = CARTESIAN_POINT ( 'NONE',  ( 3.063284526839890276, 4.729683950898869504, 7.360373001730925679 ) ) ;
#16659 = ORIENTED_EDGE ( 'NONE', *, *, #3269, .F. ) ;
#16660 = CARTESIAN_POINT ( 'NONE',  ( 8.906813281368062718, 0.1505923090604537329, 1.366675429750776161 ) ) ;
#16661 = CARTESIAN_POINT ( 'NONE',  ( 0.000000000000000000, 0.000000000000000000, 0.000000000000000000 ) ) ;
#16662 = CARTESIAN_POINT ( 'NONE',  ( 18.93569951633547177, -3.895973091535266608, -2.639289341045732762 ) ) ;
#16663 = EDGE_CURVE ( 'NONE', #14221, #11829, #3999, .T. ) ;
#16665 = ORIENTED_EDGE ( 'NONE', *, *, #17368, .F. ) ;
#16664 = FACE_OUTER_BOUND ( 'NONE', #32894, .T. ) ;
#16666 = AXIS2_PLACEMENT_3D ( 'NONE', #6417, #6118, #31859 ) ;
#16667 = CARTESIAN_POINT ( 'NONE',  ( 7.064632816082964339, -8.721381771256204729, -0.7071067811865412445 ) ) ;
#16668 = AXIS2_PLACEMENT_3D ( 'NONE', #19617, #29815, #24797 ) ;
#16669 = CARTESIAN_POINT ( 'NONE',  ( 10.00000000000000000, -3.055657119358777152, -3.641590349731960163 ) ) ;
#16670 = CARTESIAN_POINT ( 'NONE',  ( -53.35155202832373078, 4.402097243136373628, 5.049999999999999822 ) ) ;
#16671 = DIRECTION ( 'NONE',  ( 1.000000000000000000, -8.574039729943018344E-17, -0.000000000000000000 ) ) ;
#16672 = LINE ( 'NONE', #26885, #8756 ) ;
#16673 = VECTOR ( 'NONE', #19001, 1000.000000000000000 ) ;
#16674 = AXIS2_PLACEMENT_3D ( 'NONE', #21943, #23950, #29658 ) ;
#16675 = CARTESIAN_POINT ( 'NONE',  ( -47.55999999999999517, -10.96999999999998643, 9.000000000000000000 ) ) ;
#16676 = CARTESIAN_POINT ( 'NONE',  ( 7.249760686538667009, -5.151476664237435443, -6.139290821770307716 ) ) ;
#16677 = DIRECTION ( 'NONE',  ( 0.000000000000000000, -0.5877852522924799095, 0.8090169943749425663 ) ) ;
#16678 = ORIENTED_EDGE ( 'NONE', *, *, #30235, .T. ) ;
#16679 = VECTOR ( 'NONE', #28264, 1000.000000000000000 ) ;
#16680 = EDGE_CURVE ( 'NONE', #28186, #21430, #13672, .T. ) ;
#16681 = AXIS2_PLACEMENT_3D ( 'NONE', #6142, #26204, #7979 ) ;
#16682 = CARTESIAN_POINT ( 'NONE',  ( 20.86000000273118715, -1.942864903642428587, -1.573300977624592756 ) ) ;
#16683 = ORIENTED_EDGE ( 'NONE', *, *, #25449, .T. ) ;
#16684 = CIRCLE ( 'NONE', #25244, 1.676012832569465205 ) ;
#16685 = CARTESIAN_POINT ( 'NONE',  ( 24.94969606499759962, -17.50686502442625425, -1.454450177773842112 ) ) ;
#16686 = B_SPLINE_CURVE_WITH_KNOTS ( 'NONE', 3,
 ( #15372, #15871, #16020, #17908, #26081, #205 ),
 .UNSPECIFIED., .F., .F.,
 ( 4, 2, 4 ),
 ( 0.000000000000000000, 0.001111101124723993692, 0.002222202249447986951 ),
 .UNSPECIFIED. ) ;
#16687 = DIRECTION ( 'NONE',  ( 0.4999999999999978351, 0.8660254037844398178, 0.000000000000000000 ) ) ;
#16688 = EDGE_CURVE ( 'NONE', #22217, #29709, #8582, .T. ) ;
#16689 = FACE_OUTER_BOUND ( 'NONE', #68, .T. ) ;
#16690 = DIRECTION ( 'NONE',  ( 0.000000000000000000, -0.9659258262890700886, 0.2588190451025141336 ) ) ;
#16691 = CARTESIAN_POINT ( 'NONE',  ( 0.1606233164476231767, -5.257199111574093031, -9.238724727306442119 ) ) ;
#16692 = ORIENTED_EDGE ( 'NONE', *, *, #3476, .F. ) ;
#16693 = CYLINDRICAL_SURFACE ( 'NONE', #3349, 5.010000000000000675 ) ;
#16694 = VECTOR ( 'NONE', #7449, 1000.000000000000000 ) ;
#16695 = VERTEX_POINT ( 'NONE', #10853 ) ;
#16697 = CIRCLE ( 'NONE', #31660, 2.999999999999999112 ) ;
#16696 = PERSON_AND_ORGANIZATION_ROLE ( 'classification_officer' ) ;
#16698 = EDGE_CURVE ( 'NONE', #24378, #5341, #29983, .T. ) ;
#16699 = CARTESIAN_POINT ( 'NONE',  ( 28.66412195420384634, -6.764514867728558478, 3.994702635811785196 ) ) ;
#16700 = VECTOR ( 'NONE', #27202, 1000.000000000000000 ) ;
#16701 = CIRCLE ( 'NONE', #31666, 0.5000000000000008882 ) ;
#16702 = CIRCLE ( 'NONE', #24724, 7.482234843104714983 ) ;
#16703 = CARTESIAN_POINT ( 'NONE',  ( -3.362942409646513031, -5.022711880624455567E-15, 2.999999999999999556 ) ) ;
#16704 = ORIENTED_EDGE ( 'NONE', *, *, #16680, .F. ) ;
#16705 = CARTESIAN_POINT ( 'NONE',  ( 107.7536796087345294, 16.80655079293032017, 0.4463807625373348298 ) ) ;
#16706 = ADVANCED_FACE ( 'NONE', ( #31755 ), #24083, .T. ) ;
#16707 = ORIENTED_EDGE ( 'NONE', *, *, #18600, .F. ) ;
#16708 = ORIENTED_EDGE ( 'NONE', *, *, #16190, .F. ) ;
#16709 = FACE_OUTER_BOUND ( 'NONE', #10629, .T. ) ;
#16710 = CARTESIAN_POINT ( 'NONE',  ( -2.462550801365593678, 0.3701630799359330593, -3.521866450007987037 ) ) ;
#16711 = CARTESIAN_POINT ( 'NONE',  ( 23.54750000000000654, -2.594547506269383685, -0.7685399846772043020 ) ) ;
#16712 = CARTESIAN_POINT ( 'NONE',  ( 1.947447778977702049, -0.8602978363041573484, -1.758031988188919037 ) ) ;
#16714 = ORIENTED_EDGE ( 'NONE', *, *, #12328, .T. ) ;
#16713 = PLANE ( 'NONE',  #29368 ) ;
#16715 = CARTESIAN_POINT ( 'NONE',  ( -6.937550801365595099, -1.828967928396026510, 3.368539882008728004 ) ) ;
#16716 = FACE_OUTER_BOUND ( 'NONE', #27644, .T. ) ;
#16717 = CARTESIAN_POINT ( 'NONE',  ( -33.81874022276151237, 19.50000000000000000, 1.977928362984239019 ) ) ;
#16719 = ADVANCED_FACE ( 'NONE', ( #8342 ), #23874, .F. ) ;
#16718 = CYLINDRICAL_SURFACE ( 'NONE', #32248, 8.749000000000002331 ) ;
#16720 = ORIENTED_EDGE ( 'NONE', *, *, #26232, .T. ) ;
#16722 = ORIENTED_EDGE ( 'NONE', *, *, #811, .T. ) ;
#16721 = CARTESIAN_POINT ( 'NONE',  ( 4.749760686538667009, 5.151476664237477188, 6.139290821770273077 ) ) ;
#16723 = ADVANCED_FACE ( 'NONE', ( #16192 ), #3825, .T. ) ;
#16724 = AXIS2_PLACEMENT_3D ( 'NONE', #1235, #18609, #28799 ) ;
#16725 = AXIS2_PLACEMENT_3D ( 'NONE', #12342, #30262, #28222 ) ;
#16726 = DIRECTION ( 'NONE',  ( 0.000000000000000000, 0.000000000000000000, -1.000000000000000000 ) ) ;
#16727 = AXIS2_PLACEMENT_3D ( 'NONE', #22716, #7470, #1114 ) ;
#16728 = CARTESIAN_POINT ( 'NONE',  ( 22.29750000273118715, 2.594547506269380133, 0.7685399846772031918 ) ) ;
#16729 = AXIS2_PLACEMENT_3D ( 'NONE', #27882, #30396, #7975 ) ;
#16730 = AXIS2_PLACEMENT_3D ( 'NONE', #9990, #4812, #7471 ) ;
#16731 = CARTESIAN_POINT ( 'NONE',  ( -17.84619894073145119, 15.94212570950478636, 1.500000000000000000 ) ) ;
#16732 = VECTOR ( 'NONE', #26069, 1000.000000000000000 ) ;
#16733 = CARTESIAN_POINT ( 'NONE',  ( -6.350050802731187716, -2.983565686104819648, -0.3135853898029605791 ) ) ;
#16734 = CARTESIAN_POINT ( 'NONE',  ( -4.099836581868715690, -5.441267727784081742, -1.745641626744263153 ) ) ;
#16735 = DIRECTION ( 'NONE',  ( 0.000000000000000000, 0.000000000000000000, -1.000000000000000000 ) ) ;
#16736 = APPROVAL_PERSON_ORGANIZATION ( #24345, #11877, #8811 ) ;
#16737 = CARTESIAN_POINT ( 'NONE',  ( 54.90142980599745925, -3.782945109527762639, 1.169950777188785596 ) ) ;
#16738 = CARTESIAN_POINT ( 'NONE',  ( -2.237550801365593589, 1.088641768524161613, 3.675193018007247403 ) ) ;
#16739 = CARTESIAN_POINT ( 'NONE',  ( 5.338982705820766102E-17, 0.6226916219172039524, 4.971152295393303611 ) ) ;
#16740 = ORIENTED_EDGE ( 'NONE', *, *, #24719, .F. ) ;
#16741 = EDGE_CURVE ( 'NONE', #2976, #3034, #26557, .T. ) ;
#16742 = DIRECTION ( 'NONE',  ( 0.000000000000000000, 0.000000000000000000, 1.000000000000000000 ) ) ;
#16743 = CARTESIAN_POINT ( 'NONE',  ( 47.99837860531645362, -3.577301031427907230, -2.713652344655542503 ) ) ;
#16745 = CARTESIAN_POINT ( 'NONE',  ( 24.22349034905825960, -17.32906192875332962, 1.351230503573712216 ) ) ;
#16744 = CARTESIAN_POINT ( 'NONE',  ( 6.880159790065804692, -2.190520500543428728, -8.451885315426448386 ) ) ;
#16746 = VERTEX_POINT ( 'NONE', #29380 ) ;
#16747 = VECTOR ( 'NONE', #8046, 1000.000000000000114 ) ;
#16748 = CARTESIAN_POINT ( 'NONE',  ( 10.25005080000000035, 0.000000000000000000, 0.000000000000000000 ) ) ;
#16749 = AXIS2_PLACEMENT_3D ( 'NONE', #11994, #24195, #1319 ) ;
#16750 = VERTEX_POINT ( 'NONE', #28729 ) ;
#16751 = FACE_OUTER_BOUND ( 'NONE', #14824, .T. ) ;
#16753 = ORIENTED_EDGE ( 'NONE', *, *, #8346, .T. ) ;
#16752 = CARTESIAN_POINT ( 'NONE',  ( 40.87774960799753643, -5.751897813703351403, -3.998505783863144813 ) ) ;
#16754 = ORIENTED_EDGE ( 'NONE', *, *, #26240, .F. ) ;
#16755 = CIRCLE ( 'NONE', #26900, 0.5000000000000000000 ) ;
#16756 = ADVANCED_FACE ( 'NONE', ( #16003 ), #31413, .T. ) ;
#16757 = LINE ( 'NONE', #24930, #18291 ) ;
#16758 = CARTESIAN_POINT ( 'NONE',  ( 0.000000000000000000, 0.000000000000000000, 0.000000000000000000 ) ) ;
#16760 = ORIENTED_EDGE ( 'NONE', *, *, #4184, .T. ) ;
#16759 = CARTESIAN_POINT ( 'NONE',  ( -2.596426400646765220, -12.68075645936657381, -1.499999999999999778 ) ) ;
#16761 = CARTESIAN_POINT ( 'NONE',  ( 14.71918161885289855, 9.125819088444179883, -1.500000000000414557 ) ) ;
#16762 = CARTESIAN_POINT ( 'NONE',  ( 22.75111450864416085, -1.241879311143409511E-16, -2.499999999999998668 ) ) ;
#16763 = CARTESIAN_POINT ( 'NONE',  ( 25.98690466878746008, 22.56136012750956965, 0.4463807625373348298 ) ) ;
#16764 = ADVANCED_FACE ( 'NONE', ( #19185 ), #24209, .T. ) ;
#16765 = CC_DESIGN_APPROVAL ( #7375, ( #1293 ) ) ;
#16766 = CARTESIAN_POINT ( 'NONE',  ( 7.166310626576994025, -7.340520188510355482, -1.000000000000000000 ) ) ;
#16768 = ORIENTED_EDGE ( 'NONE', *, *, #4041, .T. ) ;
#16767 = CARTESIAN_POINT ( 'NONE',  ( 107.5607856375281557, -18.96928505737806248, -4.559234559040556967 ) ) ;
#16769 = EDGE_CURVE ( 'NONE', #9461, #2248, #6309, .T. ) ;
#16770 = FACE_OUTER_BOUND ( 'NONE', #12251, .T. ) ;
#16771 = CARTESIAN_POINT ( 'NONE',  ( 24.98500000273118715, -0.2613211581691358698, -2.486304738420681559 ) ) ;
#16772 = CARTESIAN_POINT ( 'NONE',  ( 54.97742507208633356, -6.506533559248902421, 3.993434333358794053 ) ) ;
#16773 = DIRECTION ( 'NONE',  ( 1.000000000000000000, -8.574039729943018344E-17, -0.000000000000000000 ) ) ;
#16774 = CARTESIAN_POINT ( 'NONE',  ( 102.8580990270160385, -4.820463887425400884, -4.522129901861164036 ) ) ;
#16775 = AXIS2_PLACEMENT_3D ( 'NONE', #13413, #25995, #22965 ) ;
#16776 = VERTEX_POINT ( 'NONE', #8975 ) ;
#16777 = CARTESIAN_POINT ( 'NONE',  ( 0.7632845268398871230, 0.4999240074894433228, 8.734705317681628500 ) ) ;
#16778 = CARTESIAN_POINT ( 'NONE',  ( 107.4500373638804120, -17.36019379023677089, -4.522129901861164036 ) ) ;
#16779 = FACE_OUTER_BOUND ( 'NONE', #22932, .T. ) ;
#16780 = ORIENTED_EDGE ( 'NONE', *, *, #18607, .T. ) ;
#16781 = ADVANCED_FACE ( 'NONE', ( #1144 ), #11341, .F. ) ;
#16782 = CC_DESIGN_DATE_AND_TIME_ASSIGNMENT ( #22871, #32927, ( #27439 ) ) ;
#16783 = B_SPLINE_CURVE_WITH_KNOTS ( 'NONE', 3,
 ( #2646, #12813, #25212, #17513 ),
 .UNSPECIFIED., .F., .F.,
 ( 4, 4 ),
 ( 0.001654338126360077339, 0.002457869280243896344 ),
 .UNSPECIFIED. ) ;
#16784 = CARTESIAN_POINT ( 'NONE',  ( 3.063284526839887167, -5.538577986808947529, 6.772677083992368452 ) ) ;
#16785 = DIRECTION ( 'NONE',  ( 0.000000000000000000, 0.000000000000000000, -1.000000000000000000 ) ) ;
#16786 = SECURITY_CLASSIFICATION ( '', '', #22987 ) ;
#16787 = ORIENTED_EDGE ( 'NONE', *, *, #25321, .T. ) ;
#16788 = DIRECTION ( 'NONE',  ( -0.000000000000000000, -0.2588190451025240701, -0.9659258262890673130 ) ) ;
#16789 = ORIENTED_EDGE ( 'NONE', *, *, #1620, .F. ) ;
#16790 = EDGE_LOOP ( 'NONE', ( #20371, #2664, #11069 ) ) ;
#16791 = CARTESIAN_POINT ( 'NONE',  ( 7.064632918400240769, 3.647351267791677731, -7.953573330858177748 ) ) ;
#16793 = ORIENTED_EDGE ( 'NONE', *, *, #4260, .F. ) ;
#16792 = CARTESIAN_POINT ( 'NONE',  ( 6.038144853276843804, -8.412419482080416344, 1.027626812407973267 ) ) ;
#16794 = ORIENTED_EDGE ( 'NONE', *, *, #6263, .F. ) ;
#16795 = CARTESIAN_POINT ( 'NONE',  ( 22.73500000136559862, 1.570731468192929858, 2.892927487894329630 ) ) ;
#16796 = EDGE_CURVE ( 'NONE', #9413, #15401, #3064, .T. ) ;
#16797 = EDGE_LOOP ( 'NONE', ( #6389, #13420, #14070, #20140 ) ) ;
#16798 = CARTESIAN_POINT ( 'NONE',  ( 12.61464622672343516, 16.97301654637829671, 1.508259000770581837 ) ) ;
#16799 = CARTESIAN_POINT ( 'NONE',  ( 10.00000000000000000, -1.625881193364669297, -4.467071865485488402 ) ) ;
#16801 = EDGE_LOOP ( 'NONE', ( #20258, #3451, #4650, #9071 ) ) ;
#16800 = CARTESIAN_POINT ( 'NONE',  ( 41.34457103394125710, -4.143788916011438950, -1.529340246550954685 ) ) ;
#16802 = CARTESIAN_POINT ( 'NONE',  ( 3.063284526839887167, 0.000000000000000000, 0.000000000000000000 ) ) ;
#16803 = CARTESIAN_POINT ( 'NONE',  ( 7.249760686538667009, 0.000000000000000000, 0.000000000000000000 ) ) ;
#16804 = CARTESIAN_POINT ( 'NONE',  ( -56.49561586466536056, 0.04964621674521208644, 1.500000000000000000 ) ) ;
#16805 = CARTESIAN_POINT ( 'NONE',  ( 6.357668022120090079, 5.080751859797355330, 6.947679035623472998 ) ) ;
#16806 = CARTESIAN_POINT ( 'NONE',  ( 6.448894291894883501, -17.04229596238074151, -4.522129901861166701 ) ) ;
#16807 = FACE_OUTER_BOUND ( 'NONE', #10908, .T. ) ;
#16808 = DIRECTION ( 'NONE',  ( -0.000000000000000000, -0.000000000000000000, 1.000000000000000000 ) ) ;
#16809 = CARTESIAN_POINT ( 'NONE',  ( 7.249760686538667009, -2.741043480754977946, 7.530955069117504230 ) ) ;
#16810 = CARTESIAN_POINT ( 'NONE',  ( 0.1255855353822278031, 9.314797388872380068, 5.239665997526921970 ) ) ;
#16811 = CARTESIAN_POINT ( 'NONE',  ( 23.98500000273118715, -0.2613211581691358698, -2.486304738420681559 ) ) ;
#16812 = CARTESIAN_POINT ( 'NONE',  ( 25.75999999999999801, -2.208672634433321348E-15, 0.000000000000000000 ) ) ;
#16813 = EDGE_CURVE ( 'NONE', #1604, #23747, #23058, .T. ) ;
#16814 = CARTESIAN_POINT ( 'NONE',  ( -5.650050802731187538, -2.331437884370912705, 1.887961173149512062 ) ) ;
#16815 = ORIENTED_EDGE ( 'NONE', *, *, #28587, .F. ) ;
#16816 = CARTESIAN_POINT ( 'NONE',  ( -7.350050800000000883, 0.9222479816126443186, 3.113457007523260156 ) ) ;
#16817 = LINE ( 'NONE', #24989, #23681 ) ;
#16818 = CARTESIAN_POINT ( 'NONE',  ( 0.9232102171129904500, 0.000000000000000000, 4.522129901861156931 ) ) ;
#16819 = CARTESIAN_POINT ( 'NONE',  ( -41.86373177837819526, -16.13513036599590222, 5.128141679950119602 ) ) ;
#16820 = ORIENTED_EDGE ( 'NONE', *, *, #22766, .T. ) ;
#16821 = CARTESIAN_POINT ( 'NONE',  ( 14.08105513877552895, -14.60666186089152419, -1.499999999999999556 ) ) ;
#16822 = ORIENTED_EDGE ( 'NONE', *, *, #31521, .F. ) ;
#16823 = CARTESIAN_POINT ( 'NONE',  ( 0.1512386650912407315, -7.218081413057891638, 1.774506574461718111 ) ) ;
#16824 = CALENDAR_DATE ( 2026, 6, 10 ) ;
#16825 = ORIENTED_EDGE ( 'NONE', *, *, #3599, .T. ) ;
#16826 = CARTESIAN_POINT ( 'NONE',  ( -2.807368950796196305, -12.37532080748741237, 1.500000000000000000 ) ) ;
#16827 = EDGE_CURVE ( 'NONE', #25565, #26497, #19689, .T. ) ;
#16828 = EDGE_CURVE ( 'NONE', #14119, #6329, #27197, .T. ) ;
#16829 = LINE ( 'NONE', #3643, #26188 ) ;
#16830 = CARTESIAN_POINT ( 'NONE',  ( -2.617344628312510135, 0.000000000000000000, 1.468739241856748867 ) ) ;
#16831 = CARTESIAN_POINT ( 'NONE',  ( 21.03177542174510606, -17.18603084754150601, -1.753176640694676047 ) ) ;
#16832 = CARTESIAN_POINT ( 'NONE',  ( 110.0070906499164352, 18.03948353657134263, -4.621439243524461560 ) ) ;
#16833 =( BOUNDED_CURVE ( )  B_SPLINE_CURVE ( 1, ( #14277, #27157 ),
 .UNSPECIFIED., .F., .F. ) 
 B_SPLINE_CURVE_WITH_KNOTS ( ( 2, 2 ),
 ( 0.000000000000000000, 1.000000000000000000 ),
 .UNSPECIFIED. ) 
 CURVE ( )  GEOMETRIC_REPRESENTATION_ITEM ( )  RATIONAL_B_SPLINE_CURVE ( ( 0.9641176721898547797, 0.9641176721898547797 ) ) 
 REPRESENTATION_ITEM ( '' )  );
#16834 = EDGE_CURVE ( 'NONE', #4959, #6174, #11826, .T. ) ;
#16835 = ORIENTED_EDGE ( 'NONE', *, *, #22667, .T. ) ;
#16836 = DIRECTION ( 'NONE',  ( 0.000000000000000000, 1.000000000000000000, 0.000000000000000000 ) ) ;
#16837 = CARTESIAN_POINT ( 'NONE',  ( 56.97280603064898941, -277.2763395528616002, -0.4463807625373402699 ) ) ;
#16838 = CARTESIAN_POINT ( 'NONE',  ( 2.864531114197722328, -5.073635298885090350, -8.105385692883677606 ) ) ;
#16840 = VERTEX_POINT ( 'NONE', #6809 ) ;
#16839 = DIRECTION ( 'NONE',  ( 0.000000000000000000, 0.000000000000000000, 1.000000000000000000 ) ) ;
#16841 = CARTESIAN_POINT ( 'NONE',  ( 7.249760686538667009, -8.721381771256204729, -0.7071067811865429098 ) ) ;
#16842 = CARTESIAN_POINT ( 'NONE',  ( 3.063284526839888944, 8.152713396088756781, 3.174628368996099681 ) ) ;
#16843 = CARTESIAN_POINT ( 'NONE',  ( 3.554613218822866738, -15.76807188677689275, -4.522129901861166701 ) ) ;
#16844 = CARTESIAN_POINT ( 'NONE',  ( 25.94779144751832334, 19.04267035867732361, 1.250701234898322411 ) ) ;
#16845 = CARTESIAN_POINT ( 'NONE',  ( 0.3076688720859437898, 10.24120291390723558, 0.9727984658935059370 ) ) ;
#16846 = DIRECTION ( 'NONE',  ( 0.000000000000000000, 0.000000000000000000, -1.000000000000000000 ) ) ;
#16847 = FACE_OUTER_BOUND ( 'NONE', #25910, .T. ) ;
#16848 = SPHERICAL_SURFACE ( 'NONE', #13990, 0.5000000000000000000 ) ;
#16849 = DIRECTION ( 'NONE',  ( 0.000000000000000000, 0.000000000000000000, -1.000000000000000000 ) ) ;
#16850 = ORIENTED_EDGE ( 'NONE', *, *, #25657, .T. ) ;
#16851 = B_SPLINE_CURVE_WITH_KNOTS ( 'NONE', 3,
 ( #9930, #10584, #25134, #20145 ),
 .UNSPECIFIED., .F., .F.,
 ( 4, 4 ),
 ( 0.000000000000000000, 0.0001149031832728065387 ),
 .UNSPECIFIED. ) ;
#16852 = CYLINDRICAL_SURFACE ( 'NONE', #11918, 0.5000000000000000000 ) ;
#16853 = ORIENTED_EDGE ( 'NONE', *, *, #1389, .F. ) ;
#16854 = LINE ( 'NONE', #1486, #17758 ) ;
#16855 = LINE ( 'NONE', #6975, #6072 ) ;
#16856 = CARTESIAN_POINT ( 'NONE',  ( 3.499999999999999556, -6.700937042937072263, 2.183447440113167826 ) ) ;
#16857 = LINE ( 'NONE', #24374, #7644 ) ;
#16858 = CARTESIAN_POINT ( 'NONE',  ( 5.084999606894402593E-16, -5.227991826304019263, -9.620177616658041941 ) ) ;
#16859 = ORIENTED_EDGE ( 'NONE', *, *, #23847, .F. ) ;
#16860 = DIRECTION ( 'NONE',  ( -1.000000000000000000, -0.000000000000000000, 0.000000000000000000 ) ) ;
#16861 = EDGE_CURVE ( 'NONE', #25021, #9041, #8989, .T. ) ;
#16862 = ORIENTED_EDGE ( 'NONE', *, *, #10582, .T. ) ;
#16863 = PERSON_AND_ORGANIZATION ( #6766, #25292 ) ;
#16864 = B_SPLINE_CURVE_WITH_KNOTS ( 'NONE', 3,
 ( #25117, #12423, #4087, #4233, #19475, #32351, #11750, #19624, #9253, #29822, #6898, #17092, #4423, #24806, #8061, #23291, #5586, #12590, #541, #7904, #12738, #15261, #25464, #2573, #27985, #28287, #2420, #5085, #22944, #56, #25971, #27796, #10244, #3079 ),
 .UNSPECIFIED., .F., .F.,
 ( 4, 2, 2, 2, 2, 2, 2, 2, 2, 2, 2, 2, 2, 2, 2, 2, 4 ),
 ( -5.999999999868128345E-08, 0.001865929031388419103, 0.003731918062776836981, 0.005597907094165255511, 0.006530901609859464559, 0.007463896125553672739, 0.008396890641247883522, 0.009329885156942092569, 0.01119587418833051587, 0.01306186321971893743, 0.01399485773541314995, 0.01492785225110736247, 0.01679384128249578750, 0.01865983031388421601, 0.02239180837666106955, 0.02612378643943793349, 0.02985576450221478703 ),
 .UNSPECIFIED. ) ;
#16865 = CARTESIAN_POINT ( 'NONE',  ( 54.97719654313131343, -6.505560170230147321, 3.995006645005578338 ) ) ;
#16866 = FACE_OUTER_BOUND ( 'NONE', #21214, .T. ) ;
#16867 = CARTESIAN_POINT ( 'NONE',  ( 5.885541838704151374, 6.185046950422397494, -5.674471607902377812 ) ) ;
#16868 = ORIENTED_EDGE ( 'NONE', *, *, #18613, .F. ) ;
#16869 = VERTEX_POINT ( 'NONE', #4311 ) ;
#16870 = DIRECTION ( 'NONE',  ( -1.000000000000000000, 8.574039729943019576E-17, 1.232595164407830946E-32 ) ) ;
#16871 = DIRECTION ( 'NONE',  ( 1.000000000000000000, -0.000000000000000000, 0.000000000000000000 ) ) ;
#16872 = CARTESIAN_POINT ( 'NONE',  ( 23.73500000000000298, -0.2613211581691358698, -2.486304738420681559 ) ) ;
#16873 = CARTESIAN_POINT ( 'NONE',  ( 1.138845227633290769, -9.034331793438131086, -1.500000000000000444 ) ) ;
#16875 = ORIENTED_EDGE ( 'NONE', *, *, #7288, .F. ) ;
#16874 = CARTESIAN_POINT ( 'NONE',  ( 10.00000000000000000, 0.8254815157535241310, 4.681538312723519724 ) ) ;
#16876 = CARTESIAN_POINT ( 'NONE',  ( -3.987550801365593145, 3.521866450007987037, 0.3701630799359328372 ) ) ;
#16877 = DIRECTION ( 'NONE',  ( -1.000000000000000000, 0.000000000000000000, 0.000000000000000000 ) ) ;
#16878 = DIRECTION ( 'NONE',  ( 0.000000000000000000, 1.000000000000000000, 0.000000000000000000 ) ) ;
#16879 = DIRECTION ( 'NONE',  ( 0.9873162094020069279, -0.1587661886298609715, 2.857460637125401170E-14 ) ) ;
#16880 = EDGE_LOOP ( 'NONE', ( #19344, #11719 ) ) ;
#16882 = ORIENTED_EDGE ( 'NONE', *, *, #17071, .F. ) ;
#16881 = CARTESIAN_POINT ( 'NONE',  ( -15.01523975624633067, -21.93625144122058757, 1.063946347602459985 ) ) ;
#16883 = CARTESIAN_POINT ( 'NONE',  ( 2.592584925145449137, 6.844296717726236601, 7.731606906650903888 ) ) ;
#16884 = DIRECTION ( 'NONE',  ( -1.000000000000000000, 8.574039729943018344E-17, -0.000000000000000000 ) ) ;
#16885 = EDGE_CURVE ( 'NONE', #14212, #13759, #25172, .T. ) ;
#16886 = CARTESIAN_POINT ( 'NONE',  ( -23.54713438637984169, 18.60133783399175655, 1.500000000000000000 ) ) ;
#16887 = CARTESIAN_POINT ( 'NONE',  ( -25.28731355807216374, 18.27315738579029158, 1.777518634818306742 ) ) ;
#16888 = CYLINDRICAL_SURFACE ( 'NONE', #19368, 6.000000000000001776 ) ;
#16889 = CARTESIAN_POINT ( 'NONE',  ( 2.440333710190773164, -2.130583817698453508, 10.46055952248795329 ) ) ;
#16890 = EDGE_CURVE ( 'NONE', #31286, #6749, #8116, .T. ) ;
#16891 = CARTESIAN_POINT ( 'NONE',  ( 10.00000000000000000, 3.055657119358849094, -3.641590349731898879 ) ) ;
#16892 = CARTESIAN_POINT ( 'NONE',  ( -4.137550801365594388, 1.828967928396027176, -3.368539882008727115 ) ) ;
#16893 = VERTEX_POINT ( 'NONE', #7308 ) ;
#16894 = CYLINDRICAL_SURFACE ( 'NONE', #17187, 0.5000000000000004441 ) ;
#16895 = ORIENTED_EDGE ( 'NONE', *, *, #12858, .F. ) ;
#16896 =( BOUNDED_SURFACE ( )  B_SPLINE_SURFACE ( 3, 3, ( 
 ( #18136, #5448, #5626, #7946, #25666, #15644, #12964, #289 ),
 ( #23329, #13127, #20512, #433, #18319, #17989, #15804, #28675 ),
 ( #10613, #26012, #23480, #5771, #15947, #3272, #13436, #26643 ),
 ( #26987, #29314, #1569, #19123, #11596, #21303, #3751, #13918 ) ),
 .UNSPECIFIED., .F., .F., .F. ) 
 B_SPLINE_SURFACE_WITH_KNOTS ( ( 4, 4 ),
 ( 4, 2, 2, 4 ),
 ( 0.000000000000000000, 1.000000000000000000 ),
 ( 0.000000000000000000, 0.5000000000000000000, 0.7500000000000000000, 1.000000000000000000 ),
 .UNSPECIFIED. ) 
 GEOMETRIC_REPRESENTATION_ITEM ( )  RATIONAL_B_SPLINE_SURFACE ( (
 ( 1.000000000000000000, 1.000000000000000000, 1.000000000000000000, 1.000000000000000000, 1.000000000000000000, 1.000000000000000000, 1.000000000000000000, 1.000000000000000000),
 ( 0.9743068154145673176, 0.9743068154145673176, 0.9743068154145673176, 0.9743068154145673176, 0.9743068154145673176, 0.9743068154145673176, 0.9743068154145673176, 0.9743068154145673176),
 ( 0.9743068154145673176, 0.9743068154145673176, 0.9743068154145673176, 0.9743068154145673176, 0.9743068154145673176, 0.9743068154145673176, 0.9743068154145673176, 0.9743068154145673176),
 ( 1.000000000000000000, 1.000000000000000000, 1.000000000000000000, 1.000000000000000000, 1.000000000000000000, 1.000000000000000000, 1.000000000000000000, 1.000000000000000000) ) ) 
 REPRESENTATION_ITEM ( '' )  SURFACE ( )  );
#16897 = DIRECTION ( 'NONE',  ( 8.574039729943018344E-17, 1.000000000000000000, 0.000000000000000000 ) ) ;
#16898 = EDGE_CURVE ( 'NONE', #28422, #28176, #24364, .T. ) ;
#16899 = DIRECTION ( 'NONE',  ( 0.000000000000000000, 1.224646799147352961E-16, 1.000000000000000000 ) ) ;
#16901 = CARTESIAN_POINT ( 'NONE',  ( 3.063284526839887167, 0.000000000000000000, 0.000000000000000000 ) ) ;
#16900 = DIRECTION ( 'NONE',  ( 0.000000000000000000, -0.08715574274766567375, 0.9961946980917449901 ) ) ;
#16902 = ADVANCED_FACE ( 'NONE', ( #24699 ), #22204, .T. ) ;
#16903 = ORIENTED_EDGE ( 'NONE', *, *, #5481, .T. ) ;
#16904 = CARTESIAN_POINT ( 'NONE',  ( -53.45715098423449518, 5.485000000000009202, 1.500000000000000000 ) ) ;
#16905 = VERTEX_POINT ( 'NONE', #11657 ) ;
#16906 = CARTESIAN_POINT ( 'NONE',  ( 2.970200390942824065, -9.143933199822406266, 0.5647484629967252090 ) ) ;
#16908 = ORIENTED_EDGE ( 'NONE', *, *, #26372, .F. ) ;
#16907 = CARTESIAN_POINT ( 'NONE',  ( 69.01333418885296567, -4.972402945391593221, -3.997239029220839068 ) ) ;
#16909 = EDGE_LOOP ( 'NONE', ( #11762, #2294 ) ) ;
#16910 = ADVANCED_FACE ( 'NONE', ( #9827 ), #2131, .F. ) ;
#16911 = CARTESIAN_POINT ( 'NONE',  ( 6.038145268433179780, 5.783741681378160138, -6.194606843114025096 ) ) ;
#16912 = PLANE ( 'NONE',  #3320 ) ;
#16914 = ORIENTED_EDGE ( 'NONE', *, *, #28428, .T. ) ;
#16913 = CARTESIAN_POINT ( 'NONE',  ( -4.436748700219182773, -8.316102859869440422, -1.500000000000000444 ) ) ;
#16915 = LINE ( 'NONE', #27108, #31637 ) ;
#16916 = DIRECTION ( 'NONE',  ( -1.000000000000000000, 0.000000000000000000, 0.000000000000000000 ) ) ;
#16917 = CARTESIAN_POINT ( 'NONE',  ( -2.767073886773234292, -0.6621507858625358400, 1.748408842879327407 ) ) ;
#16918 = CARTESIAN_POINT ( 'NONE',  ( 7.931701155947533444, -9.929036424221253654, -1.000000000000000000 ) ) ;
#16920 = EDGE_LOOP ( 'NONE', ( #26095, #26087, #27314 ) ) ;
#16919 = CARTESIAN_POINT ( 'NONE',  ( 108.0159102312815378, -18.29846548910601101, -4.592014164311896351 ) ) ;
#16921 = CARTESIAN_POINT ( 'NONE',  ( 0.000000000000000000, 0.000000000000000000, 4.137834579201376428 ) ) ;
#16922 = EDGE_CURVE ( 'NONE', #33081, #33059, #20043, .T. ) ;
#16923 = B_SPLINE_CURVE_WITH_KNOTS ( 'NONE', 3,
 ( #3205, #31302, #26101, #5566, #15747, #3059, #8375, #13215, #31, #12721 ),
 .UNSPECIFIED., .F., .F.,
 ( 4, 2, 2, 2, 4 ),
 ( 0.000000000000000000, 0.0003402153055305003082, 0.0006804306110610006163, 0.001020645916591500979, 0.001360861222122001233 ),
 .UNSPECIFIED. ) ;
#16924 = CARTESIAN_POINT ( 'NONE',  ( 4.749760686538667009, 7.892520144992435149, 1.391664247347255134 ) ) ;
#16925 = DIRECTION ( 'NONE',  ( 0.000000000000000000, -0.7071067811865516806, 0.7071067811865434649 ) ) ;
#16926 = CARTESIAN_POINT ( 'NONE',  ( 24.73076886165253185, -17.48512500876796238, -1.500000000000000666 ) ) ;
#16927 = CARTESIAN_POINT ( 'NONE',  ( 0.3749742512057840371, -8.659825570211374668, -5.190538276685897401 ) ) ;
#16928 = ORIENTED_EDGE ( 'NONE', *, *, #2900, .F. ) ;
#16929 = CARTESIAN_POINT ( 'NONE',  ( 0.000000000000000000, 4.762163868918270815, 9.915734732513236338 ) ) ;
#16930 = CARTESIAN_POINT ( 'NONE',  ( 3.499999999999999556, -6.106419733534973027, -3.518755179752868223 ) ) ;
#16931 = CARTESIAN_POINT ( 'NONE',  ( 10.00000000000000000, 5.009999999999999787, 0.000000000000000000 ) ) ;
#16932 = ORIENTED_EDGE ( 'NONE', *, *, #21044, .T. ) ;
#16933 = CARTESIAN_POINT ( 'NONE',  ( 8.923856355840481314, 0.3992388782433658467, -1.500000000000000000 ) ) ;
#16934 = EDGE_CURVE ( 'NONE', #31320, #1139, #30237, .T. ) ;
#16935 = CARTESIAN_POINT ( 'NONE',  ( 2.995361005316267811, -0.2432974174152454927, -1.434016190628302212 ) ) ;
#16936 = VERTEX_POINT ( 'NONE', #19371 ) ;
#16937 = CARTESIAN_POINT ( 'NONE',  ( -17.45597128428593336, -27.93932300454937590, 10.99999999999999822 ) ) ;
#16938 = ADVANCED_FACE ( 'NONE', ( #16847 ), #27044, .F. ) ;
#16939 = ORIENTED_EDGE ( 'NONE', *, *, #32177, .F. ) ;
#16940 = VERTEX_POINT ( 'NONE', #311 ) ;
#16941 = CARTESIAN_POINT ( 'NONE',  ( 10.55147673363119232, -4.208382051008212166, 2.718385644597158812 ) ) ;
#16943 = ORIENTED_EDGE ( 'NONE', *, *, #1372, .F. ) ;
#16942 = CYLINDRICAL_SURFACE ( 'NONE', #27200, 8.500000000000000000 ) ;
#16944 = VERTEX_POINT ( 'NONE', #20537 ) ;
#16945 = CARTESIAN_POINT ( 'NONE',  ( 22.23500000136559507, -1.570731468192933633, -2.892927487894330962 ) ) ;
#16946 = EDGE_CURVE ( 'NONE', #8809, #15458, #31096, .T. ) ;
#16947 = ORIENTED_EDGE ( 'NONE', *, *, #187, .T. ) ;
#16948 = FACE_OUTER_BOUND ( 'NONE', #182, .T. ) ;
#16949 = CARTESIAN_POINT ( 'NONE',  ( 6.038145077921538650, -7.799182446117172596, -3.316258947000939816 ) ) ;
#16951 = ORIENTED_EDGE ( 'NONE', *, *, #20985, .T. ) ;
#16950 = DIRECTION ( 'NONE',  ( 0.000000000000000000, -0.1736481776669307198, 0.9848077530122080203 ) ) ;
#16952 = CARTESIAN_POINT ( 'NONE',  ( 5.612974259723590542, -7.786824029658784063, 2.621729824970357114 ) ) ;
#16953 = CARTESIAN_POINT ( 'NONE',  ( 3.499999999999999556, 6.704570150426983233, 5.172265885002680363 ) ) ;
#16954 = CARTESIAN_POINT ( 'NONE',  ( 24.23500000136559507, -1.570731468192933633, -2.892927487894330074 ) ) ;
#16955 = PLANE ( 'NONE',  #22082 ) ;
#16956 = EDGE_CURVE ( 'NONE', #12143, #15684, #2790, .T. ) ;
#16957 = CARTESIAN_POINT ( 'NONE',  ( 13.54302414779168373, -18.70685303420762935, -5.485967528433938867 ) ) ;
#16958 = CARTESIAN_POINT ( 'NONE',  ( 48.53640747082131668, 22.19355195243385026, 1.508259000770581393 ) ) ;
#16959 = CARTESIAN_POINT ( 'NONE',  ( -50.60000000000000142, -10.96966150227468972, 7.500000000000000000 ) ) ;
#16960 = CARTESIAN_POINT ( 'NONE',  ( 3.063284526839887167, 8.461683424509313767, 2.223716399045601921 ) ) ;
#16961 = DIRECTION ( 'NONE',  ( -1.000000000000000000, 0.000000000000000000, -0.000000000000000000 ) ) ;
#16962 = LINE ( 'NONE', #29188, #662 ) ;
#16963 = DIRECTION ( 'NONE',  ( 1.000000000000000000, -0.000000000000000000, -0.000000000000000000 ) ) ;
#16964 = CARTESIAN_POINT ( 'NONE',  ( -4.800050802731187005, -3.113457007523259268, 0.9222479816126455399 ) ) ;
#16965 = EDGE_LOOP ( 'NONE', ( #9209, #3435, #32358, #1453 ) ) ;
#16966 = CARTESIAN_POINT ( 'NONE',  ( -7.387550801365593500, 0.3701630799359330593, -3.521866450007987037 ) ) ;
#16967 = DIRECTION ( 'NONE',  ( -0.9563911903463312436, 0.000000000000000000, -0.2920888409849436429 ) ) ;
#16968 = EDGE_CURVE ( 'NONE', #2120, #31503, #25374, .T. ) ;
#16969 = DIRECTION ( 'NONE',  ( 0.000000000000000000, -0.9961946980917453232, 0.08715574274766135776 ) ) ;
#16970 = CARTESIAN_POINT ( 'NONE',  ( -2.794738735352966685, 0.000000000000000000, -1.491740999229417941 ) ) ;
#16971 = ORIENTED_EDGE ( 'NONE', *, *, #14637, .T. ) ;
#16972 = DIRECTION ( 'NONE',  ( 1.000000000000000000, 0.000000000000000000, 0.000000000000000000 ) ) ;
#16973 = DIRECTION ( 'NONE',  ( -1.000000000000000000, 0.000000000000000000, 0.000000000000000000 ) ) ;
#16974 = ORIENTED_EDGE ( 'NONE', *, *, #30645, .T. ) ;
#16975 = CARTESIAN_POINT ( 'NONE',  ( 15.99612907445991183, -15.99421271805945288, 1.500000000000000000 ) ) ;
#16976 = DATE_TIME_ROLE ( 'creation_date' ) ;
#16977 = CARTESIAN_POINT ( 'NONE',  ( -2.512942406915326110, -5.022711880624455567E-15, 2.999999999999999556 ) ) ;
#16978 = ORIENTED_EDGE ( 'NONE', *, *, #3036, .F. ) ;
#16979 = LINE ( 'NONE', #22334, #11816 ) ;
#16980 = DIRECTION ( 'NONE',  ( 7.472768010111698665E-18, 0.08715574274766461904, -0.9961946980917449901 ) ) ;
#16981 = CARTESIAN_POINT ( 'NONE',  ( 85.02201553618581897, -4.979580722663584424, -4.215289907568986472 ) ) ;
#16982 = DIRECTION ( 'NONE',  ( 1.000000000000000000, 0.000000000000000000, 0.000000000000000000 ) ) ;
#16983 = DIRECTION ( 'NONE',  ( 0.000000000000000000, -0.9063077870366542665, 0.4226182617406900599 ) ) ;
#16984 = ORIENTED_EDGE ( 'NONE', *, *, #22244, .T. ) ;
#16985 = CARTESIAN_POINT ( 'NONE',  ( 8.960941058736731080, 0.001013528757994727400, 1.090795311548445667 ) ) ;
#16986 = CARTESIAN_POINT ( 'NONE',  ( 23.18045508973794711, -21.93188832360385732, -1.140730425198753117 ) ) ;
#16987 = DIRECTION ( 'NONE',  ( 0.000000000000000000, 0.000000000000000000, -1.000000000000000000 ) ) ;
#16988 = EDGE_CURVE ( 'NONE', #11582, #4684, #21453, .T. ) ;
#16990 = ORIENTED_EDGE ( 'NONE', *, *, #2823, .T. ) ;
#16989 = CARTESIAN_POINT ( 'NONE',  ( 25.67945691304631595, 2.703519047173982948, -1.190363068855617712 ) ) ;
#16991 = CARTESIAN_POINT ( 'NONE',  ( 107.6996442589674956, 19.35565155597525688, -4.612695725900422872 ) ) ;
#16992 = CARTESIAN_POINT ( 'NONE',  ( 0.000000000000000000, 0.000000000000000000, 0.000000000000000000 ) ) ;
#16993 = FACE_OUTER_BOUND ( 'NONE', #2606, .T. ) ;
#16994 = CARTESIAN_POINT ( 'NONE',  ( 25.22852577301904020, 18.96657818733213574, 1.477421824444246967 ) ) ;
#16995 = CARTESIAN_POINT ( 'NONE',  ( -33.00303921916323446, -0.1219419795969449855, 1.272152312594969414 ) ) ;
#16996 = CARTESIAN_POINT ( 'NONE',  ( 7.249760686538667009, -6.226446564517873483, -6.147671362329282019 ) ) ;
#16997 = CARTESIAN_POINT ( 'NONE',  ( 24.50111451137534146, -3.256483526998273983E-15, 2.499999999999998668 ) ) ;
#16998 = FACE_OUTER_BOUND ( 'NONE', #25463, .T. ) ;
#16999 = ORIENTED_EDGE ( 'NONE', *, *, #7167, .T. ) ;
#17000 = DIRECTION ( 'NONE',  ( 7.023442172597814953E-17, 0.8191520442889869136, 0.5735764363510531538 ) ) ;
#17001 = ORIENTED_EDGE ( 'NONE', *, *, #22071, .T. ) ;
#17002 = ADVANCED_FACE ( 'NONE', ( #22856 ), #2996, .F. ) ;
#17003 = CARTESIAN_POINT ( 'NONE',  ( -6.104531657079157014, 0.3127741368606810068, -2.975847129947406522 ) ) ;
#17004 = CARTESIAN_POINT ( 'NONE',  ( 25.61000000136559507, 2.892927487894327410, -1.570731468192931635 ) ) ;
#17005 = EDGE_CURVE ( 'NONE', #18235, #18153, #17852, .T. ) ;
#17006 = CARTESIAN_POINT ( 'NONE',  ( -8.000050800000000351, 0.3701630799359330593, -3.521866450007987037 ) ) ;
#17007 = FACE_OUTER_BOUND ( 'NONE', #17591, .T. ) ;
#17008 = CARTESIAN_POINT ( 'NONE',  ( 23.63572006014529592, -7.640988024200195738, 1.873789191059426429 ) ) ;
#17009 = ORIENTED_EDGE ( 'NONE', *, *, #20097, .T. ) ;
#17010 = FACE_OUTER_BOUND ( 'NONE', #16001, .T. ) ;
#17011 = ORIENTED_EDGE ( 'NONE', *, *, #28175, .T. ) ;
#17012 = DATE_AND_TIME ( #1845, #17820 ) ;
#17013 = CARTESIAN_POINT ( 'NONE',  ( 85.03530313761559967, -5.196410162969478996, 4.006106264926406979 ) ) ;
#17014 = CARTESIAN_POINT ( 'NONE',  ( 7.331643324767637360, -8.426631371196835474, -0.9999999999999997780 ) ) ;
#17015 = DIRECTION ( 'NONE',  ( 0.000000000000000000, 0.000000000000000000, 1.000000000000000000 ) ) ;
#17016 = ORIENTED_EDGE ( 'NONE', *, *, #28298, .T. ) ;
#17017 = ORIENTED_EDGE ( 'NONE', *, *, #16566, .T. ) ;
#17018 = CARTESIAN_POINT ( 'NONE',  ( 6.530491751506348308, 6.216163082443066479, 6.030130624359195224 ) ) ;
#17019 = CARTESIAN_POINT ( 'NONE',  ( -2.262550801365593056, 3.521866450007987037, 0.3701630799359328372 ) ) ;
#17020 = CARTESIAN_POINT ( 'NONE',  ( 24.98499999999999943, 2.486304738420679783, -0.2613211581691337604 ) ) ;
#17021 = CARTESIAN_POINT ( 'NONE',  ( 10.87894471766993654, -15.23741606896315837, -1.754278687356615851 ) ) ;
#17023 = EDGE_LOOP ( 'NONE', ( #32851, #8258, #13074, #13327, #27460 ) ) ;
#17022 = CARTESIAN_POINT ( 'NONE',  ( 3.249999999999999556, 0.000000000000000000, 0.000000000000000000 ) ) ;
#17024 = CARTESIAN_POINT ( 'NONE',  ( -3.787550801365593411, -0.3701630799359326152, 3.521866450007987037 ) ) ;
#17025 = CARTESIAN_POINT ( 'NONE',  ( -34.92557263839314885, 0.5000000000000000000, 2.487612133692613359 ) ) ;
#17026 = DIRECTION ( 'NONE',  ( 0.000000000000000000, -0.7431448254773863615, -0.6691306063588671194 ) ) ;
#17027 = CARTESIAN_POINT ( 'NONE',  ( 108.0633640349745548, -18.98178845726371122, -3.316617650382913229 ) ) ;
#17028 = VERTEX_POINT ( 'NONE', #2635 ) ;
#17030 = VERTEX_POINT ( 'NONE', #15671 ) ;
#17029 = CARTESIAN_POINT ( 'NONE',  ( 4.749760686538667009, -6.139290821770289064, 5.151476664237455871 ) ) ;
#17031 = CARTESIAN_POINT ( 'NONE',  ( 7.249760686538667009, -7.530955069117495349, -2.741043480755002371 ) ) ;
#17032 = CARTESIAN_POINT ( 'NONE',  ( 7.064632879756604034, 8.466096581343480310, 2.210816291636240383 ) ) ;
#17033 = EDGE_CURVE ( 'NONE', #28679, #15781, #17776, .T. ) ;
#17034 = CARTESIAN_POINT ( 'NONE',  ( 25.76000000000000512, 2.749440278475487442, 1.299952413566024756 ) ) ;
#17035 = EDGE_CURVE ( 'NONE', #2302, #30719, #29448, .T. ) ;
#17036 = CARTESIAN_POINT ( 'NONE',  ( -27.63096596336819744, 17.00757181511110971, 1.808020238517759282 ) ) ;
#17037 = CYLINDRICAL_SURFACE ( 'NONE', #25260, 0.5000000000000004441 ) ;
#17038 = DIRECTION ( 'NONE',  ( 1.000000000000000000, -0.000000000000000000, -0.000000000000000000 ) ) ;
#17039 = CARTESIAN_POINT ( 'NONE',  ( 68.94677942531217241, -3.651108094209274846, 1.873789666860799619 ) ) ;
#17040 = DIRECTION ( 'NONE',  ( 0.000000000000000000, 0.000000000000000000, -1.000000000000000000 ) ) ;
#17041 = VERTEX_POINT ( 'NONE', #12798 ) ;
#17042 = CARTESIAN_POINT ( 'NONE',  ( 101.6829671662719790, -2.333289718345304298, 3.084778200030451334 ) ) ;
#17043 = ORIENTED_EDGE ( 'NONE', *, *, #13272, .F. ) ;
#17044 = VECTOR ( 'NONE', #2456, 1000.000000000000000 ) ;
#17045 = VECTOR ( 'NONE', #25628, 1000.000000000000000 ) ;
#17046 = DIRECTION ( 'NONE',  ( -0.000000000000000000, -0.000000000000000000, -1.000000000000000000 ) ) ;
#17047 = DIRECTION ( 'NONE',  ( -0.3902696869428256554, -0.9207005872994481477, -5.986714400036072000E-18 ) ) ;
#17048 = DIRECTION ( 'NONE',  ( -0.000000000000000000, -0.4226182617407029940, -0.9063077870366482713 ) ) ;
#17049 = DIRECTION ( 'NONE',  ( 1.000000000000000000, -8.574039729943018344E-17, -0.000000000000000000 ) ) ;
#17050 = ORIENTED_EDGE ( 'NONE', *, *, #8631, .F. ) ;
#17051 = VECTOR ( 'NONE', #26136, 1000.000000000000000 ) ;
#17052 = DIRECTION ( 'NONE',  ( -0.000000000000000000, -0.000000000000000000, -1.000000000000000000 ) ) ;
#17054 = EDGE_LOOP ( 'NONE', ( #9212, #27169, #7121 ) ) ;
#17053 = B_SPLINE_CURVE_WITH_KNOTS ( 'NONE', 3,
 ( #18651, #18836, #312, #18506 ),
 .UNSPECIFIED., .F., .F.,
 ( 4, 4 ),
 ( 2.152606690576576400E-07, 0.0003940451885343313073 ),
 .UNSPECIFIED. ) ;
#17055 = DIRECTION ( 'NONE',  ( 0.4999999999999977240, 0.8660254037844398178, 0.000000000000000000 ) ) ;
#17057 = VERTEX_POINT ( 'NONE', #12500 ) ;
#17056 = CARTESIAN_POINT ( 'NONE',  ( 40.87774081726615094, -5.750296118533150924, -3.995970210918201815 ) ) ;
#17058 = ORIENTED_EDGE ( 'NONE', *, *, #11940, .T. ) ;
#17059 = CARTESIAN_POINT ( 'NONE',  ( 23.25111450864416085, -3.256483526998273983E-15, 2.499999999999998668 ) ) ;
#17060 = CARTESIAN_POINT ( 'NONE',  ( 23.61632761765384458, -8.296864917636222359, -2.713652344655542059 ) ) ;
#17062 = ORIENTED_EDGE ( 'NONE', *, *, #7854, .T. ) ;
#17061 = CARTESIAN_POINT ( 'NONE',  ( 107.4500373638809947, -17.36019379023286646, 4.522129901861156931 ) ) ;
#17063 = CARTESIAN_POINT ( 'NONE',  ( 21.28505181527162904, 16.92208734359699562, -1.500000000000000000 ) ) ;
#17064 = CARTESIAN_POINT ( 'NONE',  ( 22.36000000000000298, -1.573300977624594976, 1.942864903642425700 ) ) ;
#17065 = CARTESIAN_POINT ( 'NONE',  ( -3.729005870813945744, -1.848196750359484497, 1.499999999999999112 ) ) ;
#17066 = CARTESIAN_POINT ( 'NONE',  ( 8.305304940806125913, -2.146676032413550761, -1.000000000000000000 ) ) ;
#17068 = ORIENTED_EDGE ( 'NONE', *, *, #10774, .F. ) ;
#17067 = CARTESIAN_POINT ( 'NONE',  ( 108.0129365102922918, -18.25564464663832354, -5.138066728956478535 ) ) ;
#17069 = CARTESIAN_POINT ( 'NONE',  ( 3.063284526842894540, -6.772677083981750279, 5.538577986799005259 ) ) ;
#17070 = CIRCLE ( 'NONE', #552, 10.99999999999999822 ) ;
#17071 = EDGE_CURVE ( 'NONE', #5453, #1564, #28365, .T. ) ;
#17072 = AXIS2_PLACEMENT_3D ( 'NONE', #7954, #18145, #30547 ) ;
#17073 = CARTESIAN_POINT ( 'NONE',  ( 5.377543748152549874, -2.741043480754877582, -7.530955069117540646 ) ) ;
#17074 = CARTESIAN_POINT ( 'NONE',  ( 22.92250000136559862, -1.913930629741527500, 2.363507492473149618 ) ) ;
#17075 = EDGE_CURVE ( 'NONE', #11908, #516, #21146, .T. ) ;
#17076 = CARTESIAN_POINT ( 'NONE',  ( 1.624999999999999778, -5.222868219166785231, -9.680994141368826078 ) ) ;
#17077 = CARTESIAN_POINT ( 'NONE',  ( 21.25111450864416085, -3.256483526998273983E-15, 2.499999999999998668 ) ) ;
#17078 = DIRECTION ( 'NONE',  ( 0.000000000000000000, 0.000000000000000000, -1.000000000000000000 ) ) ;
#17079 = CIRCLE ( 'NONE', #19219, 0.5000000000000004441 ) ;
#17080 =( BOUNDED_CURVE ( )  B_SPLINE_CURVE ( 2, ( #17557, #10199, #15731, #5201, #2695, #12865, #10535, #23088, #506, #2384, #20746 ),
 .UNSPECIFIED., .F., .F. ) 
 B_SPLINE_CURVE_WITH_KNOTS ( ( 3, 2, 2, 2, 2, 3 ),
 ( 0.3728822619934377136, 0.3750000000000000000, 0.3906250000000000000, 0.4062500000000000000, 0.4218750000000000000, 0.4353822619934377136 ),
 .UNSPECIFIED. ) 
 CURVE ( )  GEOMETRIC_REPRESENTATION_ITEM ( )  RATIONAL_B_SPLINE_CURVE ( ( 0.9821626249036857770, 0.9896829947469991673, 1.000000000000000000, 0.9238795325112867385, 1.000000000000000000, 0.9238795325112867385, 1.000000000000000000, 0.9238795325112867385, 1.000000000000000000, 0.9341965377642874602, 0.9821626249036857770 ) ) 
 REPRESENTATION_ITEM ( '' )  );
#17081 = ORIENTED_EDGE ( 'NONE', *, *, #30961, .T. ) ;
#17082 = CARTESIAN_POINT ( 'NONE',  ( 3.499999999999999556, 2.429606751577043422, 5.757344182232919216 ) ) ;
#17083 = EDGE_CURVE ( 'NONE', #21390, #4392, #18120, .T. ) ;
#17084 = FACE_OUTER_BOUND ( 'NONE', #16000, .T. ) ;
#17085 = DIRECTION ( 'NONE',  ( 0.000000000000000000, 0.000000000000000000, -1.000000000000000000 ) ) ;
#17086 = ORIENTED_EDGE ( 'NONE', *, *, #23776, .T. ) ;
#17087 = CARTESIAN_POINT ( 'NONE',  ( 8.930755659325139817, 0.4999999999999980571, -1.500000000000000000 ) ) ;
#17088 = ADVANCED_FACE ( 'NONE', ( #3139 ), #10981, .T. ) ;
#17089 = AXIS2_PLACEMENT_3D ( 'NONE', #157, #10346, #20558 ) ;
#17090 = CARTESIAN_POINT ( 'NONE',  ( 3.406359441062986715, 0.6647459039674445958, -0.7949826693599028049 ) ) ;
#17091 = VERTEX_POINT ( 'NONE', #28699 ) ;
#17092 = CARTESIAN_POINT ( 'NONE',  ( 7.168240634028618885, -7.372423425476283931, 1.000000000000000222 ) ) ;
#17093 = ORIENTED_EDGE ( 'NONE', *, *, #25627, .F. ) ;
#17094 = AXIS2_PLACEMENT_3D ( 'NONE', #18243, #5567, #25951 ) ;
#17095 = VECTOR ( 'NONE', #32638, 1000.000000000000000 ) ;
#17096 = ORIENTED_EDGE ( 'NONE', *, *, #16466, .T. ) ;
#17097 = CARTESIAN_POINT ( 'NONE',  ( 7.249760686538667009, 4.007137495034812424, 6.940565734314612101 ) ) ;
#17098 = PERSON_AND_ORGANIZATION ( #21916, #29615 ) ;
#17100 = VERTEX_POINT ( 'NONE', #21663 ) ;
#17099 = CARTESIAN_POINT ( 'NONE',  ( 6.357667697713671018, -8.557242355892494601, 0.9262207444595624839 ) ) ;
#17101 = EDGE_CURVE ( 'NONE', #12129, #10411, #24165, .T. ) ;
#17102 = ORIENTED_EDGE ( 'NONE', *, *, #5669, .F. ) ;
#17103 = CARTESIAN_POINT ( 'NONE',  ( 21.98500000136559507, -2.892927487894331406, 1.570731468192932523 ) ) ;
#17104 = ORIENTED_EDGE ( 'NONE', *, *, #18267, .F. ) ;
#17106 = AXIS2_PLACEMENT_3D ( 'NONE', #1037, #13570, #10918 ) ;
#17105 = PLANE ( 'NONE',  #19318 ) ;
#17107 = CARTESIAN_POINT ( 'NONE',  ( -4.365512850963738423, -6.230587388684557304, 1.500000000000000000 ) ) ;
#17109 = VERTEX_POINT ( 'NONE', #13634 ) ;
#17108 = CARTESIAN_POINT ( 'NONE',  ( 54.90853374639801388, -4.039626021003738465, -1.873789188464666466 ) ) ;
#17110 = CARTESIAN_POINT ( 'NONE',  ( 3.063284526839887167, 2.223716399045691183, -8.461683424509292450 ) ) ;
#17111 = EDGE_CURVE ( 'NONE', #1705, #24091, #26522, .T. ) ;
#17112 = LINE ( 'NONE', #22309, #18143 ) ;
#17113 = CARTESIAN_POINT ( 'NONE',  ( 22.79750000136559862, 0.3178988483021036315, 3.024605502323848949 ) ) ;
#17114 = DIRECTION ( 'NONE',  ( -1.000000000000000000, 0.000000000000000000, -3.469446951953611033E-15 ) ) ;
#17115 = CIRCLE ( 'NONE', #5396, 2.999999999999999556 ) ;
#17116 = FACE_OUTER_BOUND ( 'NONE', #23638, .T. ) ;
#17117 = DIRECTION ( 'NONE',  ( -1.000000000000000000, 0.000000000000000000, -0.000000000000000000 ) ) ;
#17118 = CARTESIAN_POINT ( 'NONE',  ( -2.096054051514731231, 1.210157370878028882, -1.500000000000000000 ) ) ;
#17119 = EDGE_CURVE ( 'NONE', #4621, #24728, #7564, .T. ) ;
#17120 = AXIS2_PLACEMENT_3D ( 'NONE', #5132, #9964, #1967 ) ;
#17121 = EDGE_CURVE ( 'NONE', #23722, #26388, #18542, .T. ) ;
#17122 = AXIS2_PLACEMENT_3D ( 'NONE', #11614, #21810, #6920 ) ;
#17123 = VECTOR ( 'NONE', #16140, 1000.000000000000000 ) ;
#17124 = LINE ( 'NONE', #16809, #2197 ) ;
#17125 = CARTESIAN_POINT ( 'NONE',  ( 0.7632845268448539278, 8.734705317657757817, 0.4999240074866477257 ) ) ;
#17126 = DIRECTION ( 'NONE',  ( 0.000000000000000000, 0.000000000000000000, 1.000000000000000000 ) ) ;
#17127 = VECTOR ( 'NONE', #22731, 1000.000000000000000 ) ;
#17128 = CARTESIAN_POINT ( 'NONE',  ( 41.44567272411835290, -7.615257740949710197, 4.522129901861163148 ) ) ;
#17129 = ADVANCED_FACE ( 'NONE', ( #11300 ), #11128, .T. ) ;
#17130 = CARTESIAN_POINT ( 'NONE',  ( -6.500050802731188959, -1.549418761218565477, 2.853674364686380471 ) ) ;
#17131 = ORIENTED_EDGE ( 'NONE', *, *, #6928, .T. ) ;
#17132 = CARTESIAN_POINT ( 'NONE',  ( -4.000050800000000351, -2.331437884370912705, 1.887961173149512062 ) ) ;
#17133 = AXIS2_PLACEMENT_3D ( 'NONE', #3185, #23080, #13347 ) ;
#17134 = CARTESIAN_POINT ( 'NONE',  ( 22.61755859552698311, -21.90439257241343185, -1.185952627206551035 ) ) ;
#17135 = CARTESIAN_POINT ( 'NONE',  ( -3.950050802731187360, -2.983565686104819648, -0.3135853898029605791 ) ) ;
#17136 = ORIENTED_EDGE ( 'NONE', *, *, #7715, .F. ) ;
#17137 = CARTESIAN_POINT ( 'NONE',  ( -12.44989959798873791, 0.000000000000000000, -0.9987809114023521451 ) ) ;
#17138 = DIRECTION ( 'NONE',  ( -0.000000000000000000, -0.000000000000000000, -1.000000000000000000 ) ) ;
#17139 = EDGE_CURVE ( 'NONE', #26968, #5714, #19311, .T. ) ;
#17140 = ORIENTED_EDGE ( 'NONE', *, *, #26153, .F. ) ;
#17141 = CARTESIAN_POINT ( 'NONE',  ( 101.7460807238309570, -3.242109246518175336, -4.282234000298882570 ) ) ;
#17142 = APPLICATION_PROTOCOL_DEFINITION ( 'international standard', 'config_control_design', 1994, #25059 ) ;
#17143 = AXIS2_PLACEMENT_3D ( 'NONE', #7780, #15120, #10597 ) ;
#17144 = CARTESIAN_POINT ( 'NONE',  ( 5.489344087273876127, 5.297876218488320355, 6.152099123112469314 ) ) ;
#17145 = B_SPLINE_CURVE_WITH_KNOTS ( 'NONE', 3,
 ( #28001, #5100, #22807, #15427, #73, #10261, #5601, #28150, #2948, #17608, #25478, #33012, #7772, #25638, #30998, #27812, #10587, #25326, #4928, #2435, #20792, #22958, #5252, #8080, #2753, #10084, #12928, #12753, #15609, #23151, #15783, #20646, #23450, #23307 ),
 .UNSPECIFIED., .F., .F.,
 ( 4, 2, 2, 2, 2, 2, 2, 2, 2, 2, 2, 2, 2, 2, 2, 2, 4 ),
 ( 0.000000000000000000, 0.001968049515999117927, 0.003936099031998235853, 0.004920123789997794816, 0.005904148547997353780, 0.006888173305996912743, 0.007872198063996471706, 0.009840247579995589633, 0.01180829709599470756, 0.01279232185399426652, 0.01377634661199382549, 0.01574439612799293994, 0.01771244564399205440, 0.01968049515999117233, 0.02361659419198941165, 0.02755269322398765097, 0.03148879225598588683 ),
 .UNSPECIFIED. ) ;
#17146 = ORIENTED_EDGE ( 'NONE', *, *, #2015, .F. ) ;
#17147 = CARTESIAN_POINT ( 'NONE',  ( -3.727408454243656077, -1.844569501927837862, 1.499999999999999778 ) ) ;
#17148 = VECTOR ( 'NONE', #30345, 1000.000000000000000 ) ;
#17149 = CIRCLE ( 'NONE', #30544, 10.94895958125474245 ) ;
#17150 = ADVANCED_FACE ( 'NONE', ( #8618 ), #18505, .F. ) ;
#17151 = FACE_OUTER_BOUND ( 'NONE', #775, .T. ) ;
#17152 = CARTESIAN_POINT ( 'NONE',  ( 40.88155443526453325, -6.447799953488541291, -4.312042181587000478 ) ) ;
#17153 = AXIS2_PLACEMENT_3D ( 'NONE', #18606, #14234, #13586 ) ;
#17154 = CARTESIAN_POINT ( 'NONE',  ( 10.55147673363119232, -2.376879293651037006, -4.116875700062107235 ) ) ;
#17155 = ORIENTED_EDGE ( 'NONE', *, *, #29211, .F. ) ;
#17156 = FACE_OUTER_BOUND ( 'NONE', #21857, .T. ) ;
#17157 = EDGE_CURVE ( 'NONE', #11133, #2614, #26664, .T. ) ;
#17158 = DIRECTION ( 'NONE',  ( -0.000000000000000000, -0.000000000000000000, -1.000000000000000000 ) ) ;
#17159 = DIRECTION ( 'NONE',  ( -0.000000000000000000, 0.000000000000000000, 1.000000000000000000 ) ) ;
#17160 = AXIS2_PLACEMENT_3D ( 'NONE', #11984, #4622, #4470 ) ;
#17161 = AXIS2_PLACEMENT_3D ( 'NONE', #27806, #27994, #23300 ) ;
#17163 = VERTEX_POINT ( 'NONE', #1290 ) ;
#17162 = CARTESIAN_POINT ( 'NONE',  ( 10.00000000000000000, -1.115095498423275933, -4.884328206559848340 ) ) ;
#17164 = CARTESIAN_POINT ( 'NONE',  ( 108.1960732670208216, 19.26997324246910992, -4.614321361849309966 ) ) ;
#17165 = CARTESIAN_POINT ( 'NONE',  ( 17.41559371906258136, 18.02474698348857274, 1.500000000000000000 ) ) ;
#17166 = DIRECTION ( 'NONE',  ( 0.000000000000000000, -1.000000000000000000, -5.782411586589358822E-15 ) ) ;
#17167 = CARTESIAN_POINT ( 'NONE',  ( -0.2059365608663963898, 0.000000000000000000, 4.148259000770580407 ) ) ;
#17168 = CARTESIAN_POINT ( 'NONE',  ( 0.000000000000000000, 0.000000000000000000, 0.000000000000000000 ) ) ;
#17169 = EDGE_CURVE ( 'NONE', #596, #32538, #17179, .T. ) ;
#17170 = ADVANCED_FACE ( 'NONE', ( #949 ), #21026, .T. ) ;
#17171 = LINE ( 'NONE', #11825, #31657 ) ;
#17172 = CARTESIAN_POINT ( 'NONE',  ( 6.038145268433180668, -6.194606843114042860, -5.783741681378140598 ) ) ;
#17173 = CARTESIAN_POINT ( 'NONE',  ( -2.512942406915326110, -5.022711880624455567E-15, 2.999999999999999556 ) ) ;
#17174 = CARTESIAN_POINT ( 'NONE',  ( 6.749760686538667009, 0.000000000000000000, 5.000000000000000000 ) ) ;
#17175 = ORIENTED_EDGE ( 'NONE', *, *, #23302, .T. ) ;
#17176 = CIRCLE ( 'NONE', #7559, 0.4999999999999995559 ) ;
#17177 = CARTESIAN_POINT ( 'NONE',  ( 5.489321606599602887, 2.678948506461329426, 7.664118171219008069 ) ) ;
#17178 = ORIENTED_EDGE ( 'NONE', *, *, #1034, .F. ) ;
#17179 = CIRCLE ( 'NONE', #14491, 8.749000000000002331 ) ;
#17180 = VECTOR ( 'NONE', #7062, 1000.000000000000000 ) ;
#17181 = CARTESIAN_POINT ( 'NONE',  ( -5.504531657079157370, -2.975847129947406522, -0.3127741368606805072 ) ) ;
#17182 = CARTESIAN_POINT ( 'NONE',  ( 25.11000000136559507, -2.892927487894331406, 1.570731468192932301 ) ) ;
#17183 = AXIS2_PLACEMENT_3D ( 'NONE', #11197, #13852, #31300 ) ;
#17184 = CARTESIAN_POINT ( 'NONE',  ( 29.32519546910713970, -5.313460878238872809, -5.695980980372493008 ) ) ;
#17185 = DIRECTION ( 'NONE',  ( -0.000000000000000000, -0.3746065934159164001, 0.9271838545667856479 ) ) ;
#17186 = CARTESIAN_POINT ( 'NONE',  ( 25.91108971418532292, 23.29498995882573098, 2.334455007174183194 ) ) ;
#17187 = AXIS2_PLACEMENT_3D ( 'NONE', #4045, #26759, #32124 ) ;
#17188 = VERTEX_POINT ( 'NONE', #3621 ) ;
#17189 = CARTESIAN_POINT ( 'NONE',  ( -23.54713438637982748, 12.65740340961132304, 3.359978791489319772 ) ) ;
#17190 = CONICAL_SURFACE ( 'NONE', #2803, 9.500000000000003553, 0.1919862177193767117 ) ;
#17191 = ADVANCED_FACE ( 'NONE', ( #13781 ), #23568, .F. ) ;
#17192 = AXIS2_PLACEMENT_3D ( 'NONE', #3235, #7331, #25038 ) ;
#17193 = APPROVAL ( #7362, 'UNSPECIFIED' ) ;
#17194 = EDGE_LOOP ( 'NONE', ( #5841, #2137 ) ) ;
#17195 = APPROVAL_STATUS ( 'not_yet_approved' ) ;
#17196 = CARTESIAN_POINT ( 'NONE',  ( 28.66416261876312532, -6.762916490609137021, 3.997238537448035700 ) ) ;
#17197 = DIRECTION ( 'NONE',  ( 1.000000000000000000, 0.000000000000000000, 0.000000000000000000 ) ) ;
#17198 = AXIS2_PLACEMENT_3D ( 'NONE', #1329, #14314, #11161 ) ;
#17200 = CARTESIAN_POINT ( 'NONE',  ( 3.249999999999999556, 8.734705317681626724, -0.4999240074894737984 ) ) ;
#17199 = CARTESIAN_POINT ( 'NONE',  ( 5.489344046532321109, 7.082516960462315048, 3.969101778623947308 ) ) ;
#17201 = B_SPLINE_CURVE_WITH_KNOTS ( 'NONE', 3,
 ( #10404, #2914, #30666, #3210, #10224, #28272, #20446, #15573, #25956, #7740, #3065, #18431, #15396, #23588, #15752, #23110, #25788, #23278, #10554, #30966, #13220, #23420, #527, #19536, #23910, #22206, #27386, #4313, #5857, #24514, #1019, #11052, #8708, #32261, #31450, #9322, #12010, #19691, #23761, #16043, #22040, #8527, #1828, #11203 ),
 .UNSPECIFIED., .F., .F.,
 ( 4, 2, 2, 2, 2, 2, 2, 2, 2, 2, 2, 2, 2, 2, 2, 2, 2, 2, 2, 2, 2, 4 ),
 ( 0.000000000000000000, 0.0006857049238397940321, 0.001371409847679588064, 0.002742819695359173960, 0.003428524619198961704, 0.004114229543038749014, 0.004799934466878537191, 0.005485639390718325369, 0.006857049238397909530, 0.008228459086077491089, 0.009599868933757074382, 0.01028557385759686950, 0.01097127878143666288, 0.01234268862911625485, 0.01371409847679585028, 0.01508550832447544225, 0.01645691817215503422, 0.01782832801983462792, 0.01919973786751422162, 0.01988544279135401674, 0.02057114771519381533, 0.02194255756287339515 ),
 .UNSPECIFIED. ) ;
#17202 = CIRCLE ( 'NONE', #30570, 15.00000000000000355 ) ;
#17203 = ORIENTED_EDGE ( 'NONE', *, *, #25449, .F. ) ;
#17204 = AXIS2_PLACEMENT_3D ( 'NONE', #15248, #42, #25793 ) ;
#17205 = DIRECTION ( 'NONE',  ( 0.000000000000000000, 0.000000000000000000, -1.000000000000000000 ) ) ;
#17206 = CARTESIAN_POINT ( 'NONE',  ( 7.064423659272769385, -7.906491560605053870, -3.748318449931996810 ) ) ;
#17207 = ADVANCED_FACE ( 'NONE', ( #13946 ), #11468, .F. ) ;
#17208 = AXIS2_PLACEMENT_3D ( 'NONE', #5430, #8092, #28991 ) ;
#17209 = CARTESIAN_POINT ( 'NONE',  ( 25.86000000136559862, 1.570731468192929858, 2.892927487894329186 ) ) ;
#17210 = VECTOR ( 'NONE', #21508, 1000.000000000000000 ) ;
#17211 = CARTESIAN_POINT ( 'NONE',  ( 2.040402999919812110, -10.88381885264265492, -1.762032186063900108 ) ) ;
#17213 = ORIENTED_EDGE ( 'NONE', *, *, #32889, .T. ) ;
#17212 = CARTESIAN_POINT ( 'NONE',  ( 0.2678094507063553675, -7.640026513854723866, 1.500000000000000444 ) ) ;
#17214 = CARTESIAN_POINT ( 'NONE',  ( -3.687550801365593323, -2.752080473201636845, 2.228590825266444586 ) ) ;
#17215 = DIRECTION ( 'NONE',  ( -1.000000000000000000, 0.000000000000000000, 0.000000000000000000 ) ) ;
#17216 = ADVANCED_FACE ( 'NONE', ( #14630 ), #27509, .T. ) ;
#17217 = CIRCLE ( 'NONE', #27356, 0.5000000000000000000 ) ;
#17218 = CARTESIAN_POINT ( 'NONE',  ( -59.75626822162180218, -5.804869634004078627, 5.128141679950119602 ) ) ;
#17219 = CARTESIAN_POINT ( 'NONE',  ( 7.249760686538667009, -2.741043480754877582, -7.530955069117540646 ) ) ;
#17220 = TOROIDAL_SURFACE ( 'NONE', #148, 5.587650971692158741, 0.4500000000000000111 ) ;
#17221 = ORIENTED_EDGE ( 'NONE', *, *, #28804, .F. ) ;
#17223 = EDGE_LOOP ( 'NONE', ( #20143, #28509, #5461, #3094 ) ) ;
#17222 = CARTESIAN_POINT ( 'NONE',  ( 21.04767255914985213, -17.06392231637775225, 1.500000000000857314 ) ) ;
#17224 = CIRCLE ( 'NONE', #4966, 0.5000000000000000000 ) ;
#17225 = FACE_OUTER_BOUND ( 'NONE', #12589, .T. ) ;
#17226 = DIRECTION ( 'NONE',  ( -0.000000000000000000, -0.000000000000000000, -1.000000000000000000 ) ) ;
#17227 = CARTESIAN_POINT ( 'NONE',  ( -17.08382165986120071, 13.10789634492833855, 1.904575337205325125 ) ) ;
#17228 = AXIS2_PLACEMENT_3D ( 'NONE', #690, #8851, #11188 ) ;
#17229 = DIRECTION ( 'NONE',  ( -1.000000000000000000, 0.000000000000000000, 0.000000000000000000 ) ) ;
#17230 = CARTESIAN_POINT ( 'NONE',  ( 14.56325452644739649, -20.55228321368884892, -1.750894134686189041 ) ) ;
#17231 = AXIS2_PLACEMENT_3D ( 'NONE', #3947, #29174, #29511 ) ;
#17232 = DIRECTION ( 'NONE',  ( -0.000000000000000000, -0.3746065934159164001, 0.9271838545667856479 ) ) ;
#17233 = B_SPLINE_SURFACE_WITH_KNOTS ( 'NONE', 3, 3, ( 
 ( #322, #8320, #23851, #8630, #10993, #16326, #816 ),
 ( #3007, #18517, #28710, #21194, #13647, #30908, #31392 ),
 ( #31247, #26047, #23361, #468, #28378, #16161, #13160 ),
 ( #8467, #18664, #3491, #13007, #15981, #29052, #28863 ) ),
 .UNSPECIFIED., .F., .F., .F.,
 ( 4, 4 ),
 ( 4, 3, 4 ),
 ( -7.601402592587692883E-13, 1.000000000000000444 ),
 ( 0.003594141869012155120, 0.5017970709346459834, 1.000000000000279776 ),
 .UNSPECIFIED. ) ;
#17234 = CIRCLE ( 'NONE', #9195, 0.5000000000000000000 ) ;
#17235 = AXIS2_PLACEMENT_3D ( 'NONE', #7937, #5436, #5760 ) ;
#17236 = CARTESIAN_POINT ( 'NONE',  ( 102.2339617642406182, -1.281710854345167849, 1.169950773171794633 ) ) ;
#17237 = DIRECTION ( 'NONE',  ( 2.219124775574910312E-17, 0.2588190451025183525, 0.9659258262890689783 ) ) ;
#17238 = VERTEX_POINT ( 'NONE', #22485 ) ;
#17239 = LINE ( 'NONE', #12203, #13966 ) ;
#17240 = ORIENTED_EDGE ( 'NONE', *, *, #30553, .F. ) ;
#17241 = AXIS2_PLACEMENT_3D ( 'NONE', #8494, #6482, #16502 ) ;
#17242 = TOROIDAL_SURFACE ( 'NONE', #2855, 6.000000000000000000, 2.750000000000000444 ) ;
#17243 = DIRECTION ( 'NONE',  ( -0.9842544651762054064, 0.1767573132311699990, 0.000000000000000000 ) ) ;
#17244 = AXIS2_PLACEMENT_3D ( 'NONE', #17555, #12863, #10197 ) ;
#17245 = CARTESIAN_POINT ( 'NONE',  ( 2.437082531750072167, 7.214115859539331765, -7.858345965138702205 ) ) ;
#17246 = EDGE_LOOP ( 'NONE', ( #1573, #8113, #1628, #15648 ) ) ;
#17247 = CIRCLE ( 'NONE', #24613, 1.799999999999977396 ) ;
#17248 = DIRECTION ( 'NONE',  ( 0.000000000000000000, 0.000000000000000000, -1.000000000000000000 ) ) ;
#17249 = VERTEX_POINT ( 'NONE', #17125 ) ;
#17250 = CARTESIAN_POINT ( 'NONE',  ( 0.000000000000000000, 0.000000000000000000, 0.000000000000000000 ) ) ;
#17252 = ORIENTED_EDGE ( 'NONE', *, *, #31170, .T. ) ;
#17251 = CARTESIAN_POINT ( 'NONE',  ( 69.01403922547133618, -4.986533802114832881, -4.018750763356134570 ) ) ;
#17253 = ORIENTED_EDGE ( 'NONE', *, *, #3841, .F. ) ;
#17254 = EDGE_CURVE ( 'NONE', #19445, #15207, #24112, .T. ) ;
#17255 = CARTESIAN_POINT ( 'NONE',  ( 2.556102741905670328, -8.982703267213965503, 5.229406529225562039 ) ) ;
#17256 = EDGE_CURVE ( 'NONE', #15940, #2042, #26257, .T. ) ;
#17257 = CARTESIAN_POINT ( 'NONE',  ( 41.43369393131070666, -3.642920876114435824, 2.713652344655541615 ) ) ;
#17259 = ORIENTED_EDGE ( 'NONE', *, *, #5503, .T. ) ;
#17258 = CARTESIAN_POINT ( 'NONE',  ( 2.040255037894282530, -16.78712277524563490, -1.499999999999999334 ) ) ;
#17260 = AXIS2_PLACEMENT_3D ( 'NONE', #4486, #10475, #8302 ) ;
#17261 = DIRECTION ( 'NONE',  ( 1.000000000000000000, 0.000000000000000000, 0.000000000000000000 ) ) ;
#17262 = CARTESIAN_POINT ( 'NONE',  ( 2.655375060943963472, -12.56041828387959747, -1.000000000000000000 ) ) ;
#17263 = EDGE_CURVE ( 'NONE', #29923, #16893, #30025, .T. ) ;
#17264 = CIRCLE ( 'NONE', #16173, 2.099999999999990319 ) ;
#17265 = CARTESIAN_POINT ( 'NONE',  ( 0.000000000000000000, 10.82112760146736186, 1.975651141462277272 ) ) ;
#17266 = VECTOR ( 'NONE', #27166, 1000.000000000000000 ) ;
#17267 = CARTESIAN_POINT ( 'NONE',  ( 7.637044425070966369, -3.948987408479414096, -1.500000000000000888 ) ) ;
#17269 = ORIENTED_EDGE ( 'NONE', *, *, #25349, .T. ) ;
#17268 = CARTESIAN_POINT ( 'NONE',  ( 107.5605230035171189, -18.96547504619710267, -4.568439005055447311 ) ) ;
#17270 = CARTESIAN_POINT ( 'NONE',  ( 2.976845773540287787, -8.532418605434708425, -3.349682859779589350 ) ) ;
#17271 = VECTOR ( 'NONE', #9792, 1000.000000000000227 ) ;
#17272 = CONICAL_SURFACE ( 'NONE', #32219, 2.099999999999997868, 1.029744258676653423 ) ;
#17273 = CARTESIAN_POINT ( 'NONE',  ( 4.749760686538667009, 5.151476664237558900, -6.139290821770204687 ) ) ;
#17274 = DIRECTION ( 'NONE',  ( 0.000000000000000000, 0.000000000000000000, -1.000000000000000000 ) ) ;
#17275 = LOCAL_TIME ( 16, 7, 10.00000000000000000, #204 ) ;
#17276 = CARTESIAN_POINT ( 'NONE',  ( 107.7876430002164909, 19.84562591318736224, -3.565951703812070495 ) ) ;
#17277 = CARTESIAN_POINT ( 'NONE',  ( 7.249760686538667009, 7.892520144992435149, 1.391664247347255134 ) ) ;
#17278 = ORIENTED_EDGE ( 'NONE', *, *, #10528, .T. ) ;
#17279 = CARTESIAN_POINT ( 'NONE',  ( 5.377543748152549874, -4.007137495034861274, 6.940565734314584567 ) ) ;
#17280 = DIRECTION ( 'NONE',  ( 0.000000000000000000, 1.000000000000000000, 0.000000000000000000 ) ) ;
#17281 = CARTESIAN_POINT ( 'NONE',  ( -7.993687720252830253, 3.540685504229389213, 0.1911117393897334982 ) ) ;
#17282 = VERTEX_POINT ( 'NONE', #9281 ) ;
#17283 = VECTOR ( 'NONE', #31485, 1000.000000000000000 ) ;
#17284 = CARTESIAN_POINT ( 'NONE',  ( 6.530491712438075247, 7.792522225867695163, -3.778856441136638544 ) ) ;
#17285 = FACE_OUTER_BOUND ( 'NONE', #24140, .T. ) ;
#17287 = VERTEX_POINT ( 'NONE', #12273 ) ;
#17286 = AXIS2_PLACEMENT_3D ( 'NONE', #19621, #12093, #19289 ) ;
#17288 = CARTESIAN_POINT ( 'NONE',  ( -7.000050800000000351, 0.000000000000000000, -6.000000000000000888 ) ) ;
#17289 = ORIENTED_EDGE ( 'NONE', *, *, #6392, .T. ) ;
#17290 = CIRCLE ( 'NONE', #14074, 6.248999999999999666 ) ;
#17291 = ADVANCED_FACE ( 'NONE', ( #7114 ), #24983, .T. ) ;
#17292 = ORIENTED_EDGE ( 'NONE', *, *, #7361, .T. ) ;
#17293 = CARTESIAN_POINT ( 'NONE',  ( 3.499999999999999556, -4.724769925181202090, 4.089810527897741466 ) ) ;
#17295 = ORIENTED_EDGE ( 'NONE', *, *, #15588, .F. ) ;
#17294 = DIRECTION ( 'NONE',  ( -0.1327696077594705815, 0.9911469271785068313, 0.000000000000000000 ) ) ;
#17296 = ORIENTED_EDGE ( 'NONE', *, *, #15320, .F. ) ;
#17297 = CARTESIAN_POINT ( 'NONE',  ( 21.23500000136559507, -1.570731468192933633, -2.892927487894330962 ) ) ;
#17298 = CC_DESIGN_APPROVAL ( #9842, ( #31711 ) ) ;
#17299 = VERTEX_POINT ( 'NONE', #32378 ) ;
#17300 = LINE ( 'NONE', #27495, #19934 ) ;
#17302 = ORIENTED_EDGE ( 'NONE', *, *, #183, .F. ) ;
#17301 = CARTESIAN_POINT ( 'NONE',  ( 23.85260150830463033, -3.857138523344298076, -1.873789191062679160 ) ) ;
#17303 = DIRECTION ( 'NONE',  ( -1.000000000000000000, -0.000000000000000000, -0.000000000000000000 ) ) ;
#17304 = DIRECTION ( 'NONE',  ( -7.023442172597859327E-17, -0.8191520442889911324, 0.5735764363510470476 ) ) ;
#17305 = CARTESIAN_POINT ( 'NONE',  ( 24.04750000136559507, -3.024605502323851169, 0.3178988483021052969 ) ) ;
#17306 = LINE ( 'NONE', #20490, #14064 ) ;
#17307 =( BOUNDED_SURFACE ( )  B_SPLINE_SURFACE ( 3, 2, ( 
 ( #9906, #1104, #7066 ),
 ( #17276, #4573, #14897 ),
 ( #25101, #8794, #14748 ),
 ( #16457, #30165, #7238 ) ),
 .UNSPECIFIED., .F., .F., .F. ) 
 B_SPLINE_SURFACE_WITH_KNOTS ( ( 4, 4 ),
 ( 3, 3 ),
 ( -1.734723475976807094E-18, 0.003477590727840301505 ),
 ( 0.000000000000000000, 1.000000000000000000 ),
 .UNSPECIFIED. ) 
 GEOMETRIC_REPRESENTATION_ITEM ( )  RATIONAL_B_SPLINE_SURFACE ( (
 ( 1.000000000000000000, 0.7044453589051415943, 1.000000000000000000),
 ( 1.000000000000000000, 0.7044500455794215910, 1.000000000000000000),
 ( 1.000000000000000000, 0.7044547099241695864, 1.000000000000000000),
 ( 1.000000000000000000, 0.7044593522111741724, 1.000000000000000000) ) ) 
 REPRESENTATION_ITEM ( '' )  SURFACE ( )  );
#17308 = AXIS2_PLACEMENT_3D ( 'NONE', #15896, #15243, #22926 ) ;
#17309 = AXIS2_PLACEMENT_3D ( 'NONE', #21204, #1133, #23712 ) ;
#17310 = CARTESIAN_POINT ( 'NONE',  ( 73.45519860865672968, -21.36028973287419319, -4.522129901861166701 ) ) ;
#17311 = CARTESIAN_POINT ( 'NONE',  ( 33.81874022276149816, 20.00000000000000000, 1.818740222761736414 ) ) ;
#17312 = DIRECTION ( 'NONE',  ( 1.000000000000000000, 0.000000000000000000, -0.000000000000000000 ) ) ;
#17313 = CYLINDRICAL_SURFACE ( 'NONE', #5423, 0.4499999999999990119 ) ;
#17314 = CARTESIAN_POINT ( 'NONE',  ( 41.20585001718148277, -8.497180311781159290, -0.02339150517595086839 ) ) ;
#17315 = DIRECTION ( 'NONE',  ( 0.000000000000000000, -0.2588190451025108030, -0.9659258262890709767 ) ) ;
#17316 = CARTESIAN_POINT ( 'NONE',  ( 35.23476908784419237, -3.791088091780328906, -0.07017451552781628354 ) ) ;
#17317 = LOCAL_TIME ( 16, 7, 10.00000000000000000, #23817 ) ;
#17318 = DIRECTION ( 'NONE',  ( 1.000000000000000000, -0.000000000000000000, 0.000000000000000000 ) ) ;
#17319 = CARTESIAN_POINT ( 'NONE',  ( -3.750050802731187627, 0.3135853898029611342, -2.983565686104819648 ) ) ;
#17320 = ORIENTED_EDGE ( 'NONE', *, *, #21117, .F. ) ;
#17321 = CARTESIAN_POINT ( 'NONE',  ( -8.187550801365594211, 0.3701630799359330593, -3.521866450007987037 ) ) ;
#17322 = EDGE_CURVE ( 'NONE', #16071, #30224, #24638, .T. ) ;
#17323 = CARTESIAN_POINT ( 'NONE',  ( 107.3934749906246111, 17.60820349277802421, -4.075198509582265594 ) ) ;
#17324 = CARTESIAN_POINT ( 'NONE',  ( -4.000050802731187183, -3.113457007523259268, 0.9222479816126455399 ) ) ;
#17325 = ORIENTED_EDGE ( 'NONE', *, *, #13975, .F. ) ;
#17326 = DIRECTION ( 'NONE',  ( 0.000000000000000000, 0.2588190451025115246, 0.9659258262890707547 ) ) ;
#17327 = CIRCLE ( 'NONE', #2954, 8.750000000000000000 ) ;
#17328 = ORIENTED_EDGE ( 'NONE', *, *, #22164, .T. ) ;
#17329 = CARTESIAN_POINT ( 'NONE',  ( 19.80507712518364372, -16.61824031234324295, 1.500000000000000666 ) ) ;
#17330 = ITEM_DEFINED_TRANSFORMATION ( 'NONE', 'NONE', #25800,  #2865 ) ;
#17331 = DIRECTION ( 'NONE',  ( 0.9947025833170223263, 0.1027947991993880261, -0.000000000000000000 ) ) ;
#17333 = ADVANCED_FACE ( 'NONE', ( #9435 ), #24474, .T. ) ;
#17332 = ORIENTED_EDGE ( 'NONE', *, *, #21355, .F. ) ;
#17334 = CARTESIAN_POINT ( 'NONE',  ( 9.096376384877638444, -0.1528062924499160868, -1.364612494264896281 ) ) ;
#17335 = EDGE_CURVE ( 'NONE', #1359, #15940, #4376, .T. ) ;
#17336 = ORIENTED_EDGE ( 'NONE', *, *, #3013, .T. ) ;
#17337 = DIRECTION ( 'NONE',  ( 0.000000000000000000, 0.000000000000000000, -1.000000000000000000 ) ) ;
#17338 = CARTESIAN_POINT ( 'NONE',  ( 9.302055952181044418, 0.2457637073014158069, -1.500000000000004219 ) ) ;
#17339 = CARTESIAN_POINT ( 'NONE',  ( 1.624999999999999778, -4.762163868918343645, 9.915734732513202587 ) ) ;
#17340 = LINE ( 'NONE', #14465, #4306 ) ;
#17341 = VERTEX_POINT ( 'NONE', #1592 ) ;
#17342 = CARTESIAN_POINT ( 'NONE',  ( 0.000000000000000000, 10.76487093102067583, -1.999317321091388377 ) ) ;
#17343 = EDGE_CURVE ( 'NONE', #15916, #20282, #24085, .T. ) ;
#17344 = LINE ( 'NONE', #4791, #191 ) ;
#17346 = VERTEX_POINT ( 'NONE', #32530 ) ;
#17345 = CARTESIAN_POINT ( 'NONE',  ( 0.9232102171129938917, 0.000000000000000000, -4.522129901861164925 ) ) ;
#17347 = DIRECTION ( 'NONE',  ( -1.000000000000000000, -0.000000000000000000, -0.000000000000000000 ) ) ;
#17348 = CARTESIAN_POINT ( 'NONE',  ( 29.41391112839825794, -2.700987858898180161, -0.07017451552781628354 ) ) ;
#17349 = CARTESIAN_POINT ( 'NONE',  ( 107.5617723795401872, -18.98359893170738744, -4.522129901861166701 ) ) ;
#17350 = PLANE ( 'NONE',  #3798 ) ;
#17351 = DIRECTION ( 'NONE',  ( -7.023442172597887676E-17, -0.8191520442889951292, 0.5735764363510412744 ) ) ;
#17352 = EDGE_CURVE ( 'NONE', #5699, #6454, #1442, .T. ) ;
#17353 = CARTESIAN_POINT ( 'NONE',  ( 0.000000000000000000, -7.009698679648292519, 0.7308381473896670144 ) ) ;
#17354 = AXIS2_PLACEMENT_3D ( 'NONE', #4182, #29767, #19416 ) ;
#17355 = CARTESIAN_POINT ( 'NONE',  ( 3.249999999999999556, 6.478011392632891052, 6.807171995660606711 ) ) ;
#17356 = CARTESIAN_POINT ( 'NONE',  ( -56.46106707970686500, 0.01431647023326164565, -1.180353684121977276 ) ) ;
#17357 = CARTESIAN_POINT ( 'NONE',  ( -23.35000000000000142, -10.96966150227469505, 4.000000000000000000 ) ) ;
#17358 = ORIENTED_EDGE ( 'NONE', *, *, #12537, .T. ) ;
#17359 = CARTESIAN_POINT ( 'NONE',  ( -7.077711312404032898E-17, -0.8254815157534933778, -4.681538312723525053 ) ) ;
#17360 = ORIENTED_EDGE ( 'NONE', *, *, #9409, .T. ) ;
#17361 = CARTESIAN_POINT ( 'NONE',  ( -7.154531657079157725, -3.105402419394638791, 0.9198621039125867149 ) ) ;
#17362 = CARTESIAN_POINT ( 'NONE',  ( 108.9718513837279517, 17.93233736012435742, 5.382000289407169902 ) ) ;
#17363 = CARTESIAN_POINT ( 'NONE',  ( 41.43709133142961321, -4.769546740945156849, -4.522129901861162260 ) ) ;
#17364 = CARTESIAN_POINT ( 'NONE',  ( -23.54713438637982748, 8.434582260019382716, 8.205946861809124471 ) ) ;
#17365 = DIRECTION ( 'NONE',  ( -7.472768010111758754E-18, -0.08715574274766552110, 0.9961946980917449901 ) ) ;
#17366 = ORIENTED_EDGE ( 'NONE', *, *, #8981, .T. ) ;
#17367 = CARTESIAN_POINT ( 'NONE',  ( 18.99195638486427384, -3.267134207175613536, 1.527295581757372123 ) ) ;
#17368 = EDGE_CURVE ( 'NONE', #32762, #31355, #24494, .T. ) ;
#17369 = ORIENTED_EDGE ( 'NONE', *, *, #24268, .F. ) ;
#17370 = COORDINATED_UNIVERSAL_TIME_OFFSET ( 0, 0, .AHEAD. ) ;
#17371 = EDGE_CURVE ( 'NONE', #22830, #28234, #24523, .T. ) ;
#17372 = CARTESIAN_POINT ( 'NONE',  ( 40.88393865713020858, -6.886838077535163194, 4.008636882558729297 ) ) ;
#17373 = ADVANCED_FACE ( 'NONE', ( #14132 ), #27010, .F. ) ;
#17374 = CARTESIAN_POINT ( 'NONE',  ( 6.038145208238973716, 4.620191422127224001, -7.104833038995668204 ) ) ;
#17376 = DIRECTION ( 'NONE',  ( 0.000000000000000000, 0.000000000000000000, 1.000000000000000000 ) ) ;
#17375 = CARTESIAN_POINT ( 'NONE',  ( 2.274274201625327230, 0.000000000000000000, 0.000000000000000000 ) ) ;
#17377 = ORIENTED_EDGE ( 'NONE', *, *, #11216, .F. ) ;
#17378 = CARTESIAN_POINT ( 'NONE',  ( -7.550050802731187893, 2.983565686104819648, 0.3135853898029609677 ) ) ;
#17379 = CARTESIAN_POINT ( 'NONE',  ( 7.249760686538667009, -7.906491560603638113, -3.748318449932378282 ) ) ;
#17380 = CARTESIAN_POINT ( 'NONE',  ( 23.61000000136559507, 2.892927487894327410, -1.570731468192931635 ) ) ;
#17381 = CARTESIAN_POINT ( 'NONE',  ( 4.139048519582217089, -11.97498679546279199, -1.500000000000001332 ) ) ;
#17383 = ORIENTED_EDGE ( 'NONE', *, *, #21871, .F. ) ;
#17382 = CARTESIAN_POINT ( 'NONE',  ( -0.7739934281325318022, -8.972773999336984829, 4.522129901861157819 ) ) ;
#17384 = CARTESIAN_POINT ( 'NONE',  ( -2.387550801365593056, 3.521866450007987037, 0.3701630799359328372 ) ) ;
#17385 = CARTESIAN_POINT ( 'NONE',  ( 108.0068349480237515, 18.21621961241920573, -4.398253369385427547 ) ) ;
#17386 = CARTESIAN_POINT ( 'NONE',  ( 2.437082316315974939, -10.59788678609685952, -1.217322776604839785 ) ) ;
#17387 = CARTESIAN_POINT ( 'NONE',  ( 35.29731606331278471, -6.671246578258721804, -3.993434333679743986 ) ) ;
#17388 = ORIENTED_EDGE ( 'NONE', *, *, #6524, .T. ) ;
#17390 = ORIENTED_EDGE ( 'NONE', *, *, #29832, .F. ) ;
#17389 = CARTESIAN_POINT ( 'NONE',  ( 23.72853298629391006, -17.37454644214624722, 1.486007232661737065 ) ) ;
#17391 = ADVANCED_FACE ( 'NONE', ( #4263 ), #20658, .T. ) ;
#17392 = CC_DESIGN_DATE_AND_TIME_ASSIGNMENT ( #8772, #4237, ( #25875 ) ) ;
#17393 = CARTESIAN_POINT ( 'NONE',  ( 24.72695737054825926, 18.91229966141139229, 1.500000000000000000 ) ) ;
#17394 = LINE ( 'NONE', #27587, #23742 ) ;
#17395 = CARTESIAN_POINT ( 'NONE',  ( -18.13299741701835188, 15.72250979567403206, 1.500000000000000222 ) ) ;
#17396 = CARTESIAN_POINT ( 'NONE',  ( -30.49072021768049012, 9.200062826706727037, 1.500000000000000000 ) ) ;
#17397 = CARTESIAN_POINT ( 'NONE',  ( 15.97646417262808072, -20.81271057983140338, -1.751026346894440255 ) ) ;
#17398 = FACE_OUTER_BOUND ( 'NONE', #17893, .T. ) ;
#17399 = CARTESIAN_POINT ( 'NONE',  ( 102.2651039925859209, -1.731228206879544373, 2.184956770111046165 ) ) ;
#17400 = FACE_OUTER_BOUND ( 'NONE', #6068, .T. ) ;
#17401 = ORIENTED_EDGE ( 'NONE', *, *, #15321, .T. ) ;
#17402 = LINE ( 'NONE', #25068, #24154 ) ;
#17403 = ORIENTED_EDGE ( 'NONE', *, *, #26446, .F. ) ;
#17404 = ADVANCED_FACE ( 'NONE', ( #30521 ), #10448, .T. ) ;
#17405 = CARTESIAN_POINT ( 'NONE',  ( -61.24371088333262492, -10.96999999999998643, 1.949999999999999956 ) ) ;
#17406 = CARTESIAN_POINT ( 'NONE',  ( -23.35000000000045262, -10.96966150227483539, 5.010000000000023768 ) ) ;
#17407 = CARTESIAN_POINT ( 'NONE',  ( -31.85000000000000497, -10.96966150227469505, 4.500000000000000888 ) ) ;
#17408 = ORIENTED_EDGE ( 'NONE', *, *, #17786, .F. ) ;
#17409 = CYLINDRICAL_SURFACE ( 'NONE', #2346, 11.00000000000000000 ) ;
#17410 = EDGE_LOOP ( 'NONE', ( #20297, #29464, #14488, #12304 ) ) ;
#17411 = CARTESIAN_POINT ( 'NONE',  ( 0.000000000000000000, 0.000000000000000000, -1.500000000000000000 ) ) ;
#17413 = ORIENTED_EDGE ( 'NONE', *, *, #22773, .T. ) ;
#17412 = CARTESIAN_POINT ( 'NONE',  ( 84.96658996055005275, -4.075471198594033062, -4.018749453393667181 ) ) ;
#17414 = ORIENTED_EDGE ( 'NONE', *, *, #15032, .T. ) ;
#17415 = CARTESIAN_POINT ( 'NONE',  ( -53.12500000000000000, -10.96966150227468972, 7.500000000000000000 ) ) ;
#17416 = FACE_OUTER_BOUND ( 'NONE', #18059, .T. ) ;
#17418 = ORIENTED_EDGE ( 'NONE', *, *, #23501, .T. ) ;
#17417 = CARTESIAN_POINT ( 'NONE',  ( 107.3476768466457401, -15.88628154573096651, 1.500000000000000000 ) ) ;
#17419 = CARTESIAN_POINT ( 'NONE',  ( 107.5617944031221640, -18.98359742639815551, 4.522129901861158707 ) ) ;
#17420 = DIRECTION ( 'NONE',  ( 0.000000000000000000, 0.000000000000000000, 1.000000000000000000 ) ) ;
#17421 = DIRECTION ( 'NONE',  ( -1.000000000000000000, -0.000000000000000000, 0.000000000000000000 ) ) ;
#17422 = DIRECTION ( 'NONE',  ( 0.000000000000000000, 0.000000000000000000, 1.000000000000000000 ) ) ;
#17424 = VERTEX_POINT ( 'NONE', #22816 ) ;
#17423 = CARTESIAN_POINT ( 'NONE',  ( 107.9850792167139275, -17.85450654912270707, -4.471870475959497604 ) ) ;
#17425 = CARTESIAN_POINT ( 'NONE',  ( 22.00639167669143603, -21.80013755708273848, 1.500000000000000000 ) ) ;
#17426 = CARTESIAN_POINT ( 'NONE',  ( 23.11000000136559507, -3.156283516753370044, -0.9349337715887220401 ) ) ;
#17427 = CARTESIAN_POINT ( 'NONE',  ( -8.000050800000000351, 3.673940397442060361E-16, 3.000000000000000444 ) ) ;
#17428 = CARTESIAN_POINT ( 'NONE',  ( 24.55229918076951989, -17.45956433520428774, -1.484437869256384213 ) ) ;
#17429 = LINE ( 'NONE', #22440, #661 ) ;
#17430 = EDGE_LOOP ( 'NONE', ( #23247, #13361, #4860, #3894, #815 ) ) ;
#17431 = CARTESIAN_POINT ( 'NONE',  ( 17.32050807568873552, 10.00000000000002309, 1.500000000000000000 ) ) ;
#17432 = DIRECTION ( 'NONE',  ( -1.000000000000000000, -0.000000000000000000, -0.000000000000000000 ) ) ;
#17433 = EDGE_CURVE ( 'NONE', #14000, #32878, #26124, .T. ) ;
#17434 = CARTESIAN_POINT ( 'NONE',  ( -5.237550801365594033, -3.675193018007245627, 1.088641768524163389 ) ) ;
#17435 = ORIENTED_EDGE ( 'NONE', *, *, #6396, .F. ) ;
#17436 = EDGE_CURVE ( 'NONE', #18851, #32762, #10973, .T. ) ;
#17437 = EDGE_CURVE ( 'NONE', #30219, #22141, #12405, .T. ) ;
#17438 = DIRECTION ( 'NONE',  ( -1.000000000000000000, 0.000000000000000000, 0.000000000000000000 ) ) ;
#17439 = CARTESIAN_POINT ( 'NONE',  ( 3.238981242682563710, 0.6371288015966571905, -1.059614580210906043 ) ) ;
#17440 = EDGE_LOOP ( 'NONE', ( #4351, #2046, #21765, #20426 ) ) ;
#17441 = CARTESIAN_POINT ( 'NONE',  ( 18.93617721851659041, -3.890633339435721982, 4.522129901861162260 ) ) ;
#17442 = EDGE_LOOP ( 'NONE', ( #15951, #24808, #13300, #25106 ) ) ;
#17443 = ORIENTED_EDGE ( 'NONE', *, *, #7480, .T. ) ;
#17444 = FACE_OUTER_BOUND ( 'NONE', #5134, .T. ) ;
#17446 = ORIENTED_EDGE ( 'NONE', *, *, #9360, .T. ) ;
#17445 = CARTESIAN_POINT ( 'NONE',  ( -5.240875073191923583, 0.000000000000000000, -3.405250132838343102 ) ) ;
#17447 = ORIENTED_EDGE ( 'NONE', *, *, #10196, .F. ) ;
#17448 = DIRECTION ( 'NONE',  ( 7.770718973608968796E-17, 0.9063077870366493816, 0.4226182617407006070 ) ) ;
#17449 = ORIENTED_EDGE ( 'NONE', *, *, #24960, .T. ) ;
#17450 = CARTESIAN_POINT ( 'NONE',  ( 0.3045634635876924845, -2.226307684702756529, 10.03290811084030842 ) ) ;
#17452 = VERTEX_POINT ( 'NONE', #33021 ) ;
#17451 = CARTESIAN_POINT ( 'NONE',  ( 0.5309851148689820333, -4.399114163800174282, 1.500000000000000000 ) ) ;
#17453 = LINE ( 'NONE', #32198, #10114 ) ;
#17454 = DIRECTION ( 'NONE',  ( -1.000000000000000000, 8.574039729943018344E-17, -0.000000000000000000 ) ) ;
#17455 = CARTESIAN_POINT ( 'NONE',  ( -7.362942409646514363, 1.214281993118000652E-15, 3.000000000000000000 ) ) ;
#17456 = FACE_OUTER_BOUND ( 'NONE', #18486, .T. ) ;
#17457 = CARTESIAN_POINT ( 'NONE',  ( 107.9497830788478581, -17.34625094442601068, -4.563380564795206595 ) ) ;
#17458 = CARTESIAN_POINT ( 'NONE',  ( 25.48003136492429377, -17.55790038815346676, 1.043845799725922951 ) ) ;
#17459 = CARTESIAN_POINT ( 'NONE',  ( -23.54713438637982748, 10.71031731502107576, 2.573304945315896042 ) ) ;
#17460 = CARTESIAN_POINT ( 'NONE',  ( 35.16139127360178662, -8.400504373793673096, 0.02339150517593243869 ) ) ;
#17461 = DIRECTION ( 'NONE',  ( 0.000000000000000000, 0.000000000000000000, -1.000000000000000000 ) ) ;
#17462 = CARTESIAN_POINT ( 'NONE',  ( 35.23476908784419237, -3.791088091780328906, -0.02339150518254430253 ) ) ;
#17463 = CARTESIAN_POINT ( 'NONE',  ( 0.6728000687364281696, -2.287261066731684611, -8.860258565222334681 ) ) ;
#17464 = EDGE_CURVE ( 'NONE', #22830, #8298, #30574, .T. ) ;
#17465 = CARTESIAN_POINT ( 'NONE',  ( -1.900050802731187316, 2.853674364686379583, 1.549418761218565921 ) ) ;
#17466 = ORIENTED_EDGE ( 'NONE', *, *, #4119, .T. ) ;
#17467 = EDGE_CURVE ( 'NONE', #8185, #1782, #7596, .T. ) ;
#17468 = CARTESIAN_POINT ( 'NONE',  ( -7.987550801365593145, 3.521866450007987037, 0.3701630799359328372 ) ) ;
#17469 = CYLINDRICAL_SURFACE ( 'NONE', #1255, 0.5000000000000004441 ) ;
#17470 = CARTESIAN_POINT ( 'NONE',  ( -6.912942406915326465, 7.727249047114547632E-16, -2.999999999999999556 ) ) ;
#17471 = ORIENTED_EDGE ( 'NONE', *, *, #17371, .T. ) ;
#17472 = CARTESIAN_POINT ( 'NONE',  ( 0.000000000000000000, -5.848742439617962141, 6.167836887840968174 ) ) ;
#17473 = CARTESIAN_POINT ( 'NONE',  ( 7.064423669210280643, -6.147671362330640044, -6.226446564518105298 ) ) ;
#17474 = CARTESIAN_POINT ( 'NONE',  ( 107.9988559483833370, -18.05288805794269535, 4.627775613152216749 ) ) ;
#17475 = ORIENTED_EDGE ( 'NONE', *, *, #18924, .T. ) ;
#17476 = CARTESIAN_POINT ( 'NONE',  ( 12.16199335750468258, -15.44738821017505259, 1.500000000000415668 ) ) ;
#17477 = ITEM_DEFINED_TRANSFORMATION ( 'NONE', 'NONE', #26854,  #2865 ) ;
#17478 = FACE_OUTER_BOUND ( 'NONE', #19545, .T. ) ;
#17479 = EDGE_LOOP ( 'NONE', ( #30928, #9291, #8824, #11507 ) ) ;
#17480 = CARTESIAN_POINT ( 'NONE',  ( 10.00000000000000000, 4.116875700062115229, -2.376879293651021019 ) ) ;
#17481 = ORIENTED_EDGE ( 'NONE', *, *, #27935, .T. ) ;
#17482 =( BOUNDED_CURVE ( )  B_SPLINE_CURVE ( 3, ( #13753, #15942, #26339, #923 ),
 .UNSPECIFIED., .F., .F. ) 
 B_SPLINE_CURVE_WITH_KNOTS ( ( 4, 4 ),
 ( 4.712388980384687009, 6.091199089460269889 ),
 .UNSPECIFIED. ) 
 CURVE ( )  GEOMETRIC_REPRESENTATION_ITEM ( )  RATIONAL_B_SPLINE_CURVE ( ( 1.000000000000000000, 0.8477497222584666758, 0.8477497222584666758, 1.000000000000000000 ) ) 
 REPRESENTATION_ITEM ( '' )  );
#17483 = CARTESIAN_POINT ( 'NONE',  ( 108.0270953819671291, -18.45952887646314977, -4.403827697248457795 ) ) ;
#17484 = CARTESIAN_POINT ( 'NONE',  ( 9.282537329959810180, 0.2172754300396264326, -1.041239158277639021 ) ) ;
#17485 = CARTESIAN_POINT ( 'NONE',  ( 10.00000000000000000, 3.641590349731970822, -3.055657119358763829 ) ) ;
#17486 = DIRECTION ( 'NONE',  ( -7.023442172597786603E-17, -0.8191520442889833609, -0.5735764363510580388 ) ) ;
#17487 = ORIENTED_EDGE ( 'NONE', *, *, #25747, .F. ) ;
#17488 = CARTESIAN_POINT ( 'NONE',  ( 21.63953834185432257, -21.76333864698586140, -1.486663794871770916 ) ) ;
#17489 = CARTESIAN_POINT ( 'NONE',  ( 17.41559371906258136, 18.02474698348859405, -1.491740999229418829 ) ) ;
#17490 = ORIENTED_EDGE ( 'NONE', *, *, #18641, .F. ) ;
#17491 = EDGE_CURVE ( 'NONE', #19087, #26011, #14519, .T. ) ;
#17492 = PRODUCT ( 'Part6_handleknob', 'Part6_handleknob', '', ( #3038 ) ) ;
#17493 = CARTESIAN_POINT ( 'NONE',  ( 26.27358061090003361, 19.78731608622335969, 0.4463807625373084065 ) ) ;
#17494 = CARTESIAN_POINT ( 'NONE',  ( 29.25343337322282622, -7.426690278353109242, 4.522129901861162260 ) ) ;
#17495 = CARTESIAN_POINT ( 'NONE',  ( 0.7632845268448663623, 0.4999240074867329353, -8.734705317657697421 ) ) ;
#17496 = CARTESIAN_POINT ( 'NONE',  ( 101.6833487790503341, -2.338784847420880553, -3.093621779973272812 ) ) ;
#17497 = EDGE_CURVE ( 'NONE', #20265, #23931, #2284, .T. ) ;
#17498 = CARTESIAN_POINT ( 'NONE',  ( 6.037141752603385036, 0.4483113388088468820, 8.462586328878536790 ) ) ;
#17499 = CARTESIAN_POINT ( 'NONE',  ( 7.249760686538667009, 4.007137495034812424, 6.940565734314612101 ) ) ;
#17500 = CARTESIAN_POINT ( 'NONE',  ( -56.32772727923107681, 0.4611123337040696213, -1.500000000000000000 ) ) ;
#17501 = ORIENTED_EDGE ( 'NONE', *, *, #6821, .T. ) ;
#17502 = B_SPLINE_CURVE_WITH_KNOTS ( 'NONE', 3,
 ( #8858, #26587, #19066, #13210, #518, #29920 ),
 .UNSPECIFIED., .F., .F.,
 ( 4, 2, 4 ),
 ( 0.009527197497169513293, 0.5047635987485847853, 1.000000000000000000 ),
 .UNSPECIFIED. ) ;
#17503 = EDGE_CURVE ( 'NONE', #6111, #6331, #4764, .T. ) ;
#17504 = CARTESIAN_POINT ( 'NONE',  ( -5.262550801365593500, -0.3701630799359326152, 3.521866450007987037 ) ) ;
#17505 = ORIENTED_EDGE ( 'NONE', *, *, #16796, .T. ) ;
#17506 = CARTESIAN_POINT ( 'NONE',  ( -7.604531657079157903, 2.325406398514293205, -1.883076972206379374 ) ) ;
#17507 = CARTESIAN_POINT ( 'NONE',  ( 109.1350892575554070, 18.84131025218471578, 5.127064441657748439 ) ) ;
#17508 = EDGE_CURVE ( 'NONE', #28583, #32678, #14938, .T. ) ;
#17509 = CARTESIAN_POINT ( 'NONE',  ( 107.5052154967213482, 18.24033990947258133, 5.057122841292876814 ) ) ;
#17510 = CARTESIAN_POINT ( 'NONE',  ( 2.281627749324421917, -0.2935656086769610207, 1.757435426329174044 ) ) ;
#17511 = DIRECTION ( 'NONE',  ( 0.000000000000000000, 1.000000000000000000, 0.000000000000000000 ) ) ;
#17512 = ORIENTED_EDGE ( 'NONE', *, *, #27240, .F. ) ;
#17513 = CARTESIAN_POINT ( 'NONE',  ( 0.7632845268398871230, -8.461683424509331530, 2.223716399045538861 ) ) ;
#17514 = EDGE_LOOP ( 'NONE', ( #8288, #31277, #10534, #22860 ) ) ;
#17515 = CARTESIAN_POINT ( 'NONE',  ( -34.48223484310472742, 0.5174497483512505713, -2.981930256614258923 ) ) ;
#17516 = PERSON_AND_ORGANIZATION ( #6766, #25292 ) ;
#17517 = EDGE_CURVE ( 'NONE', #21706, #61, #4706, .T. ) ;
#17518 = CARTESIAN_POINT ( 'NONE',  ( 69.07021576803677476, -6.111680664911116168, 4.001041175462015431 ) ) ;
#17519 = CARTESIAN_POINT ( 'NONE',  ( 19.01480233880980819, -3.011762293215293429, -0.07017451552781921176 ) ) ;
#17521 = CARTESIAN_POINT ( 'NONE',  ( -8.000050800000000351, 0.000000000000000000, 0.000000000000000000 ) ) ;
#17520 = CARTESIAN_POINT ( 'NONE',  ( -7.000050800000000351, 0.000000000000000000, 0.000000000000000000 ) ) ;
#17522 = ORIENTED_EDGE ( 'NONE', *, *, #20438, .T. ) ;
#17523 = DIRECTION ( 'NONE',  ( 1.000000000000000000, -0.000000000000000000, -0.000000000000000000 ) ) ;
#17524 = CARTESIAN_POINT ( 'NONE',  ( 0.000000000000000000, 0.000000000000000000, 0.000000000000000000 ) ) ;
#17525 = ADVANCED_FACE ( 'NONE', ( #25086 ), #14374, .T. ) ;
#17526 = CARTESIAN_POINT ( 'NONE',  ( 21.54750000000000654, -2.594547506269383685, -0.7685399846772043020 ) ) ;
#17527 = CARTESIAN_POINT ( 'NONE',  ( 3.335187914516625440, -11.42298369410695535, -1.500000000000000444 ) ) ;
#17529 = ORIENTED_EDGE ( 'NONE', *, *, #17157, .F. ) ;
#17528 = CARTESIAN_POINT ( 'NONE',  ( 6.357667697713671018, 8.557242355892499930, -0.9262207444595036421 ) ) ;
#17530 = CARTESIAN_POINT ( 'NONE',  ( -3.737550801365593589, -1.828967928396026510, 3.368539882008728004 ) ) ;
#17531 = CARTESIAN_POINT ( 'NONE',  ( -50.81000000000000227, -10.96999999999998643, 9.000000000000000000 ) ) ;
#17532 = ADVANCED_FACE ( 'NONE', ( #29796 ), #24424, .F. ) ;
#17533 = CARTESIAN_POINT ( 'NONE',  ( -53.92460539084177640, 5.494498998130930900, 1.240130434009519833 ) ) ;
#17534 = CARTESIAN_POINT ( 'NONE',  ( -32.18314092741314880, -27.93932300454937590, -1.500000000000000000 ) ) ;
#17535 = ORIENTED_EDGE ( 'NONE', *, *, #657, .T. ) ;
#17537 = ORIENTED_EDGE ( 'NONE', *, *, #21148, .F. ) ;
#17536 = CARTESIAN_POINT ( 'NONE',  ( 23.86874014608549288, -17.38228585591217623, 1.471223822905279199 ) ) ;
#17538 = CARTESIAN_POINT ( 'NONE',  ( 18.03711215731073736, 14.23863779149164621, 1.500000000000000222 ) ) ;
#17539 = CARTESIAN_POINT ( 'NONE',  ( 2.795120465740001059, -9.482538569678542473, -2.298374178342494467 ) ) ;
#17540 = ADVANCED_FACE ( 'NONE', ( #14732 ), #22606, .T. ) ;
#17541 = EDGE_CURVE ( 'NONE', #3406, #10158, #16757, .T. ) ;
#17542 = CARTESIAN_POINT ( 'NONE',  ( 24.23500000136559507, -3.156283516753370488, -0.9349337715887220401 ) ) ;
#17543 = CARTESIAN_POINT ( 'NONE',  ( -27.92832289637516041, 5.061405101124985428, 1.500000000000000000 ) ) ;
#17544 = CARTESIAN_POINT ( 'NONE',  ( -0.5878747269098347772, -14.86239685203039862, -1.500000000000000444 ) ) ;
#17545 = DIRECTION ( 'NONE',  ( -4.917867153433080997E-17, -0.5735764363510552633, 0.8191520442889853593 ) ) ;
#17546 = DIRECTION ( 'NONE',  ( -1.000000000000000000, 0.000000000000000000, 0.000000000000000000 ) ) ;
#17547 = LINE ( 'NONE', #27744, #13500 ) ;
#17548 = ORIENTED_EDGE ( 'NONE', *, *, #8146, .F. ) ;
#17549 = ADVANCED_FACE ( 'NONE', ( #27268 ), #3879, .F. ) ;
#17550 = CARTESIAN_POINT ( 'NONE',  ( -7.312942406915325044, -8.831141768130910875E-16, 2.999999999999999556 ) ) ;
#17551 = DIRECTION ( 'NONE',  ( 0.000000000000000000, 0.000000000000000000, 1.000000000000000000 ) ) ;
#17552 = DIRECTION ( 'NONE',  ( 8.574039729943018344E-17, 1.000000000000000000, 0.000000000000000000 ) ) ;
#17553 = VERTEX_POINT ( 'NONE', #1712 ) ;
#17554 = EDGE_CURVE ( 'NONE', #4033, #15369, #3244, .T. ) ;
#17555 = CARTESIAN_POINT ( 'NONE',  ( 33.81874022276149816, 19.50000000000000000, 1.818740222761735970 ) ) ;
#17556 = EDGE_LOOP ( 'NONE', ( #26226, #27808, #25447, #8574 ) ) ;
#17557 = CARTESIAN_POINT ( 'NONE',  ( -5.362942409646513475, -3.366872799099910998E-15, -3.000000000000000000 ) ) ;
#17559 = ORIENTED_EDGE ( 'NONE', *, *, #17594, .F. ) ;
#17558 = CARTESIAN_POINT ( 'NONE',  ( 40.87782285394631998, -5.765244507547243380, -4.018749766559461811 ) ) ;
#17560 = ORIENTED_EDGE ( 'NONE', *, *, #8759, .T. ) ;
#17561 = CARTESIAN_POINT ( 'NONE',  ( 0.7632845268451443621, 5.538577986791731078, -6.772677083973650092 ) ) ;
#17562 = CARTESIAN_POINT ( 'NONE',  ( 7.077711312404847644E-17, 0.8254815157535873027, -4.681538312723508177 ) ) ;
#17563 = CARTESIAN_POINT ( 'NONE',  ( 19.10390797508229710, -2.015740111943975066, 0.07017451552782173751 ) ) ;
#17565 = ORIENTED_EDGE ( 'NONE', *, *, #14313, .T. ) ;
#17564 = CARTESIAN_POINT ( 'NONE',  ( 22.49290772595112387, 0.1310194482076003919, 2.499999999999998668 ) ) ;
#17566 = CARTESIAN_POINT ( 'NONE',  ( 107.5617723795404999, -18.98359893170737323, 4.522129901861158707 ) ) ;
#17567 = CARTESIAN_POINT ( 'NONE',  ( 41.56220206661831895, -20.97620094563766457, 4.522129901861156931 ) ) ;
#17568 = FACE_OUTER_BOUND ( 'NONE', #7821, .T. ) ;
#17569 = CARTESIAN_POINT ( 'NONE',  ( 8.842484022065033145, 0.1108283380285731701, -1.500000000000000000 ) ) ;
#17572 = EDGE_CURVE ( 'NONE', #9922, #9843, #9169, .T. ) ;
#17571 = ORIENTED_EDGE ( 'NONE', *, *, #6240, .T. ) ;
#17570 = CARTESIAN_POINT ( 'NONE',  ( 108.0291956795919219, -18.48977263977070606, -4.324979624428802794 ) ) ;
#17573 = CARTESIAN_POINT ( 'NONE',  ( 0.000000000000000000, 0.000000000000000000, 0.000000000000000000 ) ) ;
#17574 = CARTESIAN_POINT ( 'NONE',  ( 23.50111451137534857, -3.256483526998273983E-15, 2.499999999999998668 ) ) ;
#17575 = EDGE_CURVE ( 'NONE', #31514, #21400, #31633, .T. ) ;
#17576 = FACE_OUTER_BOUND ( 'NONE', #31509, .T. ) ;
#17577 = CARTESIAN_POINT ( 'NONE',  ( 18.74987994845499628, -5.973062925086321862, -3.842005681288779950 ) ) ;
#17578 = DIRECTION ( 'NONE',  ( 0.5649695393302013313, 0.8251117619019986416, 2.783162557147745187E-15 ) ) ;
#17579 = ORIENTED_EDGE ( 'NONE', *, *, #3772, .T. ) ;
#17580 = DIRECTION ( 'NONE',  ( 1.000000000000000000, -0.000000000000000000, -0.000000000000000000 ) ) ;
#17581 = CIRCLE ( 'NONE', #24515, 5.000000000000000000 ) ;
#17582 = DIRECTION ( 'NONE',  ( 0.000000000000000000, 0.000000000000000000, -1.000000000000000000 ) ) ;
#17583 = CARTESIAN_POINT ( 'NONE',  ( -7.787550801365593856, -0.3701630799359326152, 3.521866450007987037 ) ) ;
#17584 = VERTEX_POINT ( 'NONE', #4204 ) ;
#17585 = ADVANCED_FACE ( 'NONE', ( #24584 ), #20105, .F. ) ;
#17586 = VECTOR ( 'NONE', #21931, 1000.000000000000000 ) ;
#17587 = CARTESIAN_POINT ( 'NONE',  ( -5.450050802731187360, -1.887961173149512062, -2.331437884370912261 ) ) ;
#17588 = CARTESIAN_POINT ( 'NONE',  ( -31.59999999999999787, 0.000000000000000000, 1.500000000000000000 ) ) ;
#17589 = APPLICATION_CONTEXT ( 'configuration controlled 3d designs of mechanical parts and assemblies' ) ;
#17590 = DIRECTION ( 'NONE',  ( 0.000000000000000000, 0.7431448254773954654, -0.6691306063588569053 ) ) ;
#17591 = EDGE_LOOP ( 'NONE', ( #27674, #9477, #10962, #29386, #13131 ) ) ;
#17592 = DIRECTION ( 'NONE',  ( 0.000000000000000000, 0.000000000000000000, -1.000000000000000000 ) ) ;
#17593 = ORIENTED_EDGE ( 'NONE', *, *, #13422, .F. ) ;
#17594 = EDGE_CURVE ( 'NONE', #19511, #9922, #22114, .T. ) ;
#17595 = CARTESIAN_POINT ( 'NONE',  ( 107.3477315916820913, -15.88627780335592021, 1.500000000000000000 ) ) ;
#17596 = ORIENTED_EDGE ( 'NONE', *, *, #6133, .T. ) ;
#17597 = FACE_OUTER_BOUND ( 'NONE', #26015, .T. ) ;
#17599 = ORIENTED_EDGE ( 'NONE', *, *, #31164, .T. ) ;
#17598 = CARTESIAN_POINT ( 'NONE',  ( 23.22564588060096469, -22.38932300456763969, -1.000000000000000000 ) ) ;
#17600 = ORIENTED_EDGE ( 'NONE', *, *, #31294, .F. ) ;
#17601 = CYLINDRICAL_SURFACE ( 'NONE', #17161, 4.000000000000001776 ) ;
#17603 = ORIENTED_EDGE ( 'NONE', *, *, #1389, .T. ) ;
#17602 = CIRCLE ( 'NONE', #4243, 11.00000000000000000 ) ;
#17604 = CARTESIAN_POINT ( 'NONE',  ( 7.249760686538667009, 7.199384779417119518, 4.973063321323901498 ) ) ;
#17606 = ORIENTED_EDGE ( 'NONE', *, *, #7097, .F. ) ;
#17605 = CARTESIAN_POINT ( 'NONE',  ( 6.013832568680315127, -13.53405802968792848, -1.500000000000000000 ) ) ;
#17607 = CIRCLE ( 'NONE', #24536, 8.025310301077736241 ) ;
#17608 = CARTESIAN_POINT ( 'NONE',  ( 0.1334381338377635395, -6.141084277567379957, -1.772361585196223999 ) ) ;
#17609 = DIRECTION ( 'NONE',  ( 0.000000000000000000, 0.000000000000000000, -1.000000000000000000 ) ) ;
#17610 = CARTESIAN_POINT ( 'NONE',  ( 1.750000000000000222, 1.106368468154540263, -8.427689411260562480 ) ) ;
#17611 = EDGE_CURVE ( 'NONE', #10072, #6731, #19212, .T. ) ;
#17612 = CIRCLE ( 'NONE', #8006, 4.499999999999997335 ) ;
#17613 = EDGE_CURVE ( 'NONE', #31435, #6261, #19895, .T. ) ;
#17614 = PLANE ( 'NONE',  #26234 ) ;
#17615 = DIRECTION ( 'NONE',  ( -1.000000000000000000, 8.574039729943018344E-17, -0.000000000000000000 ) ) ;
#17616 = CARTESIAN_POINT ( 'NONE',  ( 25.49907528997210093, -17.55969604403590978, 1.109946655922742664 ) ) ;
#17617 = FACE_OUTER_BOUND ( 'NONE', #8990, .T. ) ;
#17618 = CARTESIAN_POINT ( 'NONE',  ( 68.79832465278998654, -7.861404707920828905, 0.02339150517593243869 ) ) ;
#17619 = DIRECTION ( 'NONE',  ( 0.000000000000000000, 1.000000000000000000, 0.000000000000000000 ) ) ;
#17620 = CARTESIAN_POINT ( 'NONE',  ( 29.27523314209665628, -3.695744416148424971, 0.07017451550799837234 ) ) ;
#17621 = VECTOR ( 'NONE', #13016, 1000.000000000000000 ) ;
#17622 = DIRECTION ( 'NONE',  ( 1.000000000000000000, -0.000000000000000000, 8.654346879536960414E-15 ) ) ;
#17623 = CARTESIAN_POINT ( 'NONE',  ( -1.950050802731187138, 2.983565686104819648, 0.3135853898029609677 ) ) ;
#17624 = ORIENTED_EDGE ( 'NONE', *, *, #11968, .T. ) ;
#17625 = CARTESIAN_POINT ( 'NONE',  ( -8.137550801365593500, 1.828967928396027176, -3.368539882008727115 ) ) ;
#17626 = CIRCLE ( 'NONE', #7483, 4.000000000000001776 ) ;
#17627 = DIRECTION ( 'NONE',  ( 1.000000000000000000, -0.000000000000000000, -0.000000000000000000 ) ) ;
#17628 = CARTESIAN_POINT ( 'NONE',  ( -50.60000000000000142, -10.96966150227468972, 1.500000000000000000 ) ) ;
#17629 = ORIENTED_EDGE ( 'NONE', *, *, #13071, .T. ) ;
#17630 = CARTESIAN_POINT ( 'NONE',  ( -1.900050802731187760, 2.853674364686379583, 1.549418761218565921 ) ) ;
#17631 = CARTESIAN_POINT ( 'NONE',  ( 108.0225568495473567, -18.39417513866207088, 4.506423374900446532 ) ) ;
#17632 = CIRCLE ( 'NONE', #24571, 5.010000000000000675 ) ;
#17633 = ORIENTED_EDGE ( 'NONE', *, *, #17931, .F. ) ;
#17634 = CARTESIAN_POINT ( 'NONE',  ( 8.397160224431742037, -14.43505762332009823, 1.755102938775167098 ) ) ;
#17635 = COORDINATED_UNIVERSAL_TIME_OFFSET ( 0, 0, .AHEAD. ) ;
#17637 = VERTEX_POINT ( 'NONE', #28317 ) ;
#17636 = CARTESIAN_POINT ( 'NONE',  ( -3.616018626656801960, -10.49347358198851943, -1.499999999999999556 ) ) ;
#17638 = ORIENTED_EDGE ( 'NONE', *, *, #22660, .T. ) ;
#17639 = CARTESIAN_POINT ( 'NONE',  ( 11.84005032159772419, -19.96225593911332297, 1.750548462235233416 ) ) ;
#17640 = VERTEX_POINT ( 'NONE', #13260 ) ;
#17641 = CARTESIAN_POINT ( 'NONE',  ( 24.81047430030741552, 18.92139209076561457, -1.500000000000001776 ) ) ;
#17643 = ORIENTED_EDGE ( 'NONE', *, *, #28090, .F. ) ;
#17642 = CARTESIAN_POINT ( 'NONE',  ( 3.499999999999999556, 6.226349476952025341, 0.5315761383463585288 ) ) ;
#17644 = DIRECTION ( 'NONE',  ( 1.000000000000000000, 0.000000000000000000, 0.000000000000000000 ) ) ;
#17645 = DIRECTION ( 'NONE',  ( -6.062761635205572056E-17, -0.7071067811865460184, -0.7071067811865490160 ) ) ;
#17646 = AXIS2_PLACEMENT_3D ( 'NONE', #24737, #19903, #9505 ) ;
#17647 = AXIS2_PLACEMENT_3D ( 'NONE', #32972, #15053, #4871 ) ;
#17648 = ADVANCED_FACE ( 'NONE', ( #31343 ), #26658, .F. ) ;
#17649 = CARTESIAN_POINT ( 'NONE',  ( 21.60651947346046953, -21.76079427965450819, -1.483814047169784711 ) ) ;
#17650 = CARTESIAN_POINT ( 'NONE',  ( 101.7777785755449855, -3.698550425766125471, 4.282234000388568163 ) ) ;
#17651 = EDGE_CURVE ( 'NONE', #6731, #11524, #22779, .T. ) ;
#17652 = CIRCLE ( 'NONE', #31530, 5.009999999999999787 ) ;
#17653 = VERTEX_POINT ( 'NONE', #11250 ) ;
#17654 = FACE_OUTER_BOUND ( 'NONE', #4915, .T. ) ;
#17655 = DIRECTION ( 'NONE',  ( 7.770718973608983587E-17, 0.9063077870366511579, -0.4226182617406968878 ) ) ;
#17656 = DIRECTION ( 'NONE',  ( 0.000000000000000000, 1.000000000000000000, -0.000000000000000000 ) ) ;
#17657 = DIRECTION ( 'NONE',  ( 1.776356839400250465E-15, 0.000000000000000000, 1.000000000000000000 ) ) ;
#17658 = AXIS2_PLACEMENT_3D ( 'NONE', #27446, #7363, #25263 ) ;
#17659 = CARTESIAN_POINT ( 'NONE',  ( 3.063284526839887167, -6.772677083992345359, -5.538577986808975062 ) ) ;
#17660 = DIRECTION ( 'NONE',  ( -1.000000000000000000, 0.000000000000000000, 0.000000000000000000 ) ) ;
#17661 = CARTESIAN_POINT ( 'NONE',  ( -56.28351068141993352, -3.534499082302744455E-14, -1.000000000037517767 ) ) ;
#17662 = CARTESIAN_POINT ( 'NONE',  ( 22.70718278262391010, -21.88016059487456033, 1.342589741762119315 ) ) ;
#17663 = B_SPLINE_CURVE_WITH_KNOTS ( 'NONE', 3,
 ( #3190, #21391, #28603, #858, #26730, #8687, #24045, #11525 ),
 .UNSPECIFIED., .F., .F.,
 ( 4, 2, 2, 4 ),
 ( 2.024520226829450289E-07, 0.001227962984610849210, 0.001841843250904934542, 0.002455723517199020090 ),
 .UNSPECIFIED. ) ;
#17664 = VERTEX_POINT ( 'NONE', #23800 ) ;
#17665 = CARTESIAN_POINT ( 'NONE',  ( -5.812550801365592434, -3.368539882008727115, -1.828967928396028064 ) ) ;
#17666 = ORIENTED_EDGE ( 'NONE', *, *, #11199, .F. ) ;
#17667 = CARTESIAN_POINT ( 'NONE',  ( -7.854531657079157903, -2.846291840500172921, -1.545410377633947618 ) ) ;
#17668 = CARTESIAN_POINT ( 'NONE',  ( 22.23500000136559862, -3.156283516753370044, -0.9349337715887220401 ) ) ;
#17669 = VECTOR ( 'NONE', #15624, 1000.000000000000000 ) ;
#17670 = CARTESIAN_POINT ( 'NONE',  ( 108.0329321482101648, 18.36153912052067128, 4.597321217600237375 ) ) ;
#17671 = CIRCLE ( 'NONE', #22999, 15.00000000000000355 ) ;
#17672 = CARTESIAN_POINT ( 'NONE',  ( 2.629595859988236750, -11.38843847601185288, 1.760289366381509346 ) ) ;
#17673 = DIRECTION ( 'NONE',  ( 0.000000000000000000, 1.000000000000000000, 0.000000000000000000 ) ) ;
#17674 = ORIENTED_EDGE ( 'NONE', *, *, #28600, .T. ) ;
#17675 = LINE ( 'NONE', #2495, #20427 ) ;
#17676 = AXIS2_PLACEMENT_3D ( 'NONE', #21548, #29223, #23542 ) ;
#17677 = AXIS2_PLACEMENT_3D ( 'NONE', #22033, #11501, #6466 ) ;
#17678 = VECTOR ( 'NONE', #15848, 1000.000000000000000 ) ;
#17679 = CARTESIAN_POINT ( 'NONE',  ( -7.000050800000000351, 0.000000000000000000, 0.000000000000000000 ) ) ;
#17680 = ORIENTED_EDGE ( 'NONE', *, *, #20442, .T. ) ;
#17681 = CARTESIAN_POINT ( 'NONE',  ( 7.249760686538667009, -5.064320921489867899, 7.135485519861982873 ) ) ;
#17682 = APPLICATION_PROTOCOL_DEFINITION ( 'international standard', 'config_control_design', 1994, #18239 ) ;
#17683 = CARTESIAN_POINT ( 'NONE',  ( 69.06963061213430422, -6.099968625253806565, 4.018750763354483446 ) ) ;
#17684 = AXIS2_PLACEMENT_3D ( 'NONE', #20823, #110, #10299 ) ;
#17685 = ADVANCED_FACE ( 'NONE', ( #21457 ), #8573, .T. ) ;
#17686 = DIRECTION ( 'NONE',  ( 1.000000000000000000, -0.000000000000000000, 0.000000000000000000 ) ) ;
#17688 = FACE_OUTER_BOUND ( 'NONE', #20880, .T. ) ;
#17687 = CARTESIAN_POINT ( 'NONE',  ( 0.3076689308780821142, 8.857103639574720688, -5.232617538234502597 ) ) ;
#17689 = ORIENTED_EDGE ( 'NONE', *, *, #19595, .F. ) ;
#17690 = LINE ( 'NONE', #25040, #1251 ) ;
#17691 = CARTESIAN_POINT ( 'NONE',  ( 2.274274201621893976, 1.464956435144894931, 10.90201369671109610 ) ) ;
#17692 = CARTESIAN_POINT ( 'NONE',  ( 21.35999999999999943, -1.573300977624594976, 1.942864903642425700 ) ) ;
#17693 = DIRECTION ( 'NONE',  ( -0.000000000000000000, -0.000000000000000000, 1.000000000000000000 ) ) ;
#17695 = ORIENTED_EDGE ( 'NONE', *, *, #11617, .F. ) ;
#17694 = FACE_OUTER_BOUND ( 'NONE', #8440, .T. ) ;
#17696 = CARTESIAN_POINT ( 'NONE',  ( -7.462550801365593678, -3.521866450007987037, -0.3701630799359323931 ) ) ;
#17697 = DIRECTION ( 'NONE',  ( -1.000000000000000000, 0.000000000000000000, -0.000000000000000000 ) ) ;
#17698 = AXIS2_PLACEMENT_3D ( 'NONE', #24792, #16773, #30166 ) ;
#17699 = CARTESIAN_POINT ( 'NONE',  ( -53.94245116308378130, 5.494009027683203428, 1.203691125345451196 ) ) ;
#17700 = DIRECTION ( 'NONE',  ( -0.000000000000000000, -0.9961946980917461003, 0.08715574274765135188 ) ) ;
#17701 = ORIENTED_EDGE ( 'NONE', *, *, #7048, .F. ) ;
#17703 = ORIENTED_EDGE ( 'NONE', *, *, #29080, .F. ) ;
#17702 = CARTESIAN_POINT ( 'NONE',  ( 23.30969226767722091, -17.20274083179980451, 1.451821733976742301 ) ) ;
#17704 = AXIS2_PLACEMENT_3D ( 'NONE', #8310, #18650, #6273 ) ;
#17705 = CIRCLE ( 'NONE', #27848, 10.68156436372894724 ) ;
#17707 = VECTOR ( 'NONE', #6645, 1000.000000000000114 ) ;
#17706 = DIRECTION ( 'NONE',  ( 0.000000000000000000, 0.000000000000000000, -1.000000000000000000 ) ) ;
#17708 = CARTESIAN_POINT ( 'NONE',  ( 0.5704037183047365733, 5.066169706250169824, -8.085411865508655538 ) ) ;
#17709 =( BOUNDED_CURVE ( )  B_SPLINE_CURVE ( 3, ( #18878, #1331, #5995, #21367 ),
 .UNSPECIFIED., .F., .F. ) 
 B_SPLINE_CURVE_WITH_KNOTS ( ( 4, 4 ),
 ( 0.000000000000000000, 3.141592653589793116 ),
 .UNSPECIFIED. ) 
 CURVE ( )  GEOMETRIC_REPRESENTATION_ITEM ( )  RATIONAL_B_SPLINE_CURVE ( ( 1.000000000000000000, 0.3333333333333333703, 0.3333333333333333703, 1.000000000000000000 ) ) 
 REPRESENTATION_ITEM ( '' )  );
#17710 = EDGE_CURVE ( 'NONE', #6622, #19623, #16124, .T. ) ;
#17711 = VECTOR ( 'NONE', #31607, 1000.000000000000000 ) ;
#17712 = CARTESIAN_POINT ( 'NONE',  ( 21.54750000136559507, 1.913930629741522838, -2.363507492473150062 ) ) ;
#17713 = AXIS2_PLACEMENT_3D ( 'NONE', #14403, #14911, #4741 ) ;
#17714 = CARTESIAN_POINT ( 'NONE',  ( -30.00126220292998624, 9.321674377478409212, 2.002134007589322806 ) ) ;
#17715 = CARTESIAN_POINT ( 'NONE',  ( 8.236088440266469135, -19.08859993110833742, -1.499999999999919620 ) ) ;
#17716 = AXIS2_PLACEMENT_3D ( 'NONE', #15778, #16407, #31652 ) ;
#17717 = CARTESIAN_POINT ( 'NONE',  ( -23.54713438637982748, 10.71031731502107576, 2.573304945315896042 ) ) ;
#17718 = EDGE_CURVE ( 'NONE', #26820, #30798, #13991, .T. ) ;
#17719 = CARTESIAN_POINT ( 'NONE',  ( 19.01480233880637982, -3.011762293214985675, 0.4367666033482894283 ) ) ;
#17720 = LINE ( 'NONE', #2529, #15132 ) ;
#17721 = VERTEX_POINT ( 'NONE', #31009 ) ;
#17722 = DIRECTION ( 'NONE',  ( 1.000000000000000000, -8.574039729943018344E-17, -0.000000000000000000 ) ) ;
#17723 = AXIS2_PLACEMENT_3D ( 'NONE', #14363, #2033, #24413 ) ;
#17724 = ADVANCED_FACE ( 'NONE', ( #18301 ), #15935, .F. ) ;
#17725 = AXIS2_PLACEMENT_3D ( 'NONE', #19149, #29338, #21330 ) ;
#17726 = CARTESIAN_POINT ( 'NONE',  ( 3.063284526839889388, 2.223716399045570391, 8.461683424509315543 ) ) ;
#17727 = VECTOR ( 'NONE', #4809, 999.9999999999998863 ) ;
#17728 = EDGE_LOOP ( 'NONE', ( #28023, #239, #22605, #1738 ) ) ;
#17729 = VECTOR ( 'NONE', #26841, 1000.000000000000114 ) ;
#17730 = AXIS2_PLACEMENT_3D ( 'NONE', #25450, #17932, #10715 ) ;
#17731 = AXIS2_PLACEMENT_3D ( 'NONE', #32294, #19565, #17026 ) ;
#17732 = VERTEX_POINT ( 'NONE', #19614 ) ;
#17733 = CARTESIAN_POINT ( 'NONE',  ( -21.33422931780647502, 18.05240604713923958, 1.782833241104217592 ) ) ;
#17735 = ORIENTED_EDGE ( 'NONE', *, *, #23648, .T. ) ;
#17734 = CARTESIAN_POINT ( 'NONE',  ( 69.01532733225560889, -5.012350318234797264, -4.053848206251212005 ) ) ;
#17736 = ORIENTED_EDGE ( 'NONE', *, *, #14567, .T. ) ;
#17737 = EDGE_CURVE ( 'NONE', #6649, #20892, #24664, .T. ) ;
#17738 = CIRCLE ( 'NONE', #15082, 0.5000000000000000000 ) ;
#17739 = EDGE_CURVE ( 'NONE', #24462, #19352, #24793, .T. ) ;
#17740 = CARTESIAN_POINT ( 'NONE',  ( 14.13431920379513862, -20.70626837987542856, -1.500000000000000000 ) ) ;
#17741 = CARTESIAN_POINT ( 'NONE',  ( -6.762550801365593500, -2.752080473201636845, 2.228590825266444586 ) ) ;
#17742 = DIRECTION ( 'NONE',  ( 1.000000000000000000, 0.000000000000000000, 0.000000000000000000 ) ) ;
#17743 = CARTESIAN_POINT ( 'NONE',  ( 41.45135008765517881, -9.497951668093163491, -1.010822989962099960 ) ) ;
#17745 = ORIENTED_EDGE ( 'NONE', *, *, #14642, .T. ) ;
#17744 = DIRECTION ( 'NONE',  ( -8.281886410780513492E-17, -0.9659258262890682012, 0.2588190451025209060 ) ) ;
#17746 = DIRECTION ( 'NONE',  ( 0.000000000000000000, 0.000000000000000000, 1.000000000000000000 ) ) ;
#17747 = CARTESIAN_POINT ( 'NONE',  ( 102.6609843814833027, -1.982062027707615526, -4.522129901861162260 ) ) ;
#17748 = CARTESIAN_POINT ( 'NONE',  ( 0.5689136306499625872, -15.77252859670922724, 1.500000000000000444 ) ) ;
#17749 = CARTESIAN_POINT ( 'NONE',  ( 7.158832484464809021, -3.801775501247948164, -1.500000000000000000 ) ) ;
#17751 = VERTEX_POINT ( 'NONE', #9403 ) ;
#17750 = CARTESIAN_POINT ( 'NONE',  ( 3.499999999999999556, -7.851777359434021442, 3.255701506262407730 ) ) ;
#17752 = CARTESIAN_POINT ( 'NONE',  ( 1.750000000000000222, 0.6700234925292691823, 8.473551116235677583 ) ) ;
#17753 = AXIS2_PLACEMENT_3D ( 'NONE', #5056, #5368, #5207 ) ;
#17754 = VECTOR ( 'NONE', #22935, 1000.000000000000000 ) ;
#17755 = DIRECTION ( 'NONE',  ( 0.000000000000000000, 1.224646799147352961E-16, 1.000000000000000000 ) ) ;
#17756 = CARTESIAN_POINT ( 'NONE',  ( 25.42250000136559507, 1.913930629741522838, -2.363507492473150062 ) ) ;
#17757 = VECTOR ( 'NONE', #32834, 1000.000000000000000 ) ;
#17758 = VECTOR ( 'NONE', #21707, 1000.000000000000000 ) ;
#17759 = CARTESIAN_POINT ( 'NONE',  ( 3.249999999999999556, 4.057423117305393845, 8.475820894092990443 ) ) ;
#17760 = EDGE_CURVE ( 'NONE', #20952, #19944, #27121, .T. ) ;
#17761 = CARTESIAN_POINT ( 'NONE',  ( 5.489344046532323773, 6.978601450725543387, -4.149088721182456752 ) ) ;
#17762 = CARTESIAN_POINT ( 'NONE',  ( -23.35000000000000142, -10.96966150227469505, -1.500000000000000000 ) ) ;
#17763 = ORIENTED_EDGE ( 'NONE', *, *, #14330, .F. ) ;
#17764 = DIRECTION ( 'NONE',  ( -1.000000000000000000, -0.000000000000000000, -0.000000000000000000 ) ) ;
#17765 = TOROIDAL_SURFACE ( 'NONE', #26326, 301.4345239564033250, 4.000000000000000888 ) ;
#17766 = DIRECTION ( 'NONE',  ( -0.4999999999999981681, -0.8660254037844395958, 0.000000000000000000 ) ) ;
#17767 = CARTESIAN_POINT ( 'NONE',  ( -5.137550801365594388, -3.368539882008727115, -1.828967928396027842 ) ) ;
#17768 = VERTEX_POINT ( 'NONE', #4221 ) ;
#17769 = CARTESIAN_POINT ( 'NONE',  ( 25.32825331906372668, 2.585664297775035259, 0.3776202052181991675 ) ) ;
#17770 = FACE_OUTER_BOUND ( 'NONE', #24134, .T. ) ;
#17771 = CARTESIAN_POINT ( 'NONE',  ( -52.69999999999999574, -10.96966150227468972, 7.074999999999997513 ) ) ;
#17772 = VERTEX_POINT ( 'NONE', #29149 ) ;
#17773 = LINE ( 'NONE', #32997, #9691 ) ;
#17774 = ADVANCED_FACE ( 'NONE', ( #26974 ), #12087, .F. ) ;
#17775 = ORIENTED_EDGE ( 'NONE', *, *, #16828, .T. ) ;
#17776 = B_SPLINE_CURVE_WITH_KNOTS ( 'NONE', 3,
 ( #2317, #5476, #4799, #15323, #25880, #7653, #7818, #2483 ),
 .UNSPECIFIED., .F., .F.,
 ( 4, 2, 2, 4 ),
 ( 5.099451029770106864E-07, 0.001229189590448579025, 0.001843529413121382157, 0.002457869235794185071 ),
 .UNSPECIFIED. ) ;
#17777 = AXIS2_PLACEMENT_3D ( 'NONE', #18334, #28541, #8129 ) ;
#17778 = CARTESIAN_POINT ( 'NONE',  ( -41.57389320450581494, -15.56693736020740637, 5.315798355015693311 ) ) ;
#17779 = ORIENTED_EDGE ( 'NONE', *, *, #30846, .F. ) ;
#17780 = CARTESIAN_POINT ( 'NONE',  ( 107.5300661083891640, -18.52314831157204011, 5.060106418404170192 ) ) ;
#17781 = AXIS2_PLACEMENT_3D ( 'NONE', #25305, #11628, #21823 ) ;
#17783 = ORIENTED_EDGE ( 'NONE', *, *, #15371, .T. ) ;
#17782 = CARTESIAN_POINT ( 'NONE',  ( 3.249999999999999556, -1.239665997526952612, 9.314797388894886510 ) ) ;
#17784 = ORIENTED_EDGE ( 'NONE', *, *, #31452, .F. ) ;
#17785 = DIRECTION ( 'NONE',  ( -1.000000000000000000, 0.000000000000000000, 0.000000000000000000 ) ) ;
#17786 = EDGE_CURVE ( 'NONE', #5630, #19429, #24143, .T. ) ;
#17787 = CIRCLE ( 'NONE', #22589, 4.000000000000001776 ) ;
#17788 = EDGE_CURVE ( 'NONE', #5149, #27498, #32716, .T. ) ;
#17789 = AXIS2_PLACEMENT_3D ( 'NONE', #12128, #2280, #22679 ) ;
#17790 = AXIS2_PLACEMENT_3D ( 'NONE', #21258, #31456, #26456 ) ;
#17791 = ORIENTED_EDGE ( 'NONE', *, *, #22705, .T. ) ;
#17792 = CARTESIAN_POINT ( 'NONE',  ( 6.356382399260309235, -7.150437133400964207, 4.790388219480536947 ) ) ;
#17794 = ORIENTED_EDGE ( 'NONE', *, *, #6222, .T. ) ;
#17793 = CARTESIAN_POINT ( 'NONE',  ( 0.8174570305809125692, -9.170357625429589987, 1.500000000000000000 ) ) ;
#17795 = CARTESIAN_POINT ( 'NONE',  ( -5.357304906975410397, -1.062355717592097015, -2.999999999999998668 ) ) ;
#17796 = CARTESIAN_POINT ( 'NONE',  ( 0.000000000000000000, 0.000000000000000000, 0.000000000000000000 ) ) ;
#17797 = PRODUCT_DEFINITION_FORMATION_WITH_SPECIFIED_SOURCE ( 'ANY', '', #2027, .NOT_KNOWN. ) ;
#17798 = DIRECTION ( 'NONE',  ( -1.000000000000000000, 0.000000000000000000, 0.000000000000000000 ) ) ;
#17799 = CARTESIAN_POINT ( 'NONE',  ( 101.6200045064549329, -1.426643080118511708, 1.527295561047710803 ) ) ;
#17800 = CARTESIAN_POINT ( 'NONE',  ( 6.357667408475528248, 8.588075071450651521, 0.5738000813809884804 ) ) ;
#17801 = FACE_OUTER_BOUND ( 'NONE', #25550, .T. ) ;
#17802 = CARTESIAN_POINT ( 'NONE',  ( 0.6791199890552591656, 7.071625480714588186, -5.814932665552434266 ) ) ;
#17803 = EDGE_CURVE ( 'NONE', #29357, #6843, #10787, .T. ) ;
#17804 = CARTESIAN_POINT ( 'NONE',  ( 4.592425496802574958E-16, 37.67766952966368876, 3.750000000000000444 ) ) ;
#17805 = CARTESIAN_POINT ( 'NONE',  ( -0.7739934281325634435, -8.972773999336988382, 4.522129901861156931 ) ) ;
#17806 = PRODUCT_RELATED_PRODUCT_CATEGORY ( 'detail', '', ( #30333 ) ) ;
#17807 = CIRCLE ( 'NONE', #13009, 10.01806974338573752 ) ;
#17808 = CARTESIAN_POINT ( 'NONE',  ( 7.064423600674403225, 8.711672189282626988, 0.8180878109953719779 ) ) ;
#17809 = DIRECTION ( 'NONE',  ( -0.000000000000000000, -0.3746065934159164001, 0.9271838545667856479 ) ) ;
#17810 = CIRCLE ( 'NONE', #22084, 2.999999999999999556 ) ;
#17811 = AXIS2_PLACEMENT_3D ( 'NONE', #11256, #24444, #31680 ) ;
#17812 = CARTESIAN_POINT ( 'NONE',  ( 1.750000000000000222, 6.745408891279611296, -5.171987904998037067 ) ) ;
#17813 = CARTESIAN_POINT ( 'NONE',  ( -3.300050802731187893, -1.549418761218565477, 2.853674364686380471 ) ) ;
#17814 = EDGE_LOOP ( 'NONE', ( #12918, #1483, #26591, #3594, #21434, #12208 ) ) ;
#17815 = VECTOR ( 'NONE', #6359, 999.9999999999998863 ) ;
#17816 = VECTOR ( 'NONE', #24902, 1000.000000000000114 ) ;
#17817 = CARTESIAN_POINT ( 'NONE',  ( -7.137550801365592612, 3.368539882008727115, 1.828967928396026954 ) ) ;
#17818 = DIRECTION ( 'NONE',  ( -0.000000000000000000, 0.000000000000000000, 1.000000000000000000 ) ) ;
#17819 = DIRECTION ( 'NONE',  ( 0.000000000000000000, 0.000000000000000000, -1.000000000000000000 ) ) ;
#17820 = LOCAL_TIME ( 16, 7, 10.00000000000000000, #29589 ) ;
#17821 = VERTEX_POINT ( 'NONE', #1556 ) ;
#17822 = CARTESIAN_POINT ( 'NONE',  ( 18.75828436641558028, -5.879118399717574661, -3.993434336035625254 ) ) ;
#17823 = CARTESIAN_POINT ( 'NONE',  ( 5.612718825656738630, -5.432357446996367578, -6.163864706064005716 ) ) ;
#17824 = EDGE_CURVE ( 'NONE', #26609, #32336, #27290, .T. ) ;
#17825 = VERTEX_POINT ( 'NONE', #6737 ) ;
#17826 = CARTESIAN_POINT ( 'NONE',  ( 7.249760686538667009, 0.000000000000000000, 0.000000000000000000 ) ) ;
#17827 = SECURITY_CLASSIFICATION_LEVEL ( 'unclassified' ) ;
#17829 = ORIENTED_EDGE ( 'NONE', *, *, #9356, .F. ) ;
#17828 = CARTESIAN_POINT ( 'NONE',  ( -1.694237876702966217, -1.500727999663088896, -4.522129901861166701 ) ) ;
#17830 = ORIENTED_EDGE ( 'NONE', *, *, #24650, .T. ) ;
#17831 = CARTESIAN_POINT ( 'NONE',  ( -4.121075341857856067, -7.626600714980313889, 1.744488919440858377 ) ) ;
#17832 = VERTEX_POINT ( 'NONE', #24601 ) ;
#17833 = DIRECTION ( 'NONE',  ( 0.000000000000000000, 1.000000000000000000, 0.000000000000000000 ) ) ;
#17834 = VECTOR ( 'NONE', #34, 1000.000000000000000 ) ;
#17836 = ORIENTED_EDGE ( 'NONE', *, *, #11125, .T. ) ;
#17835 = DIRECTION ( 'NONE',  ( -1.000000000000000000, 8.574039729943022041E-17, -0.000000000000000000 ) ) ;
#17837 = AXIS2_PLACEMENT_3D ( 'NONE', #26179, #8128, #20685 ) ;
#17838 = CARTESIAN_POINT ( 'NONE',  ( 16.75741909111353678, 12.07361620705510497, 1.049999999999999600 ) ) ;
#17839 = CARTESIAN_POINT ( 'NONE',  ( 0.000000000000000000, 8.265874651078044977, -1.981241088980699061 ) ) ;
#17840 = AXIS2_PLACEMENT_3D ( 'NONE', #14251, #6895, #6743 ) ;
#17841 = CARTESIAN_POINT ( 'NONE',  ( 7.249760686538667009, 6.940565734314653845, -4.007137495034738706 ) ) ;
#17842 = DIRECTION ( 'NONE',  ( -1.000000000000000000, 0.000000000000000000, -0.000000000000000000 ) ) ;
#17843 = VERTEX_POINT ( 'NONE', #31832 ) ;
#17844 = CIRCLE ( 'NONE', #21564, 303.0536494382092769 ) ;
#17845 = CARTESIAN_POINT ( 'NONE',  ( 10.00000000000000178, 2.285372942704952060, 4.458382051008203284 ) ) ;
#17846 = CARTESIAN_POINT ( 'NONE',  ( 3.499999999999999556, 0.000000000000000000, 0.000000000000000000 ) ) ;
#17847 = DIRECTION ( 'NONE',  ( 0.000000000000000000, 0.5735764363510406083, 0.8191520442889956843 ) ) ;
#17848 = CARTESIAN_POINT ( 'NONE',  ( 0.000000000000000000, -4.762163868918202425, -9.915734732513268312 ) ) ;
#17849 = CC_DESIGN_SECURITY_CLASSIFICATION ( #26379, ( #3447 ) ) ;
#17850 = ADVANCED_FACE ( 'NONE', ( #14243 ), #31675, .T. ) ;
#17851 = LINE ( 'NONE', #10635, #14543 ) ;
#17852 = LINE ( 'NONE', #30747, #2229 ) ;
#17853 = CARTESIAN_POINT ( 'NONE',  ( -56.32142235783205564, 0.2514572592548188212, -1.435292253568081655 ) ) ;
#17854 = CARTESIAN_POINT ( 'NONE',  ( 22.92640216610012516, -21.90430348730595966, 1.195188340063319199 ) ) ;
#17855 = ORIENTED_EDGE ( 'NONE', *, *, #8073, .F. ) ;
#17856 = CARTESIAN_POINT ( 'NONE',  ( -5.612550801365594033, 1.828967928396027176, -3.368539882008727115 ) ) ;
#17857 = VERTEX_POINT ( 'NONE', #29300 ) ;
#17858 = CARTESIAN_POINT ( 'NONE',  ( -2.504531657079157370, -0.3127741368606806738, 2.975847129947406522 ) ) ;
#17859 = VECTOR ( 'NONE', #27006, 1000.000000000000114 ) ;
#17860 = CARTESIAN_POINT ( 'NONE',  ( 24.42250000136559507, -0.3178988483021076838, -3.024605502323848949 ) ) ;
#17861 = B_SPLINE_CURVE_WITH_KNOTS ( 'NONE', 3,
 ( #21507, #29810, #30312, #13782 ),
 .UNSPECIFIED., .F., .F.,
 ( 4, 4 ),
 ( 0.005731821976040855568, 0.005732069968806756399 ),
 .UNSPECIFIED. ) ;
#17862 = CARTESIAN_POINT ( 'NONE',  ( 107.9372080783385286, 17.82850972856275362, 4.742639206112238881 ) ) ;
#17863 = CARTESIAN_POINT ( 'NONE',  ( 18.41703969107078365, -16.82189904609263564, 1.753330412709693586 ) ) ;
#17864 = CARTESIAN_POINT ( 'NONE',  ( 3.249999999999999556, 8.734705317681626724, 0.4999240074894746311 ) ) ;
#17865 = ORIENTED_EDGE ( 'NONE', *, *, #9343, .T. ) ;
#17866 = EDGE_CURVE ( 'NONE', #15147, #25174, #29162, .T. ) ;
#17867 = FACE_OUTER_BOUND ( 'NONE', #21795, .T. ) ;
#17868 = EDGE_CURVE ( 'NONE', #32072, #15472, #20011, .T. ) ;
#17869 = VERTEX_POINT ( 'NONE', #6577 ) ;
#17870 = CARTESIAN_POINT ( 'NONE',  ( -53.56955650739543273, 4.402097243136370963, 5.500000000000000000 ) ) ;
#17871 = EDGE_CURVE ( 'NONE', #13047, #9758, #37, .T. ) ;
#17872 = PERSON_AND_ORGANIZATION ( #6766, #25292 ) ;
#17874 = CARTESIAN_POINT ( 'NONE',  ( 69.06834080223671890, -6.074152155849746215, 4.053848206249033304 ) ) ;
#17873 = CC_DESIGN_APPROVAL ( #8983, ( #21588 ) ) ;
#17875 = CARTESIAN_POINT ( 'NONE',  ( 19.01480233880980464, -3.011762293215291653, -0.4426577274541297347 ) ) ;
#17877 = DIRECTION ( 'NONE',  ( 0.000000000000000000, 0.000000000000000000, 1.000000000000000000 ) ) ;
#17876 = CARTESIAN_POINT ( 'NONE',  ( 0.1574692253523934382, -10.40622129948746633, -2.132217800985146017 ) ) ;
#17878 = B_SPLINE_CURVE_WITH_KNOTS ( 'NONE', 3,
 ( #3886, #29273, #9026, #19247, #11404, #6545, #29126, #6212, #26948, #16395 ),
 .UNSPECIFIED., .F., .F.,
 ( 4, 2, 2, 2, 4 ),
 ( 1.968338519004493493E-07, 0.0005467926395225675444, 0.001093388445193234099, 0.001639984250863900546, 0.002186580056534566992 ),
 .UNSPECIFIED. ) ;
#17879 = ORIENTED_EDGE ( 'NONE', *, *, #1183, .F. ) ;
#17880 = CARTESIAN_POINT ( 'NONE',  ( -8.000050800000000351, -1.091513931690352157, -2.808169894813009382 ) ) ;
#17881 = FACE_OUTER_BOUND ( 'NONE', #10465, .T. ) ;
#17882 = CARTESIAN_POINT ( 'NONE',  ( 23.42250000136559862, -0.3178988483021076838, -3.024605502323848949 ) ) ;
#17883 = DIRECTION ( 'NONE',  ( 4.917867153432994099E-17, 0.5735764363510447161, 0.8191520442889927978 ) ) ;
#17885 = ORIENTED_EDGE ( 'NONE', *, *, #21318, .F. ) ;
#17884 = CARTESIAN_POINT ( 'NONE',  ( 7.249760686538667009, 8.711672189281440382, -0.8180878109960949551 ) ) ;
#17886 = AXIS2_PLACEMENT_3D ( 'NONE', #24437, #1554, #16925 ) ;
#17887 = CARTESIAN_POINT ( 'NONE',  ( -6.912550801365593856, 1.088641768524161613, 3.675193018007247403 ) ) ;
#17888 = CARTESIAN_POINT ( 'NONE',  ( 5.377543748152549874, 5.151476664237558900, -6.139290821770204687 ) ) ;
#17889 = FACE_OUTER_BOUND ( 'NONE', #8430, .T. ) ;
#17890 = PLANE ( 'NONE',  #3289 ) ;
#17891 = VERTEX_POINT ( 'NONE', #20121 ) ;
#17893 = EDGE_LOOP ( 'NONE', ( #26205, #23559, #17703, #13028 ) ) ;
#17892 = CARTESIAN_POINT ( 'NONE',  ( 0.7632845268458192667, 3.174628368984171889, -8.152713396062660323 ) ) ;
#17894 = FACE_OUTER_BOUND ( 'NONE', #7886, .T. ) ;
#17895 = DIRECTION ( 'NONE',  ( 1.000000000000000000, -8.574039729943018344E-17, -0.000000000000000000 ) ) ;
#17896 = CARTESIAN_POINT ( 'NONE',  ( 21.23500000136559507, -3.156283516753370488, -0.9349337715887220401 ) ) ;
#17897 = CARTESIAN_POINT ( 'NONE',  ( -26.78358164153306120, 5.033963319885375043, 1.499999999999090949 ) ) ;
#17898 = CARTESIAN_POINT ( 'NONE',  ( 0.3749742847181612437, -9.289351359934261865, 3.955024136976932780 ) ) ;
#17900 = EDGE_CURVE ( 'NONE', #7488, #24872, #17429, .T. ) ;
#17899 = B_SPLINE_CURVE_WITH_KNOTS ( 'NONE', 3,
 ( #31102, #31760, #21370, #18693, #3518, #23877, #8834, #31271, #23546, #18541, #11166, #5824 ),
 .UNSPECIFIED., .F., .F.,
 ( 4, 2, 2, 2, 2, 4 ),
 ( 0.004476667581006692556, 0.005062001261575544211, 0.005354668101859973509, 0.005501001522002187290, 0.005574168232073290277, 0.005647334942144392397 ),
 .UNSPECIFIED. ) ;
#17901 = LINE ( 'NONE', #25746, #6573 ) ;
#17902 = CARTESIAN_POINT ( 'NONE',  ( 29.34042402276601891, -3.698761498129244263, 0.07017451552756237554 ) ) ;
#17903 = CARTESIAN_POINT ( 'NONE',  ( 41.44907012423725234, -8.741883605793594469, 2.713652344655544724 ) ) ;
#17904 = ORIENTED_EDGE ( 'NONE', *, *, #29612, .T. ) ;
#17905 = DIRECTION ( 'NONE',  ( 1.000000000000000000, 0.000000000000000000, 0.000000000000000000 ) ) ;
#17906 = EDGE_CURVE ( 'NONE', #9926, #22465, #23599, .T. ) ;
#17907 = COORDINATED_UNIVERSAL_TIME_OFFSET ( 0, 0, .AHEAD. ) ;
#17908 = CARTESIAN_POINT ( 'NONE',  ( 101.9180023365599936, -5.717737701100571890, -0.8134928171553283960 ) ) ;
#17909 = VERTEX_POINT ( 'NONE', #17936 ) ;
#17910 = LINE ( 'NONE', #15544, #1787 ) ;
#17911 = ORIENTED_EDGE ( 'NONE', *, *, #3437, .F. ) ;
#17912 = CARTESIAN_POINT ( 'NONE',  ( -19.05749829221029401, 5.903777093689171807, 2.093710349196163278 ) ) ;
#17914 = ORIENTED_EDGE ( 'NONE', *, *, #8283, .F. ) ;
#17913 = CARTESIAN_POINT ( 'NONE',  ( 102.3463693925194917, -2.889373554450824333, -4.043900685077098878 ) ) ;
#17915 = ORIENTED_EDGE ( 'NONE', *, *, #21318, .T. ) ;
#17916 = CARTESIAN_POINT ( 'NONE',  ( -3.616018626656801960, -10.49347358198851943, -1.500000000000000000 ) ) ;
#17917 = CARTESIAN_POINT ( 'NONE',  ( -7.962550801365594566, 2.752080473201636845, -2.228590825266444142 ) ) ;
#17918 = CARTESIAN_POINT ( 'NONE',  ( 6.530491627857225367, -8.330327812606277860, 2.368289848745726456 ) ) ;
#17919 = CARTESIAN_POINT ( 'NONE',  ( 102.8769692529049564, -5.092190445904434704, 0.07017451552783667001 ) ) ;
#17921 = ORIENTED_EDGE ( 'NONE', *, *, #30286, .F. ) ;
#17920 = DIRECTION ( 'NONE',  ( 0.8660254037844409281, -0.4999999999999960587, 0.000000000000000000 ) ) ;
#17922 = CARTESIAN_POINT ( 'NONE',  ( 7.437041877750292684, 18.60036511249582958, 1.508259000770582059 ) ) ;
#17923 = CARTESIAN_POINT ( 'NONE',  ( 25.05611271041078680, 19.07770844178882186, 1.500000000000000000 ) ) ;
#17924 =( BOUNDED_SURFACE ( )  B_SPLINE_SURFACE ( 3, 2, ( 
 ( #398, #60, #25121 ),
 ( #10421, #13095, #33001 ),
 ( #20285, #20633, #5406 ),
 ( #20470, #10574, #30493 ),
 ( #25810, #7906, #7578 ),
 ( #8066, #20781, #18097 ),
 ( #2244, #18271, #17778 ),
 ( #15263, #15597, #28482 ) ),
 .UNSPECIFIED., .F., .F., .F. ) 
 B_SPLINE_SURFACE_WITH_KNOTS ( ( 4, 2, 2, 4 ),
 ( 3, 3 ),
 ( 0.000000000000000000, 0.001031706651898124964, 0.002063413303796249928, 0.004126826607592499856 ),
 ( 0.000000000000000000, 1.000000000000000000 ),
 .UNSPECIFIED. ) 
 GEOMETRIC_REPRESENTATION_ITEM ( )  RATIONAL_B_SPLINE_SURFACE ( (
 ( 1.000000000000000000, 0.7660444431189785686, 1.000000000000000000),
 ( 1.000000000000000000, 0.8085210103973671236, 1.000000000000000000),
 ( 1.000000000000000000, 0.8435318601841085284, 1.000000000000000000),
 ( 1.000000000000000000, 0.9022997401202091927, 1.000000000000000000),
 ( 1.000000000000000000, 0.9260936007027841255, 1.000000000000000000),
 ( 1.000000000000000000, 0.9823303353967430818, 1.000000000000000000),
 ( 1.000000000000000000, 0.9997933690884138747, 1.000000000000000000),
 ( 1.000000000000000000, 1.000000000000000000, 1.000000000000000000) ) ) 
 REPRESENTATION_ITEM ( '' )  SURFACE ( )  );
#17925 = CARTESIAN_POINT ( 'NONE',  ( -1.597432620025311945, -13.32264212359284805, 1.744099735884073965 ) ) ;
#17926 = CARTESIAN_POINT ( 'NONE',  ( 21.17250000136559507, -3.024605502323851169, 0.3178988483021052969 ) ) ;
#17927 = CARTESIAN_POINT ( 'NONE',  ( 12.44989959798868817, 0.000000000000000000, 13.00000000000004441 ) ) ;
#17929 = VERTEX_POINT ( 'NONE', #25454 ) ;
#17928 = CARTESIAN_POINT ( 'NONE',  ( 108.0606309209090199, -18.94243229463347333, -4.540944552663033207 ) ) ;
#17930 = DIRECTION ( 'NONE',  ( 0.000000000000000000, 0.000000000000000000, 1.000000000000000000 ) ) ;
#17931 = EDGE_CURVE ( 'NONE', #17109, #2795, #13444, .T. ) ;
#17932 = DIRECTION ( 'NONE',  ( 0.000000000000000000, 0.000000000000000000, 1.000000000000000000 ) ) ;
#17933 = CARTESIAN_POINT ( 'NONE',  ( 21.92250000136559507, -1.913930629741527500, 2.363507492473149618 ) ) ;
#17934 = DIRECTION ( 'NONE',  ( 0.9993908270190957621, -0.03489949670250105940, 0.000000000000000000 ) ) ;
#17935 = CARTESIAN_POINT ( 'NONE',  ( 56.97280603064898941, -277.2763395528616002, 0.000000000000000000 ) ) ;
#17936 = CARTESIAN_POINT ( 'NONE',  ( -1.052005621165114313, 19.51744974835124680, 7.242429449796464525 ) ) ;
#17937 = ADVANCED_FACE ( 'NONE', ( #4730 ), #24948, .T. ) ;
#17938 = ORIENTED_EDGE ( 'NONE', *, *, #3257, .F. ) ;
#17939 = CARTESIAN_POINT ( 'NONE',  ( -38.14293509397970183, 21.49000000000000199, -1.500000000000000000 ) ) ;
#17940 = EDGE_CURVE ( 'NONE', #9325, #29938, #12961, .T. ) ;
#17941 = CARTESIAN_POINT ( 'NONE',  ( 10.00000000000000000, -3.055657119358777152, -3.641590349731960163 ) ) ;
#17942 = EDGE_CURVE ( 'NONE', #30719, #2302, #1236, .T. ) ;
#17943 = CARTESIAN_POINT ( 'NONE',  ( -4.987550801365594033, 0.3701630799359330593, -3.521866450007987037 ) ) ;
#17944 = ORIENTED_EDGE ( 'NONE', *, *, #30836, .T. ) ;
#17945 = CARTESIAN_POINT ( 'NONE',  ( 3.008012635915382038, -8.723904125990801006, 2.275870607900217113 ) ) ;
#17946 = LINE ( 'NONE', #10417, #23705 ) ;
#17947 = ADVANCED_FACE ( 'NONE', ( #27970 ), #26319, .F. ) ;
#17948 = CARTESIAN_POINT ( 'NONE',  ( 6.220890055307039646, -15.20372210278347680, -4.522129901861164925 ) ) ;
#17949 = CARTESIAN_POINT ( 'NONE',  ( 85.49734435724840864, -7.913007294147472059, 0.07017451552781736601 ) ) ;
#17950 = ORIENTED_EDGE ( 'NONE', *, *, #26518, .F. ) ;
#17951 = CARTESIAN_POINT ( 'NONE',  ( 101.9216173105994443, -5.769792427975438009, 0.07017451552781736601 ) ) ;
#17952 = ORIENTED_EDGE ( 'NONE', *, *, #14376, .T. ) ;
#17953 = CARTESIAN_POINT ( 'NONE',  ( -2.799189356623903890, 0.2797963115142978463, 0.9035254090724027520 ) ) ;
#17955 = VERTEX_POINT ( 'NONE', #9908 ) ;
#17954 = CARTESIAN_POINT ( 'NONE',  ( -3.222375984151269357, 0.000000000000000000, 1.000000000000000000 ) ) ;
#17956 = ORIENTED_EDGE ( 'NONE', *, *, #8866, .F. ) ;
#17957 = CARTESIAN_POINT ( 'NONE',  ( 7.249760686538667009, -4.973063321323826003, -7.199384779417172808 ) ) ;
#17958 = EDGE_CURVE ( 'NONE', #26824, #24117, #27381, .T. ) ;
#17959 = VERTEX_POINT ( 'NONE', #2722 ) ;
#17960 = CARTESIAN_POINT ( 'NONE',  ( 2.671540748214986660, 0.5000000000000006661, -1.500000000000000000 ) ) ;
#17962 = VERTEX_POINT ( 'NONE', #32494 ) ;
#17961 = DIRECTION ( 'NONE',  ( -1.000000000000000000, 0.000000000000000000, 0.000000000000000000 ) ) ;
#17963 = CARTESIAN_POINT ( 'NONE',  ( -5.600050800000000883, -2.331437884370912705, 1.887961173149512062 ) ) ;
#17964 = CARTESIAN_POINT ( 'NONE',  ( 3.249999999999999556, 0.000000000000000000, 8.749000000000002331 ) ) ;
#17965 = CARTESIAN_POINT ( 'NONE',  ( 16.87487612390083669, -15.54663979847903477, -1.500000000000000000 ) ) ;
#17966 = LINE ( 'NONE', #12933, #18157 ) ;
#17967 = DIRECTION ( 'NONE',  ( 0.000000000000000000, 0.000000000000000000, -1.000000000000000000 ) ) ;
#17968 = CARTESIAN_POINT ( 'NONE',  ( 5.887529311434773760, 8.386653846779019261, 0.3723788567093603841 ) ) ;
#17969 = CARTESIAN_POINT ( 'NONE',  ( 3.249999999999999556, 8.572527594031471218E-16, 6.999999999999998224 ) ) ;
#17970 = CARTESIAN_POINT ( 'NONE',  ( 85.10546509784848013, -6.328795743774838556, 2.184955973835313703 ) ) ;
#17971 = DIRECTION ( 'NONE',  ( 0.000000000000000000, -0.9659258262890650926, -0.2588190451025325634 ) ) ;
#17972 = CARTESIAN_POINT ( 'NONE',  ( 0.1517578099452172036, -1.375880305419571625, 4.522129901861156931 ) ) ;
#17973 = DIRECTION ( 'NONE',  ( 7.770718973608992215E-17, 0.9063077870366524902, -0.4226182617406938347 ) ) ;
#17974 = DIRECTION ( 'NONE',  ( 1.000000000000000000, 0.000000000000000000, 0.000000000000000000 ) ) ;
#17975 = B_SPLINE_CURVE_WITH_KNOTS ( 'NONE', 3,
 ( #14360, #32462, #1693, #24260, #24761, #4193, #6536, #29778 ),
 .UNSPECIFIED., .F., .F.,
 ( 4, 2, 2, 4 ),
 ( 0.000000000000000000, 0.5000000000000000000, 0.7500000000000000000, 1.000000000000000000 ),
 .UNSPECIFIED. ) ;
#17976 = EDGE_CURVE ( 'NONE', #25934, #18680, #6405, .T. ) ;
#17977 = CARTESIAN_POINT ( 'NONE',  ( 5.489343806296449024, -8.012901424861405886, -1.307372367723720563 ) ) ;
#17978 = EDGE_CURVE ( 'NONE', #10298, #2361, #8175, .T. ) ;
#17979 = CARTESIAN_POINT ( 'NONE',  ( -2.350050802731187272, -2.983565686104819648, -0.3135853898029605791 ) ) ;
#17980 = VERTEX_POINT ( 'NONE', #14750 ) ;
#17981 = CARTESIAN_POINT ( 'NONE',  ( -6.987550801365594033, -0.3701630799359326152, 3.521866450007987037 ) ) ;
#17982 = CARTESIAN_POINT ( 'NONE',  ( 8.870145747188287189, 0.000000000000000000, -1.000000000000000000 ) ) ;
#17983 = FACE_OUTER_BOUND ( 'NONE', #15911, .T. ) ;
#17984 = ORIENTED_EDGE ( 'NONE', *, *, #4868, .F. ) ;
#17985 = LINE ( 'NONE', #18133, #14386 ) ;
#17986 =( NAMED_UNIT ( * ) PLANE_ANGLE_UNIT ( ) SI_UNIT ( $, .RADIAN. ) );
#17987 = ADVANCED_FACE ( 'NONE', ( #4894 ), #25295, .T. ) ;
#17988 = ORIENTED_EDGE ( 'NONE', *, *, #183, .T. ) ;
#17989 = CARTESIAN_POINT ( 'NONE',  ( 29.41391112839824373, -2.700987858898175276, -1.010822989962086416 ) ) ;
#17990 = APPROVAL_DATE_TIME ( #12290, #7567 ) ;
#17992 = ORIENTED_EDGE ( 'NONE', *, *, #6089, .T. ) ;
#17991 = CARTESIAN_POINT ( 'NONE',  ( 101.9216173105994159, -5.769792427975438898, 0.07017451552781732438 ) ) ;
#17993 = ORIENTED_EDGE ( 'NONE', *, *, #4705, .T. ) ;
#17994 = CARTESIAN_POINT ( 'NONE',  ( 26.44001828968094259, 18.17676778675653537, -2.806473568333505586 ) ) ;
#17995 = ADVANCED_FACE ( 'NONE', ( #12729 ), #5965, .F. ) ;
#17996 = EDGE_LOOP ( 'NONE', ( #14705, #14885, #24307, #11274 ) ) ;
#17997 = APPROVAL ( #7624, 'UNSPECIFIED' ) ;
#17998 = DIRECTION ( 'NONE',  ( -0.1356223135424326209, 0.9907606108790346644, 0.000000000000000000 ) ) ;
#18000 = ORIENTED_EDGE ( 'NONE', *, *, #14146, .T. ) ;
#17999 = DIRECTION ( 'NONE',  ( 3.469446951953478110E-15, 0.000000000000000000, -1.000000000000000000 ) ) ;
#18001 = CARTESIAN_POINT ( 'NONE',  ( 102.9885081044300676, -6.698322160490905119, 1.010822989962089746 ) ) ;
#18002 = FACE_OUTER_BOUND ( 'NONE', #13154, .T. ) ;
#18003 = CARTESIAN_POINT ( 'NONE',  ( 22.00639167669224960, -21.80013755708282730, -1.499999999999999556 ) ) ;
#18004 = DIRECTION ( 'NONE',  ( 1.000000000000000000, 0.000000000000000000, 0.000000000000000000 ) ) ;
#18005 = ORIENTED_EDGE ( 'NONE', *, *, #29581, .F. ) ;
#18006 = FACE_OUTER_BOUND ( 'NONE', #8907, .T. ) ;
#18007 = CARTESIAN_POINT ( 'NONE',  ( -17.04380309137718186, -25.93932300454937945, 11.50000000000000000 ) ) ;
#18008 = CARTESIAN_POINT ( 'NONE',  ( 35.27266127981218347, -8.248087266145425644, -1.169950777424758170 ) ) ;
#18009 = CARTESIAN_POINT ( 'NONE',  ( -6.950050802731187360, 0.3135853898029611342, -2.983565686104819648 ) ) ;
#18010 = CARTESIAN_POINT ( 'NONE',  ( 24.42490082288193065, -17.42819879232223101, 1.446796129083761873 ) ) ;
#18011 = CARTESIAN_POINT ( 'NONE',  ( -7.356376981307137797, -0.1572233378491232070, 3.000000000000000444 ) ) ;
#18012 = CARTESIAN_POINT ( 'NONE',  ( -56.56779778351672405, 0.08779471422964917060, -1.028538298015328145 ) ) ;
#18013 = DIRECTION ( 'NONE',  ( -0.03487826274237457169, 0.9987827659587181772, -0.03487826274237498803 ) ) ;
#18014 = VERTEX_POINT ( 'NONE', #20932 ) ;
#18015 = EDGE_CURVE ( 'NONE', #28748, #6111, #16701, .T. ) ;
#18016 = CARTESIAN_POINT ( 'NONE',  ( -5.062550801365593323, -3.521866450007987037, -0.3701630799359323931 ) ) ;
#18017 = ORIENTED_EDGE ( 'NONE', *, *, #14376, .F. ) ;
#18018 = B_SPLINE_CURVE_WITH_KNOTS ( 'NONE', 3,
 ( #12221, #19601, #6873, #19946, #22425, #32640, #9720, #30154, #7229, #7378 ),
 .UNSPECIFIED., .F., .F.,
 ( 4, 2, 2, 2, 4 ),
 ( 2.571685856645629606E-07, 0.0005478592107668797933, 0.001095461252948095026, 0.001643063295129310259, 0.002190665337310525491 ),
 .UNSPECIFIED. ) ;
#18019 = CARTESIAN_POINT ( 'NONE',  ( -4.304531657079157192, 2.975847129947406522, 0.3127741368606808403 ) ) ;
#18020 = CARTESIAN_POINT ( 'NONE',  ( 108.0434313396344379, 18.42000276116402091, 5.147805806629488501 ) ) ;
#18021 = CARTESIAN_POINT ( 'NONE',  ( -38.14293509397969473, 10.97000000000000419, 1.050000000000000044 ) ) ;
#18022 = CARTESIAN_POINT ( 'NONE',  ( 7.362531900907073990, -8.542914936921636837, 1.000000000000000000 ) ) ;
#18023 = ORIENTED_EDGE ( 'NONE', *, *, #15895, .F. ) ;
#18024 = CARTESIAN_POINT ( 'NONE',  ( 21.62027785038666394, -21.76162169609135688, 1.485493366284274863 ) ) ;
#18025 = ORIENTED_EDGE ( 'NONE', *, *, #3484, .F. ) ;
#18026 = DIRECTION ( 'NONE',  ( 1.000000000000000000, -0.000000000000000000, -0.000000000000000000 ) ) ;
#18027 = DATE_AND_TIME ( #325, #27995 ) ;
#18028 = CARTESIAN_POINT ( 'NONE',  ( 85.03320566163840510, -5.162181109351803521, 4.053846905913455423 ) ) ;
#18029 = ADVANCED_FACE ( 'NONE', ( #8052 ), #13225, .T. ) ;
#18030 = CARTESIAN_POINT ( 'NONE',  ( -2.598264985223428969, 0.000000000000000000, 5.684322216989629695 ) ) ;
#18032 = CARTESIAN_POINT ( 'NONE',  ( 6.357667873252802693, 8.266402141659474623, -2.398098878660871680 ) ) ;
#18031 = CYLINDRICAL_SURFACE ( 'NONE', #12418, 6.248999999999999666 ) ;
#18033 = VERTEX_POINT ( 'NONE', #879 ) ;
#18034 = CARTESIAN_POINT ( 'NONE',  ( -8.000050800000002127, -2.542211635524239455, 1.618308171042345034 ) ) ;
#18035 = CARTESIAN_POINT ( 'NONE',  ( 3.249999999999999556, -9.314797388894900720, 1.239665997526854468 ) ) ;
#18036 = CARTESIAN_POINT ( 'NONE',  ( 20.98500000136559862, -0.9349337715887248157, 3.156283516753367824 ) ) ;
#18037 = LINE ( 'NONE', #23231, #119 ) ;
#18039 = ORIENTED_EDGE ( 'NONE', *, *, #16494, .T. ) ;
#18038 = CARTESIAN_POINT ( 'NONE',  ( 108.1156589233279135, 18.82219444680288234, -4.397958565568440115 ) ) ;
#18040 = CARTESIAN_POINT ( 'NONE',  ( -5.112550801365594033, -3.675193018007246071, 1.088641768524163167 ) ) ;
#18041 = CARTESIAN_POINT ( 'NONE',  ( 107.8490366731511898, 17.33753655370295377, -2.517018891476558995 ) ) ;
#18042 = DIRECTION ( 'NONE',  ( -1.000000000000000000, -0.000000000000000000, 0.000000000000000000 ) ) ;
#18043 = CARTESIAN_POINT ( 'NONE',  ( 22.23500000000000298, 0.2613211581691317065, 2.486304738420681559 ) ) ;
#18044 = VERTEX_POINT ( 'NONE', #31455 ) ;
#18045 = VERTEX_POINT ( 'NONE', #3215 ) ;
#18046 = EDGE_CURVE ( 'NONE', #18687, #22141, #23283, .T. ) ;
#18047 = DIRECTION ( 'NONE',  ( 0.000000000000000000, -0.08715574274766617335, 0.9961946980917448791 ) ) ;
#18048 = DIRECTION ( 'NONE',  ( -1.000000000000000000, 0.000000000000000000, -0.000000000000000000 ) ) ;
#18049 = ADVANCED_FACE ( 'NONE', ( #28277 ), #13475, .T. ) ;
#18050 = CARTESIAN_POINT ( 'NONE',  ( 21.98500000136559507, -0.9349337715887247047, 3.156283516753367824 ) ) ;
#18051 = CARTESIAN_POINT ( 'NONE',  ( 2.589202987961084279, 2.218054364314597127, 10.07394153291403782 ) ) ;
#18052 = DIRECTION ( 'NONE',  ( -0.8660254037844399289, 0.4999999999999978351, 0.000000000000000000 ) ) ;
#18053 = PRODUCT_DEFINITION_SHAPE ( 'NONE', 'NONE',  #33104 ) ;
#18054 = CARTESIAN_POINT ( 'NONE',  ( 41.34386496145283729, -3.886814715717017865, 0.4367667078936094960 ) ) ;
#18055 = CARTESIAN_POINT ( 'NONE',  ( 69.14445055419174935, -7.589252662750706868, 1.529340293463288480 ) ) ;
#18056 = EDGE_LOOP ( 'NONE', ( #19465, #2427, #26123, #19982 ) ) ;
#18057 = CARTESIAN_POINT ( 'NONE',  ( -23.54713438638086842, 3.998227953278294944, 2.146185852361370383 ) ) ;
#18058 = CARTESIAN_POINT ( 'NONE',  ( 18.93617721851659041, -3.890633339435721982, 4.522129901861162260 ) ) ;
#18059 = EDGE_LOOP ( 'NONE', ( #26775, #6399, #26492, #31923 ) ) ;
#18060 = CARTESIAN_POINT ( 'NONE',  ( 108.0793717420579014, 18.62013310325329840, -5.132089558057739254 ) ) ;
#18061 = ORIENTED_EDGE ( 'NONE', *, *, #32263, .T. ) ;
#18062 = CARTESIAN_POINT ( 'NONE',  ( -18.45273447307403814, 6.578304958228390120, 2.075379730733474926 ) ) ;
#18064 = ORIENTED_EDGE ( 'NONE', *, *, #4938, .T. ) ;
#18063 = CARTESIAN_POINT ( 'NONE',  ( 84.97936832876808921, -4.283865861974220479, -4.215289907538689818 ) ) ;
#18065 = ORIENTED_EDGE ( 'NONE', *, *, #10569, .F. ) ;
#18066 = CARTESIAN_POINT ( 'NONE',  ( -23.35000000000000142, -10.96966150227469505, 4.500000000000000888 ) ) ;
#18067 = CARTESIAN_POINT ( 'NONE',  ( -6.162550801365593856, 2.228590825266444142, 2.752080473201636845 ) ) ;
#18068 = CARTESIAN_POINT ( 'NONE',  ( -23.35000000000000142, -10.96966150227469505, 1.500000000000000000 ) ) ;
#18069 = CARTESIAN_POINT ( 'NONE',  ( 18.51491971917342028, -8.599446730134173933, -1.010822989962099960 ) ) ;
#18071 = ORIENTED_EDGE ( 'NONE', *, *, #5328, .T. ) ;
#18070 = FACE_OUTER_BOUND ( 'NONE', #22421, .T. ) ;
#18072 = CYLINDRICAL_SURFACE ( 'NONE', #7625, 4.000000000000001776 ) ;
#18073 = CARTESIAN_POINT ( 'NONE',  ( 24.28956136227655094, 18.19040579222011900, 1.500000000000650147 ) ) ;
#18074 = CARTESIAN_POINT ( 'NONE',  ( -2.351930117019871425, -12.55067978397925721, 1.499999999999719780 ) ) ;
#18075 = CARTESIAN_POINT ( 'NONE',  ( 24.98500000136559507, -2.892927487894331406, 1.570731468192932301 ) ) ;
#18076 = CARTESIAN_POINT ( 'NONE',  ( 25.75999999999999801, -2.208672634433321348E-15, 0.000000000000000000 ) ) ;
#18077 = EDGE_CURVE ( 'NONE', #17640, #15936, #26455, .T. ) ;
#18079 = ORIENTED_EDGE ( 'NONE', *, *, #23112, .F. ) ;
#18078 = CARTESIAN_POINT ( 'NONE',  ( 108.0612055743968369, -18.95070716190199889, -4.518753833174125489 ) ) ;
#18080 = FACE_OUTER_BOUND ( 'NONE', #3128, .T. ) ;
#18081 = EDGE_CURVE ( 'NONE', #23780, #17891, #21110, .T. ) ;
#18082 = CARTESIAN_POINT ( 'NONE',  ( -56.27770248097862549, 0.4996615022747108448, 0.000000000000000000 ) ) ;
#18083 = CARTESIAN_POINT ( 'NONE',  ( 21.73500000136559507, 1.570731468192929858, 2.892927487894329186 ) ) ;
#18084 = LINE ( 'NONE', #13223, #10811 ) ;
#18085 = CARTESIAN_POINT ( 'NONE',  ( 5.612718761614564400, 7.013540705848238410, -4.279483796478951163 ) ) ;
#18086 = CARTESIAN_POINT ( 'NONE',  ( -2.983877251335087077, -0.2474135948681053798, -1.436677650513773941 ) ) ;
#18087 = EDGE_LOOP ( 'NONE', ( #5632, #22741, #18632, #19484 ) ) ;
#18088 = CARTESIAN_POINT ( 'NONE',  ( 107.9932884231783277, -17.97271708001612822, 4.596977851539515214 ) ) ;
#18089 = DIRECTION ( 'NONE',  ( -1.000000000000000000, 0.000000000000000000, -0.000000000000000000 ) ) ;
#18090 = ORIENTED_EDGE ( 'NONE', *, *, #5808, .T. ) ;
#18091 = CARTESIAN_POINT ( 'NONE',  ( 0.000000000000000000, 9.915734732513218574, 4.762163868918305454 ) ) ;
#18092 = CARTESIAN_POINT ( 'NONE',  ( -16.96515769256209794, -25.93932300454937945, 11.09540449768827131 ) ) ;
#18093 = CARTESIAN_POINT ( 'NONE',  ( 0.9232102171129938917, 0.000000000000000000, -4.522129901861164925 ) ) ;
#18094 = CARTESIAN_POINT ( 'NONE',  ( 48.09670199522223299, -9.430894477028838097, -0.07017451552783579571 ) ) ;
#18095 = EDGE_CURVE ( 'NONE', #28727, #25625, #25196, .T. ) ;
#18096 = ORIENTED_EDGE ( 'NONE', *, *, #21455, .F. ) ;
#18097 = CARTESIAN_POINT ( 'NONE',  ( -41.33570690803944814, -14.97572508516781120, 5.493143919433947531 ) ) ;
#18098 = ORIENTED_EDGE ( 'NONE', *, *, #21003, .F. ) ;
#18099 =( BOUNDED_CURVE ( )  B_SPLINE_CURVE ( 2, ( #15934, #16584, #11249, #21625, #28660, #6091, #23636, #26627, #912, #18782, #21289 ),
 .UNSPECIFIED., .F., .F. ) 
 B_SPLINE_CURVE_WITH_KNOTS ( ( 3, 2, 2, 2, 2, 3 ),
 ( 0.8103822619934377691, 0.8125000000000000000, 0.8281250000000000000, 0.8437500000000000000, 0.8593750000000000000, 0.8728822619934377691 ),
 .UNSPECIFIED. ) 
 CURVE ( )  GEOMETRIC_REPRESENTATION_ITEM ( )  RATIONAL_B_SPLINE_CURVE ( ( 0.9821626249036861100, 0.9896829947469995004, 1.000000000000000000, 0.9238795325112867385, 1.000000000000000000, 0.9238795325112867385, 1.000000000000000000, 0.9238795325112867385, 1.000000000000000000, 0.9341965377642872381, 0.9821626249036861100 ) ) 
 REPRESENTATION_ITEM ( '' )  );
#18100 = CARTESIAN_POINT ( 'NONE',  ( 0.000000000000000000, 10.90201369670498366, -1.464956435139577851 ) ) ;
#18102 = EDGE_LOOP ( 'NONE', ( #10868, #4964, #4588, #16794 ) ) ;
#18101 = CARTESIAN_POINT ( 'NONE',  ( -3.115650298287759856, -0.007755536299741299863, 1.107207510975252385 ) ) ;
#18103 = ORIENTED_EDGE ( 'NONE', *, *, #28557, .T. ) ;
#18104 = CARTESIAN_POINT ( 'NONE',  ( 0.000000000000000000, 0.000000000000000000, 0.000000000000000000 ) ) ;
#18105 = ORIENTED_EDGE ( 'NONE', *, *, #12254, .T. ) ;
#18106 = DIRECTION ( 'NONE',  ( -1.000000000000000000, -0.000000000000000000, -0.000000000000000000 ) ) ;
#18107 = EDGE_CURVE ( 'NONE', #17857, #7402, #10409, .T. ) ;
#18109 = ORIENTED_EDGE ( 'NONE', *, *, #6126, .T. ) ;
#18108 = CARTESIAN_POINT ( 'NONE',  ( -34.48223484310472031, 0.000000000000000000, 2.552009564962238741 ) ) ;
#18110 = ORIENTED_EDGE ( 'NONE', *, *, #20616, .T. ) ;
#18111 = DIRECTION ( 'NONE',  ( 0.000000000000000000, 1.000000000000000000, 0.000000000000000000 ) ) ;
#18112 = CARTESIAN_POINT ( 'NONE',  ( 21.67755997557487291, -21.76174915995097336, -1.411535641070696068 ) ) ;
#18113 = CARTESIAN_POINT ( 'NONE',  ( 108.1300413742128512, -20.08325238768279064, -1.420916680477450011 ) ) ;
#18114 = CARTESIAN_POINT ( 'NONE',  ( -1.075551320669168254, 0.4999999999999998890, 7.404527507138928932 ) ) ;
#18115 = CARTESIAN_POINT ( 'NONE',  ( 7.249760686538667009, 0.000000000000000000, 0.000000000000000000 ) ) ;
#18116 = CARTESIAN_POINT ( 'NONE',  ( 2.274274201625327230, 7.958834565716768061, 7.593217523260608282 ) ) ;
#18117 = EDGE_CURVE ( 'NONE', #22098, #21127, #2921, .T. ) ;
#18118 = DIRECTION ( 'NONE',  ( 0.000000000000000000, -0.4226182617406974984, -0.9063077870366508249 ) ) ;
#18119 = DIRECTION ( 'NONE',  ( 7.023442172597882746E-17, 0.8191520442889946851, -0.5735764363510419406 ) ) ;
#18120 = B_SPLINE_CURVE_WITH_KNOTS ( 'NONE', 3,
 ( #30896, #7969, #31054, #8139, #18349, #7459, #15170, #12651, #33056, #29038 ),
 .UNSPECIFIED., .F., .F.,
 ( 4, 2, 2, 2, 4 ),
 ( 0.000000000000000000, 0.001704392904692032329, 0.002556589357038042964, 0.002982687583211043620, 0.003408785809384044276 ),
 .UNSPECIFIED. ) ;
#18121 = DIRECTION ( 'NONE',  ( 1.000000000000000000, 0.000000000000000000, 0.000000000000000000 ) ) ;
#18122 = CARTESIAN_POINT ( 'NONE',  ( 3.499999999999999556, 0.000000000000000000, 0.000000000000000000 ) ) ;
#18123 = CARTESIAN_POINT ( 'NONE',  ( 6.038145268433179780, -5.783741681378121946, 6.194606843114065953 ) ) ;
#18124 = ADVANCED_FACE ( 'NONE', ( #7893 ), #5388, .T. ) ;
#18125 = CARTESIAN_POINT ( 'NONE',  ( 23.72239361536733782, -6.441344918542153408, 5.695980980372492120 ) ) ;
#18126 = DIRECTION ( 'NONE',  ( -0.000000000000000000, 0.4226182617406975539, -0.9063077870366508249 ) ) ;
#18127 = ORIENTED_EDGE ( 'NONE', *, *, #24976, .T. ) ;
#18128 = CARTESIAN_POINT ( 'NONE',  ( -5.637550801365595277, 3.675193018007247403, -1.088641768524161391 ) ) ;
#18129 = CARTESIAN_POINT ( 'NONE',  ( 25.25210947164438124, -0.1742962440539902735, 2.517109471644361385 ) ) ;
#18130 = ADVANCED_FACE ( 'NONE', ( #32118 ), #17037, .T. ) ;
#18131 = LINE ( 'NONE', #13269, #27432 ) ;
#18132 = ORIENTED_EDGE ( 'NONE', *, *, #392, .F. ) ;
#18133 = CARTESIAN_POINT ( 'NONE',  ( 1.624999999999999778, -7.593217523260524793, -7.958834565716851550 ) ) ;
#18134 = AXIS2_PLACEMENT_3D ( 'NONE', #9795, #27836, #19828 ) ;
#18135 = ORIENTED_EDGE ( 'NONE', *, *, #1091, .T. ) ;
#18136 = CARTESIAN_POINT ( 'NONE',  ( 102.5305753040692736, -0.1042037546421150512, -0.07017451552781585333 ) ) ;
#18137 = ADVANCED_FACE ( 'NONE', ( #6700 ), #1025, .F. ) ;
#18139 = ORIENTED_EDGE ( 'NONE', *, *, #19703, .T. ) ;
#18138 = CARTESIAN_POINT ( 'NONE',  ( 0.000000000000000000, -5.979767908488830663, -1.814490771706242622 ) ) ;
#18140 = ORIENTED_EDGE ( 'NONE', *, *, #2933, .F. ) ;
#18141 = LINE ( 'NONE', #10112, #10223 ) ;
#18142 = ORIENTED_EDGE ( 'NONE', *, *, #4277, .F. ) ;
#18143 = VECTOR ( 'NONE', #30343, 1000.000000000000000 ) ;
#18144 = DIRECTION ( 'NONE',  ( 7.023442172597854396E-17, 0.8191520442889912434, -0.5735764363510469366 ) ) ;
#18146 = ORIENTED_EDGE ( 'NONE', *, *, #18882, .F. ) ;
#18145 = DIRECTION ( 'NONE',  ( 3.623545766764271938E-17, 0.4226182617407062136, -0.9063077870366468280 ) ) ;
#18147 = CARTESIAN_POINT ( 'NONE',  ( 102.9885081044300676, -6.698322160490901567, 0.07017451552781803215 ) ) ;
#18148 = FACE_OUTER_BOUND ( 'NONE', #17442, .T. ) ;
#18149 = ADVANCED_FACE ( 'NONE', ( #21744 ), #15641, .T. ) ;
#18150 = CARTESIAN_POINT ( 'NONE',  ( -52.69999999999999574, -10.96966150227468972, 0.9999999999999991118 ) ) ;
#18151 = EDGE_CURVE ( 'NONE', #19632, #31676, #19928, .T. ) ;
#18152 = CARTESIAN_POINT ( 'NONE',  ( 0.000000000000000000, 9.241976615262133876, 1.699438267350532161 ) ) ;
#18153 = VERTEX_POINT ( 'NONE', #4039 ) ;
#18154 = CYLINDRICAL_SURFACE ( 'NONE', #8662, 6.248999999999999666 ) ;
#18155 = DIRECTION ( 'NONE',  ( 0.9896144216807899463, -0.000000000000000000, 0.1437473352845035635 ) ) ;
#18156 = CARTESIAN_POINT ( 'NONE',  ( 15.82680059085170221, 20.06867288585792863, -4.131740999229418954 ) ) ;
#18157 = VECTOR ( 'NONE', #32737, 1000.000000000000000 ) ;
#18158 = CARTESIAN_POINT ( 'NONE',  ( -8.000050800000000351, 0.8940492601045104681, 3.137005928241842323 ) ) ;
#18159 = DIRECTION ( 'NONE',  ( 1.000000000000000000, 0.000000000000000000, -0.000000000000000000 ) ) ;
#18160 = CARTESIAN_POINT ( 'NONE',  ( 0.3076690219754985023, -7.713510465969182661, -6.806638167515123961 ) ) ;
#18161 = CARTESIAN_POINT ( 'NONE',  ( 7.249760686538667009, 1.391664247347333294, -7.892520144992419162 ) ) ;
#18162 = VECTOR ( 'NONE', #10470, 1000.000000000000227 ) ;
#18163 = ORIENTED_EDGE ( 'NONE', *, *, #5095, .F. ) ;
#18164 = CARTESIAN_POINT ( 'NONE',  ( -7.612550801365593145, -1.828967928396026510, 3.368539882008728004 ) ) ;
#18165 = ORIENTED_EDGE ( 'NONE', *, *, #19153, .F. ) ;
#18166 = ADVANCED_FACE ( 'NONE', ( #1687 ), #16888, .F. ) ;
#18167 = CARTESIAN_POINT ( 'NONE',  ( -2.554531657079157192, 0.9198621039125853827, 3.105402419394639235 ) ) ;
#18168 = TOROIDAL_SURFACE ( 'NONE', #11246, 10.64228691119592796, 0.4500000000000000111 ) ;
#18169 = CARTESIAN_POINT ( 'NONE',  ( 107.9128139062042209, -20.39012166861472508, 1.488290602270393892 ) ) ;
#18170 = DIRECTION ( 'NONE',  ( 0.000000000000000000, 0.000000000000000000, 1.000000000000000000 ) ) ;
#18171 = CARTESIAN_POINT ( 'NONE',  ( 14.03158388662595435, -14.04624128054226340, 1.000000000000000000 ) ) ;
#18172 = ORIENTED_EDGE ( 'NONE', *, *, #21954, .F. ) ;
#18173 = EDGE_CURVE ( 'NONE', #23895, #8122, #18316, .T. ) ;
#18174 = ORIENTED_EDGE ( 'NONE', *, *, #29209, .T. ) ;
#18175 = CARTESIAN_POINT ( 'NONE',  ( 0.1606233060840182858, 9.683549581718741806, 4.384181225613559718 ) ) ;
#18176 = PERSON_AND_ORGANIZATION ( #6766, #25292 ) ;
#18177 = VECTOR ( 'NONE', #12138, 1000.000000000000000 ) ;
#18178 = CARTESIAN_POINT ( 'NONE',  ( 102.4167958684119668, -3.906015252786475322, 4.112224487556747299 ) ) ;
#18179 = ADVANCED_FACE ( 'NONE', ( #1371 ), #8495, .F. ) ;
#18180 = CIRCLE ( 'NONE', #8555, 10.99999999999999822 ) ;
#18181 = CARTESIAN_POINT ( 'NONE',  ( 9.302055952177829212, 0.2457637072967208403, 1.050000000000000044 ) ) ;
#18182 = VECTOR ( 'NONE', #8221, 1000.000000000000000 ) ;
#18184 = CARTESIAN_POINT ( 'NONE',  ( 3.499999999999999556, -4.724769925181202090, 4.089810527897741466 ) ) ;
#18183 = DIRECTION ( 'NONE',  ( 0.000000000000000000, 0.000000000000000000, 1.000000000000000000 ) ) ;
#18185 = VERTEX_POINT ( 'NONE', #26236 ) ;
#18186 = EDGE_CURVE ( 'NONE', #24130, #11832, #25987, .T. ) ;
#18187 = CARTESIAN_POINT ( 'NONE',  ( 2.274274201625327230, 0.000000000000000000, 0.000000000000000000 ) ) ;
#18188 = EDGE_CURVE ( 'NONE', #4178, #19641, #4824, .T. ) ;
#18189 = CARTESIAN_POINT ( 'NONE',  ( 10.00000000000000178, -8.574039729943018837E-16, 0.000000000000000000 ) ) ;
#18190 = CARTESIAN_POINT ( 'NONE',  ( 109.1472041058641196, 18.90877050785844204, 4.999054092451761022 ) ) ;
#18191 = CARTESIAN_POINT ( 'NONE',  ( 4.013969549054183686E-16, 4.681538312723517059, 0.8254815157535410064 ) ) ;
#18192 = CIRCLE ( 'NONE', #23533, 11.00000000000000000 ) ;
#18194 = ORIENTED_EDGE ( 'NONE', *, *, #1517, .T. ) ;
#18193 = CARTESIAN_POINT ( 'NONE',  ( 9.287819511157117347, 0.2249814976390548393, -1.045547970484144829 ) ) ;
#18195 = CARTESIAN_POINT ( 'NONE',  ( -7.262550801365593500, 0.3701630799359330593, -3.521866450007987037 ) ) ;
#18196 = DIRECTION ( 'NONE',  ( 8.574039729943018344E-17, 1.000000000000000000, 0.000000000000000000 ) ) ;
#18197 = CARTESIAN_POINT ( 'NONE',  ( 23.66826818115595188, -7.072331084912446109, -2.787782631235886210 ) ) ;
#18198 = ORIENTED_EDGE ( 'NONE', *, *, #23429, .F. ) ;
#18199 = EDGE_LOOP ( 'NONE', ( #25467, #8362, #13528, #9564 ) ) ;
#18200 = CARTESIAN_POINT ( 'NONE',  ( 7.249760686538667009, -2.789499415801756586E-14, 8.014274990069656823 ) ) ;
#18201 = DIRECTION ( 'NONE',  ( 0.000000000000000000, -0.2588190451025291772, 0.9659258262890660918 ) ) ;
#18202 = TOROIDAL_SURFACE ( 'NONE', #3793, 10.64228691119592796, 0.4500000000000000111 ) ;
#18203 = AXIS2_PLACEMENT_3D ( 'NONE', #14652, #14804, #17337 ) ;
#18204 = DIRECTION ( 'NONE',  ( 0.000000000000000000, 0.000000000000000000, 1.000000000000000000 ) ) ;
#18205 = CIRCLE ( 'NONE', #30041, 10.94895958125474245 ) ;
#18207 = EDGE_CURVE ( 'NONE', #20158, #20265, #28464, .T. ) ;
#18206 = CIRCLE ( 'NONE', #9655, 0.5000000000000004441 ) ;
#18208 = CARTESIAN_POINT ( 'NONE',  ( -2.962942409646513564, 4.884725290497410777E-15, -2.999999999999999556 ) ) ;
#18209 = CC_DESIGN_PERSON_AND_ORGANIZATION_ASSIGNMENT ( #26396, #21043, ( #7706 ) ) ;
#18210 = CARTESIAN_POINT ( 'NONE',  ( 101.6022419886208610, -1.170867242066747860, -0.07017451552781628354 ) ) ;
#18211 = TOROIDAL_SURFACE ( 'NONE', #9120, 3.895301350492843540, 15.00000000000000178 ) ;
#18212 = CARTESIAN_POINT ( 'NONE',  ( 4.749760686538667009, 4.007137495034909236, -6.940565734314555257 ) ) ;
#18213 = CARTESIAN_POINT ( 'NONE',  ( 18.60402535544292490, -7.603424548862589560, 0.4367666033480746557 ) ) ;
#18214 = ORIENTED_EDGE ( 'NONE', *, *, #19764, .F. ) ;
#18215 = DIRECTION ( 'NONE',  ( -0.000000000000000000, 0.000000000000000000, 1.000000000000000000 ) ) ;
#18216 = VECTOR ( 'NONE', #17448, 1000.000000000000114 ) ;
#18217 = COORDINATED_UNIVERSAL_TIME_OFFSET ( 0, 0, .AHEAD. ) ;
#18218 = CARTESIAN_POINT ( 'NONE',  ( 34.99330891680699551, 0.1916075530515802261, 2.493613503297696266 ) ) ;
#18219 = ORIENTED_EDGE ( 'NONE', *, *, #27506, .F. ) ;
#18220 = ADVANCED_FACE ( 'NONE', ( #13185 ), #10291, .T. ) ;
#18221 = DIRECTION ( 'NONE',  ( -1.000000000000000000, 0.000000000000000000, -0.000000000000000000 ) ) ;
#18222 = VERTEX_POINT ( 'NONE', #669 ) ;
#18223 = CARTESIAN_POINT ( 'NONE',  ( -19.56543409745250273, 5.443045001481024769, 2.106299155096469367 ) ) ;
#18225 = VERTEX_POINT ( 'NONE', #18208 ) ;
#18224 = CARTESIAN_POINT ( 'NONE',  ( 54.95446108375549699, -5.684089628123738080, -4.275175837990625283 ) ) ;
#18226 = VECTOR ( 'NONE', #24416, 1000.000000000000000 ) ;
#18227 = ORIENTED_EDGE ( 'NONE', *, *, #29823, .F. ) ;
#18228 = CARTESIAN_POINT ( 'NONE',  ( -1.996286585346913167, -0.3178988483021041866, 3.024605502323847173 ) ) ;
#18229 = DIRECTION ( 'NONE',  ( -8.281886410780538144E-17, -0.9659258262890716429, 0.2588190451025081940 ) ) ;
#18230 = AXIS2_PLACEMENT_3D ( 'NONE', #21067, #31267, #28888 ) ;
#18231 = LINE ( 'NONE', #20752, #29494 ) ;
#18232 = CIRCLE ( 'NONE', #4932, 15.00000000000000355 ) ;
#18233 = CARTESIAN_POINT ( 'NONE',  ( 29.18953645666586993, -9.308308156628571695, -1.010822989962099960 ) ) ;
#18235 = VERTEX_POINT ( 'NONE', #13042 ) ;
#18234 = CARTESIAN_POINT ( 'NONE',  ( 23.79966985373406985, 18.45386651007853729, -1.499999999999999778 ) ) ;
#18236 = CIRCLE ( 'NONE', #7014, 299.4192503346018270 ) ;
#18237 = CARTESIAN_POINT ( 'NONE',  ( 17.36028307725516839, -18.11957666780532250, 4.522129901861156931 ) ) ;
#18238 = CARTESIAN_POINT ( 'NONE',  ( 0.4355866597345551816, -15.33293614044432118, 1.500000000000319300 ) ) ;
#18240 = DIRECTION ( 'NONE',  ( 0.000000000000000000, 0.000000000000000000, 1.000000000000000000 ) ) ;
#18239 = APPLICATION_CONTEXT ( 'configuration controlled 3d designs of mechanical parts and assemblies' ) ;
#18241 = AXIS2_PLACEMENT_3D ( 'NONE', #4062, #8887, #24425 ) ;
#18242 = DIRECTION ( 'NONE',  ( 0.000000000000000000, 0.000000000000000000, 1.000000000000000000 ) ) ;
#18244 = ORIENTED_EDGE ( 'NONE', *, *, #24917, .T. ) ;
#18243 = CARTESIAN_POINT ( 'NONE',  ( -29.24402871571405882, -25.93932300454937945, 11.00000000000000000 ) ) ;
#18245 = CARTESIAN_POINT ( 'NONE',  ( 3.063284526839887167, 6.772677083992467928, -5.538577986808824960 ) ) ;
#18246 = CIRCLE ( 'NONE', #3837, 12.49867430706168570 ) ;
#18247 = AXIS2_PLACEMENT_3D ( 'NONE', #26867, #6453, #16172 ) ;
#18248 = CARTESIAN_POINT ( 'NONE',  ( 1.624999999999999778, 7.958834565716877307, -7.593217523260497259 ) ) ;
#18249 = CARTESIAN_POINT ( 'NONE',  ( 22.42250000136559507, 1.913930629741522838, -2.363507492473150062 ) ) ;
#18250 = CARTESIAN_POINT ( 'NONE',  ( -34.50075980479081039, -0.03048549489923630187, 2.568038078148746184 ) ) ;
#18251 = CARTESIAN_POINT ( 'NONE',  ( 6.880160201030087741, 8.703862158141008720, -0.6895871680713464569 ) ) ;
#18252 = CARTESIAN_POINT ( 'NONE',  ( 84.55169161418332635, -5.233307109668325907, 3.993432236216280629 ) ) ;
#18253 = VERTEX_POINT ( 'NONE', #30934 ) ;
#18254 = CARTESIAN_POINT ( 'NONE',  ( -56.32100375116784363, 0.5246615022747117552, -1.050000000000000044 ) ) ;
#18255 = AXIS2_PLACEMENT_3D ( 'NONE', #26753, #14712, #17229 ) ;
#18256 = DIRECTION ( 'NONE',  ( 1.000000000000000000, -3.469446951953588156E-15, 1.053584095796274567E-14 ) ) ;
#18257 = VERTEX_POINT ( 'NONE', #21070 ) ;
#18258 = VECTOR ( 'NONE', #14977, 1000.000000000000114 ) ;
#18259 = AXIS2_PLACEMENT_3D ( 'NONE', #31056, #805, #3141 ) ;
#18260 = CIRCLE ( 'NONE', #32170, 5.999999999999999112 ) ;
#18261 = CARTESIAN_POINT ( 'NONE',  ( 25.71953681024719174, 1.150786689167072163, 2.772749569664193725 ) ) ;
#18262 = FACE_OUTER_BOUND ( 'NONE', #29603, .T. ) ;
#18263 = CARTESIAN_POINT ( 'NONE',  ( 0.4082220075202826481, -6.684754012654101629, -0.9788672205888330202 ) ) ;
#18266 = CARTESIAN_POINT ( 'NONE',  ( 107.9935202411828215, -17.97605520161211956, 4.592059696647398326 ) ) ;
#18265 = FACE_OUTER_BOUND ( 'NONE', #18375, .T. ) ;
#18264 = VECTOR ( 'NONE', #5, 1000.000000000000000 ) ;
#18267 = EDGE_CURVE ( 'NONE', #19049, #26729, #5189, .T. ) ;
#18268 = ORIENTED_EDGE ( 'NONE', *, *, #24125, .F. ) ;
#18269 = EDGE_CURVE ( 'NONE', #29792, #13047, #23243, .T. ) ;
#18270 = CIRCLE ( 'NONE', #23068, 5.000000000000000000 ) ;
#18271 = CARTESIAN_POINT ( 'NONE',  ( -41.55992208616379457, -15.55928713972474675, 5.268872846871810900 ) ) ;
#18272 = ORIENTED_EDGE ( 'NONE', *, *, #15244, .T. ) ;
#18273 = CARTESIAN_POINT ( 'NONE',  ( 4.013969549054193054E-16, 4.681538312723529494, -0.8254815157534771686 ) ) ;
#18274 = EDGE_CURVE ( 'NONE', #18687, #24814, #22594, .T. ) ;
#18276 = EDGE_LOOP ( 'NONE', ( #27650, #8005, #18455, #4232 ) ) ;
#18275 = LINE ( 'NONE', #13242, #1074 ) ;
#18277 = ORIENTED_EDGE ( 'NONE', *, *, #10562, .F. ) ;
#18278 = PLANE ( 'NONE',  #23038 ) ;
#18279 = CARTESIAN_POINT ( 'NONE',  ( 6.524595551582241804, -7.168326838404976087, 4.857153507487923072 ) ) ;
#18281 = ORIENTED_EDGE ( 'NONE', *, *, #4425, .F. ) ;
#18280 = DIRECTION ( 'NONE',  ( -0.7821988420038089584, 0.6230288689682847991, 0.000000000000000000 ) ) ;
#18282 = AXIS2_PLACEMENT_3D ( 'NONE', #21170, #6262, #31368 ) ;
#18283 = ORIENTED_EDGE ( 'NONE', *, *, #27453, .F. ) ;
#18284 = CARTESIAN_POINT ( 'NONE',  ( -31.67864539881508179, -21.93932300455407258, 1.095404497688272194 ) ) ;
#18285 = AXIS2_PLACEMENT_3D ( 'NONE', #16930, #19967, #32658 ) ;
#18286 = CARTESIAN_POINT ( 'NONE',  ( 18.66631667619762780, -6.907132599765741787, 2.336383999542480439 ) ) ;
#18287 = CIRCLE ( 'NONE', #24660, 8.749000000000002331 ) ;
#18288 = CARTESIAN_POINT ( 'NONE',  ( 3.249999999999999556, 0.000000000000000000, 0.000000000000000000 ) ) ;
#18289 = DIRECTION ( 'NONE',  ( -1.000000000000000000, -0.000000000000000000, -0.000000000000000000 ) ) ;
#18290 = CARTESIAN_POINT ( 'NONE',  ( 107.9802527803230419, -17.78500706576073753, 4.325704939602341703 ) ) ;
#18291 = VECTOR ( 'NONE', #4559, 1000.000000000000000 ) ;
#18292 = AXIS2_PLACEMENT_3D ( 'NONE', #26488, #24294, #1408 ) ;
#18293 = VECTOR ( 'NONE', #32481, 1000.000000000000000 ) ;
#18294 = LINE ( 'NONE', #28503, #1151 ) ;
#18295 = CARTESIAN_POINT ( 'NONE',  ( 25.98690466878739613, 22.56136012750964426, 0.4463807625373348298 ) ) ;
#18296 = CARTESIAN_POINT ( 'NONE',  ( 55.00858942667073137, -7.632540988274553406, 2.184956776124872935 ) ) ;
#18297 = AXIS2_PLACEMENT_3D ( 'NONE', #1653, #21713, #16509 ) ;
#18298 = AXIS2_PLACEMENT_3D ( 'NONE', #4334, #6830, #17015 ) ;
#18299 = B_SPLINE_CURVE_WITH_KNOTS ( 'NONE', 3,
 ( #2534, #29944, #2189, #7031, #22598, #17245, #12375, #5355 ),
 .UNSPECIFIED., .F., .F.,
 ( 4, 2, 2, 4 ),
 ( 2.737843117464003789E-07, 0.001261207499628673586, 0.001891674357287136598, 0.002522141214945600694 ),
 .UNSPECIFIED. ) ;
#18300 = DIRECTION ( 'NONE',  ( 0.000000000000000000, -0.2588190451025325634, 0.9659258262890650926 ) ) ;
#18301 = FACE_OUTER_BOUND ( 'NONE', #19253, .T. ) ;
#18302 = ORIENTED_EDGE ( 'NONE', *, *, #23455, .T. ) ;
#18303 = CARTESIAN_POINT ( 'NONE',  ( 5.489321708267612898, -5.297846913781735445, 6.152096559282818511 ) ) ;
#18304 = CARTESIAN_POINT ( 'NONE',  ( 47.99837860531645362, -3.577301031424839017, 2.713652344655542503 ) ) ;
#18305 = FACE_OUTER_BOUND ( 'NONE', #5735, .T. ) ;
#18306 = EDGE_LOOP ( 'NONE', ( #10813, #7390, #8850, #16369 ) ) ;
#18307 = EDGE_CURVE ( 'NONE', #25473, #17955, #26848, .T. ) ;
#18308 = VECTOR ( 'NONE', #21842, 1000.000000000000000 ) ;
#18309 =( BOUNDED_SURFACE ( )  B_SPLINE_SURFACE ( 1, 3, ( 
 ( #31137, #17922, #3055, #13067 ),
 ( #23269, #10545, #5211, #25440 ) ),
 .UNSPECIFIED., .F., .F., .F. ) 
 B_SPLINE_SURFACE_WITH_KNOTS ( ( 2, 2 ),
 ( 4, 4 ),
 ( 0.000000000000000000, 1.000000000000000000 ),
 ( 0.000000000000000000, 1.000000000000000000 ),
 .UNSPECIFIED. ) 
 GEOMETRIC_REPRESENTATION_ITEM ( )  RATIONAL_B_SPLINE_SURFACE ( (
 ( 1.000000000000000000, 0.9321687722090974404, 0.9321687722090974404, 1.000000000000000000),
 ( 1.000000000000000000, 0.9321687722090974404, 0.9321687722090974404, 1.000000000000000000) ) ) 
 REPRESENTATION_ITEM ( '' )  SURFACE ( )  );
#18310 = VECTOR ( 'NONE', #8536, 1000.000000000000227 ) ;
#18311 = CARTESIAN_POINT ( 'NONE',  ( 25.33479043841976974, -2.021976348156035108, 1.643476287762689170 ) ) ;
#18312 = CARTESIAN_POINT ( 'NONE',  ( 17.37538333147393388, -21.16291065652740144, -1.500000000000095923 ) ) ;
#18314 = ORIENTED_EDGE ( 'NONE', *, *, #20557, .F. ) ;
#18313 = VECTOR ( 'NONE', #7165, 1000.000000000000000 ) ;
#18315 = CARTESIAN_POINT ( 'NONE',  ( -10.00000000000000000, 0.000000000000000000, 0.000000000000000000 ) ) ;
#18316 = CIRCLE ( 'NONE', #9761, 9.500000000000003553 ) ;
#18317 = CIRCLE ( 'NONE', #12439, 5.009999999999999787 ) ;
#18318 = VERTEX_POINT ( 'NONE', #10857 ) ;
#18319 = CARTESIAN_POINT ( 'NONE',  ( 41.43141396789279440, -2.886852813804333007, -1.010822989962086416 ) ) ;
#18320 = APPROVAL_STATUS ( 'not_yet_approved' ) ;
#18321 = CIRCLE ( 'NONE', #30080, 0.4500000000000017319 ) ;
#18323 = EDGE_LOOP ( 'NONE', ( #14593, #22383, #3009, #20589 ) ) ;
#18322 = CARTESIAN_POINT ( 'NONE',  ( 3.499999999999999556, 6.704570150427012543, -2.172265885002588437 ) ) ;
#18324 = EDGE_LOOP ( 'NONE', ( #10293, #15878, #27264, #26343 ) ) ;
#18325 = LINE ( 'NONE', #33039, #97 ) ;
#18326 = ORIENTED_EDGE ( 'NONE', *, *, #18882, .T. ) ;
#18327 = DIRECTION ( 'NONE',  ( -0.000000000000000000, -0.000000000000000000, -1.000000000000000000 ) ) ;
#18329 = ORIENTED_EDGE ( 'NONE', *, *, #26945, .F. ) ;
#18328 = DIRECTION ( 'NONE',  ( 0.000000000000000000, 0.2079116908177532363, 0.9781476007338069101 ) ) ;
#18330 = CARTESIAN_POINT ( 'NONE',  ( 0.000000000000000000, 7.533794289458167981, -7.944914065997031649 ) ) ;
#18332 = DIRECTION ( 'NONE',  ( 1.000000000000000000, 0.000000000000000000, 0.000000000000000000 ) ) ;
#18331 = PERSON ( 'NAUO-PER4', 'UNSPECIFIED', 'UNSPECIFIED', ('UNSPECIFIED'), ('UNSPECIFIED'), ('UNSPECIFIED') ) ;
#18333 = DIRECTION ( 'NONE',  ( 0.000000000000000000, 1.000000000000000000, 0.000000000000000000 ) ) ;
#18334 = CARTESIAN_POINT ( 'NONE',  ( 0.000000000000000000, -1.239665997526952612, 9.314797388894886510 ) ) ;
#18335 = ORIENTED_EDGE ( 'NONE', *, *, #19353, .T. ) ;
#18336 = AXIS2_PLACEMENT_3D ( 'NONE', #8084, #30702, #28155 ) ;
#18337 = B_SPLINE_CURVE_WITH_KNOTS ( 'NONE', 3,
 ( #4693, #22093, #32956, #27437, #14714, #9516, #9367, #7206, #30281, #32457 ),
 .UNSPECIFIED., .F., .F.,
 ( 4, 2, 2, 2, 4 ),
 ( 1.968338519011545307E-07, 0.0005467926395225681949, 0.001093388445193235184, 0.001639984250863902281, 0.002186580056534569161 ),
 .UNSPECIFIED. ) ;
#18338 = B_SPLINE_CURVE_WITH_KNOTS ( 'NONE', 3,
 ( #6751, #1571, #4238, #9258, #31849, #11949, #8918, #1421 ),
 .UNSPECIFIED., .F., .F.,
 ( 4, 2, 2, 4 ),
 ( 2.152606640980682932E-07, 0.001262065476475210347, 0.001892990584380766211, 0.002523915692286320123 ),
 .UNSPECIFIED. ) ;
#18339 = CIRCLE ( 'NONE', #12456, 303.6457063863959434 ) ;
#18340 = CARTESIAN_POINT ( 'NONE',  ( 8.930755659325139817, 0.4999999999999997780, 1.050000000000000044 ) ) ;
#18341 = DIRECTION ( 'NONE',  ( 1.000000000000000000, -8.574039729943018344E-17, -0.000000000000000000 ) ) ;
#18342 = CARTESIAN_POINT ( 'NONE',  ( 41.35597062191753537, -8.086568374296689399, -1.873789609314816307 ) ) ;
#18343 = DIRECTION ( 'NONE',  ( 0.7895257206258718963, 0.6137174728408810731, 0.000000000000000000 ) ) ;
#18344 = AXIS2_PLACEMENT_3D ( 'NONE', #6393, #18967, #21782 ) ;
#18345 = EDGE_CURVE ( 'NONE', #18014, #20999, #9203, .T. ) ;
#18346 = AXIS2_PLACEMENT_3D ( 'NONE', #12662, #33068, #1993 ) ;
#18347 = VECTOR ( 'NONE', #18201, 999.9999999999998863 ) ;
#18348 = CARTESIAN_POINT ( 'NONE',  ( -8.000050799999998574, -0.6196328501511008113, 3.096707085269658766 ) ) ;
#18349 = CARTESIAN_POINT ( 'NONE',  ( 23.29109779593791529, -17.41442569313431221, -1.664431119656285540 ) ) ;
#18350 = DIRECTION ( 'NONE',  ( 0.000000000000000000, 0.000000000000000000, 1.000000000000000000 ) ) ;
#18351 = CARTESIAN_POINT ( 'NONE',  ( 34.71233008869360503, 0.000000000000000000, -1.019564728980880908 ) ) ;
#18352 = EDGE_CURVE ( 'NONE', #20638, #2621, #28417, .T. ) ;
#18353 = CIRCLE ( 'NONE', #8205, 0.5000000000000000000 ) ;
#18354 = APPROVAL_PERSON_ORGANIZATION ( #17516, #10447, #12668 ) ;
#18355 = CARTESIAN_POINT ( 'NONE',  ( -2.962550801365593234, 2.228590825266444142, 2.752080473201636845 ) ) ;
#18356 = ORIENTED_EDGE ( 'NONE', *, *, #26158, .T. ) ;
#18357 = CARTESIAN_POINT ( 'NONE',  ( -3.954531657079157547, -3.105402419394638791, 0.9198621039125867149 ) ) ;
#18358 = FACE_OUTER_BOUND ( 'NONE', #12429, .T. ) ;
#18359 = EDGE_CURVE ( 'NONE', #19301, #15923, #5253, .T. ) ;
#18360 = DIRECTION ( 'NONE',  ( 0.000000000000000000, 0.000000000000000000, 1.000000000000000000 ) ) ;
#18361 = CARTESIAN_POINT ( 'NONE',  ( 13.44509804349992166, -13.81913516303365341, 1.000000000000000000 ) ) ;
#18362 = ORIENTED_EDGE ( 'NONE', *, *, #3980, .F. ) ;
#18363 = DIRECTION ( 'NONE',  ( 0.000000000000000000, 1.000000000000000000, 0.000000000000000000 ) ) ;
#18364 = EDGE_CURVE ( 'NONE', #9701, #32393, #190, .T. ) ;
#18365 = VECTOR ( 'NONE', #30162, 999.9999999999998863 ) ;
#18366 = ORIENTED_EDGE ( 'NONE', *, *, #24487, .F. ) ;
#18367 = DIRECTION ( 'NONE',  ( -0.04710975479914573244, -0.5265925107009691297, -0.8488115212910426477 ) ) ;
#18368 = DATE_TIME_ROLE ( 'classification_date' ) ;
#18369 = CARTESIAN_POINT ( 'NONE',  ( 69.06389083184971867, -5.985077526012525517, 4.150066331403145625 ) ) ;
#18370 = EDGE_CURVE ( 'NONE', #16869, #26634, #30786, .T. ) ;
#18371 = DIRECTION ( 'NONE',  ( -0.6916610887771532656, 0.000000000000000000, -0.7222222222222208776 ) ) ;
#18373 = DIRECTION ( 'NONE',  ( -1.000000000000000000, 0.000000000000000000, 0.000000000000000000 ) ) ;
#18372 = CARTESIAN_POINT ( 'NONE',  ( -0.9232102171129843438, 0.000000000000000000, 4.522129901861158707 ) ) ;
#18374 = AXIS2_PLACEMENT_3D ( 'NONE', #10875, #8022, #8508 ) ;
#18375 = EDGE_LOOP ( 'NONE', ( #6756, #5402, #9422, #8903 ) ) ;
#18376 = CC_DESIGN_APPROVAL ( #28639, ( #3447 ) ) ;
#18377 = CARTESIAN_POINT ( 'NONE',  ( 18.85511084203137955, -4.796792731031784385, 4.091315477141355572 ) ) ;
#18378 = CARTESIAN_POINT ( 'NONE',  ( -23.35000000000000142, -10.96966150227469505, 4.500000000000000888 ) ) ;
#18379 = CARTESIAN_POINT ( 'NONE',  ( 9.337065666035901046, -0.007760238742138971836, 1.098363920870218946 ) ) ;
#18380 = EDGE_CURVE ( 'NONE', #25632, #292, #9602, .T. ) ;
#18382 = ORIENTED_EDGE ( 'NONE', *, *, #14627, .F. ) ;
#18381 = CARTESIAN_POINT ( 'NONE',  ( 24.38302348701447997, -17.39153354040979949, -1.380603655064296387 ) ) ;
#18383 = CARTESIAN_POINT ( 'NONE',  ( -5.462550801365593678, 3.521866450007987037, 0.3701630799359328372 ) ) ;
#18384 = CARTESIAN_POINT ( 'NONE',  ( 108.2286009897290597, 19.45110043733557958, 3.071383935681160970 ) ) ;
#18385 = CARTESIAN_POINT ( 'NONE',  ( -3.135269660805079628, -0.4999999999999985012, 1.949999999999999956 ) ) ;
#18386 = ORIENTED_EDGE ( 'NONE', *, *, #25491, .F. ) ;
#18387 = VERTEX_POINT ( 'NONE', #31916 ) ;
#18388 =( BOUNDED_SURFACE ( )  B_SPLINE_SURFACE ( 1, 2, ( 
 ( #14823, #30391, #22533, #28054, #2136, #7464, #10487, #30572, #20541, #18164, #28204, #5152, #28369, #20357, #20047, #2322, #15173, #30242, #4991, #4805, #2821, #25022, #27875, #23210, #25379, #315, #30751, #10328, #25698, #25198, #20699, #12804, #15484, #22712, #12505, #12316, #7658, #2487, #12655, #23017, #22859, #32914, #33061, #9984, #20195, #17665, #10134, #139, #7314, #17856, #15327, #25532, #30901, #32755, #2639, #9831, #17504, #27699, #14981, #7822, #18016, #13000, #8622, #31724, #10985, #23690, #619, #29045, #10812, #459, #18509, #28855, #31057, #21187, #18840, #3000, #6134, #31385, #5650, #8460, #8144, #5796, #16317, #8313, #3482, #31238, #23508, #21030, #23353, #26195, #28703, #5954, #5484, #18654, #25886, #26527, #8799, #13153, #10640, #20847, #15973, #26382, #18355, #3626, #21331, #16152, #26039, #23842, #23987, #953, #1109, #15677, #3304, #13639, #13473, #807, #13785, #11132, #11304, #21512, #31538 ),
 ( #19005, #28553, #15830, #3142, #13299, #29190, #11624, #3781, #9285, #16461, #21818, #24833, #11785, #1781, #32533, #9440, #19502, #9597, #1595, #1295, #16636, #29532, #11473, #19326, #19150, #17130, #6278, #9099, #4458, #6621, #14634, #11974, #24652, #6931, #6431, #1952, #27163, #29850, #3965, #26846, #26668, #21988, #16814, #27013, #4267, #4115, #14135, #14283, #24334, #1447, #32028, #24478, #14441, #21669, #32216, #29695, #6776, #12124, #13950, #16964, #22321, #24171, #31876, #8942, #29339, #32381, #22171, #19658, #27339, #25341, #4945, #14942, #10280, #25154, #14789, #32877, #10098, #12276, #2450, #22973, #17319, #20501, #12619, #20007, #22820, #22490, #20157, #30714, #22675, #17813, #12460, #4768, #2274, #4613, #7425, #9944, #20316, #19821, #33024, #7120, #7786, #23169, #27513, #24986, #2097, #30355, #7608, #32705, #17979, #2600, #30526, #7275, #30203, #28167, #30028, #9785, #17623, #17465, #27665, #27828, #15130 ) ),
 .UNSPECIFIED., .F., .F., .F. ) 
 B_SPLINE_SURFACE_WITH_KNOTS ( ( 2, 2 ),
 ( 3, 2, 2, 2, 2, 2, 2, 2, 2, 2, 2, 2, 2, 2, 2, 2, 2, 2, 2, 2, 2, 2, 2, 2, 2, 2, 2, 2, 2, 2, 2, 2, 2, 2, 2, 2, 2, 2, 2, 2, 2, 2, 2, 2, 2, 2, 2, 2, 2, 2, 2, 2, 2, 2, 2, 2, 2, 2, 2, 2, 3 ),
 ( 0.000000000000000000, 1.000000000000000000 ),
 ( 0.000000000000000000, 0.01562500000000000000, 0.03125000000000000000, 0.04687500000000000000, 0.06250000000000000000, 0.07812500000000000000, 0.09375000000000000000, 0.1093750000000000000, 0.1250000000000000000, 0.1406250000000000000, 0.1562500000000000000, 0.1718750000000000000, 0.1875000000000000000, 0.2031250000000000000, 0.2187500000000000000, 0.2343750000000000000, 0.2500000000000000000, 0.2656250000000000000, 0.2812500000000000000, 0.2968750000000000000, 0.3125000000000000000, 0.3281250000000000000, 0.3437500000000000000, 0.3593750000000000000, 0.3750000000000000000, 0.3906250000000000000, 0.4062500000000000000, 0.4218750000000000000, 0.4375000000000000000, 0.4531250000000000000, 0.4687500000000000000, 0.4843750000000000000, 0.5000000000000000000, 0.5156250000000000000, 0.5312500000000000000, 0.5468750000000000000, 0.5625000000000000000, 0.5781250000000000000, 0.5937500000000000000, 0.6093750000000000000, 0.6250000000000000000, 0.6406250000000000000, 0.6562500000000000000, 0.6718750000000000000, 0.6875000000000000000, 0.7031250000000000000, 0.7187500000000000000, 0.7343750000000000000, 0.7500000000000000000, 0.7656250000000000000, 0.7812500000000000000, 0.7968750000000000000, 0.8125000000000000000, 0.8281250000000000000, 0.8437500000000000000, 0.8593750000000000000, 0.8750000000000000000, 0.8906250000000000000, 0.9062500000000000000, 0.9218750000000000000, 0.9375000000000000000 ),
 .UNSPECIFIED. ) 
 GEOMETRIC_REPRESENTATION_ITEM ( )  RATIONAL_B_SPLINE_SURFACE ( (
 ( 1.000000000000000000, 0.9238795325112867385, 1.000000000000000000, 0.9238795325112867385, 1.000000000000000000, 0.9238795325112867385, 1.000000000000000000, 0.9238795325112867385, 1.000000000000000000, 0.9238795325112867385, 1.000000000000000000, 0.9238795325112867385, 1.000000000000000000, 0.9238795325112867385, 1.000000000000000000, 0.9238795325112867385, 1.000000000000000000, 0.9238795325112867385, 1.000000000000000000, 0.9238795325112867385, 1.000000000000000000, 0.9238795325112867385, 1.000000000000000000, 0.9238795325112867385, 1.000000000000000000, 0.9238795325112867385, 1.000000000000000000, 0.9238795325112867385, 1.000000000000000000, 0.9238795325112867385, 1.000000000000000000, 0.9238795325112867385, 1.000000000000000000, 0.9238795325112867385, 1.000000000000000000, 0.9238795325112867385, 1.000000000000000000, 0.9238795325112867385, 1.000000000000000000, 0.9238795325112867385, 1.000000000000000000, 0.9238795325112867385, 1.000000000000000000, 0.9238795325112867385, 1.000000000000000000, 0.9238795325112867385, 1.000000000000000000, 0.9238795325112867385, 1.000000000000000000, 0.9238795325112867385, 1.000000000000000000, 0.9238795325112867385, 1.000000000000000000, 0.9238795325112867385, 1.000000000000000000, 0.9238795325112867385, 1.000000000000000000, 0.9238795325112867385, 1.000000000000000000, 0.9238795325112867385, 1.000000000000000000, 0.9238795325112867385, 1.000000000000000000, 0.9238795325112867385, 1.000000000000000000, 0.9238795325112867385, 1.000000000000000000, 0.9238795325112867385, 1.000000000000000000, 0.9238795325112867385, 1.000000000000000000, 0.9238795325112867385, 1.000000000000000000, 0.9238795325112867385, 1.000000000000000000, 0.9238795325112867385, 1.000000000000000000, 0.9238795325112867385, 1.000000000000000000, 0.9238795325112867385, 1.000000000000000000, 0.9238795325112867385, 1.000000000000000000, 0.9238795325112867385, 1.000000000000000000, 0.9238795325112867385, 1.000000000000000000, 0.9238795325112867385, 1.000000000000000000, 0.9238795325112867385, 1.000000000000000000, 0.9238795325112867385, 1.000000000000000000, 0.9238795325112867385, 1.000000000000000000, 0.9238795325112867385, 1.000000000000000000, 0.9238795325112867385, 1.000000000000000000, 0.9238795325112867385, 1.000000000000000000, 0.9238795325112867385, 1.000000000000000000, 0.9238795325112867385, 1.000000000000000000, 0.9238795325112867385, 1.000000000000000000, 0.9238795325112867385, 1.000000000000000000, 0.9238795325112867385, 1.000000000000000000, 0.9238795325112867385, 1.000000000000000000, 0.9238795325112867385, 1.000000000000000000, 0.9238795325112867385, 1.000000000000000000, 0.9238795325112867385, 1.000000000000000000, 0.9238795325112867385, 1.000000000000000000),
 ( 1.000000000000000000, 0.9238795325112867385, 1.000000000000000000, 0.9238795325112867385, 1.000000000000000000, 0.9238795325112867385, 1.000000000000000000, 0.9238795325112867385, 1.000000000000000000, 0.9238795325112867385, 1.000000000000000000, 0.9238795325112867385, 1.000000000000000000, 0.9238795325112867385, 1.000000000000000000, 0.9238795325112867385, 1.000000000000000000, 0.9238795325112867385, 1.000000000000000000, 0.9238795325112867385, 1.000000000000000000, 0.9238795325112867385, 1.000000000000000000, 0.9238795325112867385, 1.000000000000000000, 0.9238795325112867385, 1.000000000000000000, 0.9238795325112867385, 1.000000000000000000, 0.9238795325112867385, 1.000000000000000000, 0.9238795325112867385, 1.000000000000000000, 0.9238795325112867385, 1.000000000000000000, 0.9238795325112867385, 1.000000000000000000, 0.9238795325112867385, 1.000000000000000000, 0.9238795325112867385, 1.000000000000000000, 0.9238795325112867385, 1.000000000000000000, 0.9238795325112867385, 1.000000000000000000, 0.9238795325112867385, 1.000000000000000000, 0.9238795325112867385, 1.000000000000000000, 0.9238795325112867385, 1.000000000000000000, 0.9238795325112867385, 1.000000000000000000, 0.9238795325112867385, 1.000000000000000000, 0.9238795325112867385, 1.000000000000000000, 0.9238795325112867385, 1.000000000000000000, 0.9238795325112867385, 1.000000000000000000, 0.9238795325112867385, 1.000000000000000000, 0.9238795325112867385, 1.000000000000000000, 0.9238795325112867385, 1.000000000000000000, 0.9238795325112867385, 1.000000000000000000, 0.9238795325112867385, 1.000000000000000000, 0.9238795325112867385, 1.000000000000000000, 0.9238795325112867385, 1.000000000000000000, 0.9238795325112867385, 1.000000000000000000, 0.9238795325112867385, 1.000000000000000000, 0.9238795325112867385, 1.000000000000000000, 0.9238795325112867385, 1.000000000000000000, 0.9238795325112867385, 1.000000000000000000, 0.9238795325112867385, 1.000000000000000000, 0.9238795325112867385, 1.000000000000000000, 0.9238795325112867385, 1.000000000000000000, 0.9238795325112867385, 1.000000000000000000, 0.9238795325112867385, 1.000000000000000000, 0.9238795325112867385, 1.000000000000000000, 0.9238795325112867385, 1.000000000000000000, 0.9238795325112867385, 1.000000000000000000, 0.9238795325112867385, 1.000000000000000000, 0.9238795325112867385, 1.000000000000000000, 0.9238795325112867385, 1.000000000000000000, 0.9238795325112867385, 1.000000000000000000, 0.9238795325112867385, 1.000000000000000000, 0.9238795325112867385, 1.000000000000000000, 0.9238795325112867385, 1.000000000000000000, 0.9238795325112867385, 1.000000000000000000, 0.9238795325112867385, 1.000000000000000000, 0.9238795325112867385, 1.000000000000000000) ) ) 
 REPRESENTATION_ITEM ( '' )  SURFACE ( )  );
#18389 = AXIS2_PLACEMENT_3D ( 'NONE', #7157, #27693, #2632 ) ;
#18390 = CARTESIAN_POINT ( 'NONE',  ( 108.6457025336241031, 16.11621187055573046, -2.334455007174250696 ) ) ;
#18391 = CARTESIAN_POINT ( 'NONE',  ( 108.1300413742128086, -19.94772548867798179, 1.389623142577374626 ) ) ;
#18392 = ORIENTED_EDGE ( 'NONE', *, *, #5221, .F. ) ;
#18393 = CARTESIAN_POINT ( 'NONE',  ( -8.000050800000000351, 0.000000000000000000, -3.000000000000000444 ) ) ;
#18394 = CARTESIAN_POINT ( 'NONE',  ( -23.54713438637982748, 2.712271330416904380, 6.352360439504502132 ) ) ;
#18395 = CARTESIAN_POINT ( 'NONE',  ( 2.866494652520772846, -9.241976615239517301, 2.300561732649529123 ) ) ;
#18396 = ADVANCED_FACE ( 'NONE', ( #19192 ), #4154, .F. ) ;
#18397 = CC_DESIGN_SECURITY_CLASSIFICATION ( #8765, ( #33101 ) ) ;
#18398 = CARTESIAN_POINT ( 'NONE',  ( 2.717504505341735932, -0.4236608596156875017, -1.500000000000000000 ) ) ;
#18399 = CARTESIAN_POINT ( 'NONE',  ( 35.27266127981243926, -8.248087266147095420, 1.169950777418872212 ) ) ;
#18400 = ORIENTED_EDGE ( 'NONE', *, *, #9027, .T. ) ;
#18401 = FACE_OUTER_BOUND ( 'NONE', #23491, .T. ) ;
#18402 = EDGE_CURVE ( 'NONE', #572, #9138, #3520, .T. ) ;
#18403 = B_SPLINE_CURVE_WITH_KNOTS ( 'NONE', 3,
 ( #16777, #11252, #24441, #21780, #1558, #24603, #22133, #6095 ),
 .UNSPECIFIED., .F., .F.,
 ( 4, 2, 2, 4 ),
 ( 2.024520226885745157E-07, 0.001227962984611320404, 0.001841843250905638406, 0.002455723517199956841 ),
 .UNSPECIFIED. ) ;
#18404 = VERTEX_POINT ( 'NONE', #1337 ) ;
#18405 = PERSON_AND_ORGANIZATION ( #6766, #25292 ) ;
#18406 = CARTESIAN_POINT ( 'NONE',  ( 85.13613392229180477, -2.069934983084472879, 2.713652344655542503 ) ) ;
#18407 = EDGE_CURVE ( 'NONE', #26134, #28186, #6168, .T. ) ;
#18408 = VERTEX_POINT ( 'NONE', #13676 ) ;
#18409 = AXIS2_PLACEMENT_3D ( 'NONE', #7110, #7601, #17312 ) ;
#18410 = CARTESIAN_POINT ( 'NONE',  ( 7.418618974160530399, -8.736763461978926060, -0.9999999999999997780 ) ) ;
#18411 = ORIENTED_EDGE ( 'NONE', *, *, #32065, .F. ) ;
#18412 = DIRECTION ( 'NONE',  ( 1.000000000000000000, -0.000000000000000000, -0.000000000000000000 ) ) ;
#18414 = ORIENTED_EDGE ( 'NONE', *, *, #171, .F. ) ;
#18413 = CARTESIAN_POINT ( 'NONE',  ( 40.87869491147504419, -5.924290355801652197, -4.185347298794283688 ) ) ;
#18415 = VERTEX_POINT ( 'NONE', #14002 ) ;
#18416 = CARTESIAN_POINT ( 'NONE',  ( 0.000000000000000000, 0.000000000000000000, 0.000000000000000000 ) ) ;
#18417 = CARTESIAN_POINT ( 'NONE',  ( -5.312550801365593323, 1.088641768524161613, 3.675193018007246959 ) ) ;
#18418 = CARTESIAN_POINT ( 'NONE',  ( 16.05919002109159521, -15.28992581341320545, 1.499999999999999778 ) ) ;
#18419 = ADVANCED_FACE ( 'NONE', ( #3663 ), #29230, .F. ) ;
#18420 = CARTESIAN_POINT ( 'NONE',  ( 107.6125222110667039, -19.71405102733161741, -3.024918492460353381 ) ) ;
#18422 = ORIENTED_EDGE ( 'NONE', *, *, #13121, .F. ) ;
#18421 = CARTESIAN_POINT ( 'NONE',  ( 0.000000000000000000, -5.227991826304158707, 9.620177616657965558 ) ) ;
#18423 = CARTESIAN_POINT ( 'NONE',  ( 107.6236081988486859, -19.87368190684284386, 2.697742887155947233 ) ) ;
#18424 = CARTESIAN_POINT ( 'NONE',  ( 17.92222975117456230, 13.44085466222674619, 1.500000000000000000 ) ) ;
#18425 = CARTESIAN_POINT ( 'NONE',  ( -1.691799335042641683, -13.40595961238992828, 1.500000000000560219 ) ) ;
#18426 = CARTESIAN_POINT ( 'NONE',  ( 0.000000000000000000, -7.944914065997164876, 7.533794289458026761 ) ) ;
#18427 = FACE_OUTER_BOUND ( 'NONE', #23653, .T. ) ;
#18429 = ORIENTED_EDGE ( 'NONE', *, *, #29842, .T. ) ;
#18428 = CARTESIAN_POINT ( 'NONE',  ( 22.16007320322839647, -17.32365168620649953, 1.743368838329871995 ) ) ;
#18430 = LINE ( 'NONE', #20613, #24242 ) ;
#18431 = CARTESIAN_POINT ( 'NONE',  ( -27.53304292598423331, 17.01599196463006436, 1.807868844288452070 ) ) ;
#18432 = CARTESIAN_POINT ( 'NONE',  ( 24.42250000273118715, 1.291182301015469047, 2.378061970571981654 ) ) ;
#18433 = EDGE_CURVE ( 'NONE', #10617, #993, #25924, .T. ) ;
#18434 = CARTESIAN_POINT ( 'NONE',  ( 10.00000000000000000, -1.625881193364669075, -4.467071865485488402 ) ) ;
#18435 = CARTESIAN_POINT ( 'NONE',  ( 78.40736801748178664, 24.56822898102832653, 4.629213727441585213 ) ) ;
#18436 = CARTESIAN_POINT ( 'NONE',  ( -2.619378609982131234, -0.1905507107690968260, -1.628225384166318346 ) ) ;
#18437 = CARTESIAN_POINT ( 'NONE',  ( 108.0105421681096942, -18.22116671483598438, 4.637827421830889918 ) ) ;
#18438 = CARTESIAN_POINT ( 'NONE',  ( 0.000000000000000000, 6.100541242131516384, -3.528937025535512362 ) ) ;
#18439 = ORIENTED_EDGE ( 'NONE', *, *, #1883, .F. ) ;
#18440 = DIRECTION ( 'NONE',  ( -7.023442172597900002E-17, -0.8191520442889969056, 0.5735764363510388320 ) ) ;
#18441 = DIRECTION ( 'NONE',  ( 0.000000000000000000, 0.000000000000000000, 1.000000000000000000 ) ) ;
#18442 = CARTESIAN_POINT ( 'NONE',  ( 2.600000000000000089, 0.000000000000000000, -1.500000000000000444 ) ) ;
#18444 = CARTESIAN_POINT ( 'NONE',  ( 107.9482554908978500, -17.32425405796034568, 4.517001157681336920 ) ) ;
#18443 = CARTESIAN_POINT ( 'NONE',  ( 108.0849451456563628, 18.65116801364982990, -4.602065642979003890 ) ) ;
#18445 = ORIENTED_EDGE ( 'NONE', *, *, #13651, .T. ) ;
#18446 = CARTESIAN_POINT ( 'NONE',  ( 15.05218482013242820, 8.633077639384330482, 1.050000000000000044 ) ) ;
#18447 = ORIENTED_EDGE ( 'NONE', *, *, #31005, .F. ) ;
#18448 = CARTESIAN_POINT ( 'NONE',  ( -2.609487367013886505, -0.08210191867241613262, 1.553472644056475449 ) ) ;
#18450 = EDGE_LOOP ( 'NONE', ( #19791, #16068, #9877, #31731 ) ) ;
#18449 = FACE_OUTER_BOUND ( 'NONE', #4500, .T. ) ;
#18451 = VERTEX_POINT ( 'NONE', #19040 ) ;
#18452 = CARTESIAN_POINT ( 'NONE',  ( -10.00000000000000000, 0.000000000000000000, 0.000000000000000000 ) ) ;
#18453 = DIRECTION ( 'NONE',  ( 0.9896144216807901683, -0.000000000000000000, 0.1437473352845036190 ) ) ;
#18455 = ORIENTED_EDGE ( 'NONE', *, *, #11663, .T. ) ;
#18454 = CARTESIAN_POINT ( 'NONE',  ( 5.885541806331897163, -3.871259391815505602, 7.447669719165321389 ) ) ;
#18456 = PLANE ( 'NONE',  #20456 ) ;
#18457 = CARTESIAN_POINT ( 'NONE',  ( -4.027720362024412637, -8.337845212197136036, -1.744153996925280392 ) ) ;
#18458 = B_SPLINE_CURVE_WITH_KNOTS ( 'NONE', 3,
 ( #9577, #27144, #19797, #1760, #17450, #24628, #30003, #22804 ),
 .UNSPECIFIED., .F., .F.,
 ( 4, 2, 2, 4 ),
 ( 2.049880227679818068E-07, 0.001227965543375839899, 0.001841845821052373383, 0.002455726098728907084 ),
 .UNSPECIFIED. ) ;
#18459 = CARTESIAN_POINT ( 'NONE',  ( 18.69152969128558084, -6.625301692630690908, 2.790665661679905707 ) ) ;
#18460 = CARTESIAN_POINT ( 'NONE',  ( 24.38441422956718085, -17.22282062799148150, -1.499999999997775779 ) ) ;
#18461 = DIRECTION ( 'NONE',  ( -0.000000000000000000, -0.000000000000000000, -1.000000000000000000 ) ) ;
#18462 = CARTESIAN_POINT ( 'NONE',  ( 107.8864559843597988, -16.43435653759661363, 1.556338746034127363 ) ) ;
#18463 = CARTESIAN_POINT ( 'NONE',  ( 0.000000000000000000, -5.522688772756442432, 6.461416928141223259 ) ) ;
#18464 = CARTESIAN_POINT ( 'NONE',  ( 21.08401840680159367, -16.78474387324287775, 1.500000000000000000 ) ) ;
#18465 = CYLINDRICAL_SURFACE ( 'NONE', #16775, 8.025310301077734465 ) ;
#18466 = EDGE_CURVE ( 'NONE', #26782, #5049, #26894, .T. ) ;
#18467 = DIRECTION ( 'NONE',  ( 0.8571673007021120005, 0.000000000000000000, 0.5150380749100547106 ) ) ;
#18468 = CARTESIAN_POINT ( 'NONE',  ( 7.064423669210280643, 5.064320921489786187, -7.135485519863410175 ) ) ;
#18469 = VERTEX_POINT ( 'NONE', #6315 ) ;
#18470 = FACE_OUTER_BOUND ( 'NONE', #8914, .T. ) ;
#18471 = ADVANCED_FACE ( 'NONE', ( #24215 ), #24370, .F. ) ;
#18472 = CARTESIAN_POINT ( 'NONE',  ( 29.32519546910717168, -5.313460878238876361, 5.695980980372492120 ) ) ;
#18473 = CARTESIAN_POINT ( 'NONE',  ( 32.37020706055089647, 18.00000000000000355, -0.7246014581832489476 ) ) ;
#18474 = VERTEX_POINT ( 'NONE', #6664 ) ;
#18475 = CARTESIAN_POINT ( 'NONE',  ( 23.23500000136559862, -3.156283516753370044, -0.9349337715887220401 ) ) ;
#18476 = B_SPLINE_CURVE_WITH_KNOTS ( 'NONE', 3,
 ( #26508, #26822, #3944, #8598, #21967, #11114, #31702, #14116 ),
 .UNSPECIFIED., .F., .F.,
 ( 4, 2, 2, 4 ),
 ( 2.049880227734711626E-07, 0.001227965543376307840, 0.001841845821053075078, 0.002455726098729842533 ),
 .UNSPECIFIED. ) ;
#18477 = CARTESIAN_POINT ( 'NONE',  ( 25.39550262306211792, -2.656620010619367811, 0.2256117632562368858 ) ) ;
#18478 = DIRECTION ( 'NONE',  ( -0.000000000000000000, 1.000000000000000000, 1.224646799147353207E-16 ) ) ;
#18479 = VERTEX_POINT ( 'NONE', #23878 ) ;
#18480 = CARTESIAN_POINT ( 'NONE',  ( 18.81968334181831892, -5.192801080986814810, -4.312047644171949301 ) ) ;
#18481 = ORIENTED_EDGE ( 'NONE', *, *, #29402, .T. ) ;
#18482 = DIRECTION ( 'NONE',  ( 0.4999999999999978351, 0.8660254037844399289, 0.000000000000000000 ) ) ;
#18483 = APPROVAL_DATE_TIME ( #21161, #27393 ) ;
#18485 = ORIENTED_EDGE ( 'NONE', *, *, #2496, .T. ) ;
#18484 = CARTESIAN_POINT ( 'NONE',  ( 28.66386174152028588, -4.482150724279978071, -2.184956778825816848 ) ) ;
#18486 = EDGE_LOOP ( 'NONE', ( #21552, #766, #7617 ) ) ;
#18487 = CARTESIAN_POINT ( 'NONE',  ( 25.11000000136559507, -3.156283516753370488, -0.9349337715887220401 ) ) ;
#18488 = EDGE_LOOP ( 'NONE', ( #16722, #32813, #20411, #15251 ) ) ;
#18489 = CARTESIAN_POINT ( 'NONE',  ( -7.600050800000000883, 2.331437884370912705, -1.887961173149511618 ) ) ;
#18491 = VERTEX_POINT ( 'NONE', #21859 ) ;
#18490 = CARTESIAN_POINT ( 'NONE',  ( 54.89716490669064797, -3.628845007888691132, -0.4367666026988534789 ) ) ;
#18492 = CARTESIAN_POINT ( 'NONE',  ( 0.5640493910637760511, 6.134141009795983202, -7.306425354220267288 ) ) ;
#18493 = CARTESIAN_POINT ( 'NONE',  ( 108.0320971364573239, -18.53155289684145046, 4.239511015329910926 ) ) ;
#18494 = PLANE ( 'NONE',  #19709 ) ;
#18495 = DIRECTION ( 'NONE',  ( 0.000000000000000000, 0.4226182617407134856, -0.9063077870366433864 ) ) ;
#18496 = ORIENTED_EDGE ( 'NONE', *, *, #20488, .T. ) ;
#18497 = DIRECTION ( 'NONE',  ( -1.000000000000000000, 0.000000000000000000, 0.000000000000000000 ) ) ;
#18498 = CARTESIAN_POINT ( 'NONE',  ( 72.72614267428248525, -20.12349919388105945, -5.485967528433937979 ) ) ;
#18499 = CARTESIAN_POINT ( 'NONE',  ( 35.27427105688909847, -8.145327135406411401, -1.529339875379911229 ) ) ;
#18500 = EDGE_CURVE ( 'NONE', #23437, #13750, #16854, .T. ) ;
#18501 = CARTESIAN_POINT ( 'NONE',  ( 2.501106528969298193, 0.1614173311939657851, -1.446082916213565106 ) ) ;
#18502 = EDGE_CURVE ( 'NONE', #3656, #17188, #31581, .T. ) ;
#18503 = ADVANCED_FACE ( 'NONE', ( #11662 ), #16223, .F. ) ;
#18504 = CARTESIAN_POINT ( 'NONE',  ( -8.000050800000000351, -1.393745829612481169, 2.767030136172837107 ) ) ;
#18505 = PLANE ( 'NONE',  #4900 ) ;
#18506 = CARTESIAN_POINT ( 'NONE',  ( 2.425585535373192325, 9.314797388894900720, 5.239665997526921970 ) ) ;
#18507 = CARTESIAN_POINT ( 'NONE',  ( 5.885541838704148709, -6.662285765435181695, -5.105720535585480668 ) ) ;
#18508 = CARTESIAN_POINT ( 'NONE',  ( 28.72212596679959162, -4.487363129042812204, 2.184956778824082235 ) ) ;
#18509 = CARTESIAN_POINT ( 'NONE',  ( -4.562550801365594211, 2.228590825266444142, 2.752080473201636845 ) ) ;
#18510 = ORIENTED_EDGE ( 'NONE', *, *, #27453, .T. ) ;
#18511 = CARTESIAN_POINT ( 'NONE',  ( -3.404531657079157281, 1.883076972206379374, 2.325406398514293205 ) ) ;
#18512 = B_SPLINE_CURVE_WITH_KNOTS ( 'NONE', 3,
 ( #32390, #22330, #24844, #9955, #12133, #32542 ),
 .UNSPECIFIED., .F., .F.,
 ( 4, 2, 4 ),
 ( 0.0003940451885343313073, 0.001458980440401463040, 0.002523915692268594718 ),
 .UNSPECIFIED. ) ;
#18513 = CARTESIAN_POINT ( 'NONE',  ( -7.712942406915323623, 7.727249047114547632E-16, -2.999999999999999556 ) ) ;
#18514 = CYLINDRICAL_SURFACE ( 'NONE', #2878, 0.4499999999999990119 ) ;
#18515 = CARTESIAN_POINT ( 'NONE',  ( 9.037136197880096589, -11.91234824294609140, 1.500000000000000000 ) ) ;
#18516 = ORIENTED_EDGE ( 'NONE', *, *, #28693, .F. ) ;
#18517 = CARTESIAN_POINT ( 'NONE',  ( 84.91897426281094852, -3.309433673474704296, -2.787781823995287844 ) ) ;
#18518 = ORIENTED_EDGE ( 'NONE', *, *, #14468, .F. ) ;
#18519 = CARTESIAN_POINT ( 'NONE',  ( 0.6278659085242910276, -4.203768939204204358, 1.500000000000068390 ) ) ;
#18520 = PERSON_AND_ORGANIZATION ( #6766, #25292 ) ;
#18521 = CARTESIAN_POINT ( 'NONE',  ( 28.66985322744079312, -6.539611658484044021, 4.215290389448495212 ) ) ;
#18522 = CARTESIAN_POINT ( 'NONE',  ( 3.499999999999999556, 1.418488851014487073, -6.085876303339362359 ) ) ;
#18523 = CARTESIAN_POINT ( 'NONE',  ( 5.885541838704153150, 6.662285765435218110, 5.105720535585435371 ) ) ;
#18524 = ORIENTED_EDGE ( 'NONE', *, *, #4689, .F. ) ;
#18525 = CARTESIAN_POINT ( 'NONE',  ( 6.880159790065803804, -8.451885315426441281, 2.190520500543459814 ) ) ;
#18526 = LINE ( 'NONE', #31257, #6484 ) ;
#18527 = CARTESIAN_POINT ( 'NONE',  ( 17.41559371906258136, 18.02474698348857274, -1.500000000000000000 ) ) ;
#18528 = EDGE_CURVE ( 'NONE', #9818, #12294, #28491, .T. ) ;
#18529 = B_SPLINE_CURVE_WITH_KNOTS ( 'NONE', 3,
 ( #20610, #375, #31142, #25600 ),
 .UNSPECIFIED., .F., .F.,
 ( 4, 4 ),
 ( 0.005732069968871694905, 0.4737525964756066910 ),
 .UNSPECIFIED. ) ;
#18531 = EDGE_LOOP ( 'NONE', ( #17481, #2066, #30899 ) ) ;
#18530 = DIRECTION ( 'NONE',  ( 0.000000000000000000, 0.000000000000000000, 1.000000000000000000 ) ) ;
#18532 = CARTESIAN_POINT ( 'NONE',  ( -2.662550801365593411, -3.521866450007987037, -0.3701630799359323931 ) ) ;
#18533 = DIRECTION ( 'NONE',  ( 0.000000000000000000, -0.9063077870366466060, -0.4226182617407066022 ) ) ;
#18534 = DIRECTION ( 'NONE',  ( 0.000000000000000000, -1.000000000000000000, 0.000000000000000000 ) ) ;
#18535 = ORIENTED_EDGE ( 'NONE', *, *, #29522, .T. ) ;
#18536 = ORIENTED_EDGE ( 'NONE', *, *, #25697, .F. ) ;
#18537 = EDGE_CURVE ( 'NONE', #25587, #21122, #16178, .T. ) ;
#18538 = DIRECTION ( 'NONE',  ( -1.000000000000000000, 8.574039729943018344E-17, -0.000000000000000000 ) ) ;
#18539 = DIRECTION ( 'NONE',  ( -1.387778780781445676E-14, -1.000000000000000000, 8.673617379884035472E-16 ) ) ;
#18540 = ADVANCED_FACE ( 'NONE', ( #26940 ), #27250, .T. ) ;
#18541 = CARTESIAN_POINT ( 'NONE',  ( 25.41902038486284354, -17.54124217233828631, 1.046354159564242714 ) ) ;
#18542 = B_SPLINE_CURVE_WITH_KNOTS ( 'NONE', 3,
 ( #26190, #21183, #13466, #8457, #5792, #15827, #16313, #3299, #26035, #29186, #5647, #28850 ),
 .UNSPECIFIED., .F., .F.,
 ( 4, 2, 2, 2, 2, 4 ),
 ( -5.999999999585006259E-08, 0.0007057886787611236407, 0.001058713018141682572, 0.001235175187831967242, 0.001323406272677110120, 0.001411637357522252997 ),
 .UNSPECIFIED. ) ;
#18543 = CARTESIAN_POINT ( 'NONE',  ( 8.911384905465473238, 0.4717275430040264173, 1.041239158277188048 ) ) ;
#18544 = DIRECTION ( 'NONE',  ( 0.000000000000000000, 0.000000000000000000, -1.000000000000000000 ) ) ;
#18545 = EDGE_CURVE ( 'NONE', #3159, #12213, #20346, .T. ) ;
#18546 = CARTESIAN_POINT ( 'NONE',  ( 107.5501783195510370, -18.81539188448605415, -4.846927202741923679 ) ) ;
#18547 = CARTESIAN_POINT ( 'NONE',  ( 1.661358730909628482E-15, -10.85582367538893322, -1.425064293572451790 ) ) ;
#18548 = CARTESIAN_POINT ( 'NONE',  ( 47.95950916398558661, -8.432626694227655761, 0.4367665434690334303 ) ) ;
#18549 = VERTEX_POINT ( 'NONE', #13867 ) ;
#18550 = EDGE_LOOP ( 'NONE', ( #12031, #24261, #8987, #22794 ) ) ;
#18551 = APPROVAL_ROLE ( '' ) ;
#18552 = CARTESIAN_POINT ( 'NONE',  ( 41.43369393131070666, -3.642920876109168926, 2.713652344655542503 ) ) ;
#18553 = ORIENTED_EDGE ( 'NONE', *, *, #3089, .T. ) ;
#18554 = CARTESIAN_POINT ( 'NONE',  ( 3.249999999999999556, 4.286263797015736102E-16, -3.499999999999999556 ) ) ;
#18555 = ORIENTED_EDGE ( 'NONE', *, *, #10499, .F. ) ;
#18556 = CARTESIAN_POINT ( 'NONE',  ( 3.249999999999999556, 0.000000000000000000, 0.000000000000000000 ) ) ;
#18557 = EDGE_CURVE ( 'NONE', #26682, #7898, #1201, .T. ) ;
#18558 = ORIENTED_EDGE ( 'NONE', *, *, #33027, .T. ) ;
#18559 = VERTEX_POINT ( 'NONE', #31802 ) ;
#18560 = LINE ( 'NONE', #8217, #3285 ) ;
#18561 = CARTESIAN_POINT ( 'NONE',  ( -3.712550801365593234, 1.088641768524161613, 3.675193018007246959 ) ) ;
#18562 = CARTESIAN_POINT ( 'NONE',  ( 6.680689650589743067, -6.092366900306463329, 1.500000000000000222 ) ) ;
#18563 = DIRECTION ( 'NONE',  ( 1.000000000000000000, -0.000000000000000000, -0.000000000000000000 ) ) ;
#18564 =( BOUNDED_SURFACE ( )  B_SPLINE_SURFACE ( 3, 3, ( 
 ( #6472, #16350, #19813, #29225, #11164, #30024, #26559, #13996, #21703, #22316, #3659, #984, #13815, #4451, #24211, #3517 ),
 ( #14629, #24829, #29382, #12120, #21369, #1146, #31575, #21550, #26418, #13514, #1333, #31757, #23726, #1947, #3346, #8832 ),
 ( #19037, #6311, #16497, #32528, #11506, #7112, #26705, #840, #16194, #3819, #31911, #8977, #11017, #19188, #9591, #31415 ),
 ( #8490, #18691, #28890, #5998, #25488, #4763, #28011, #10092, #22815, #17805, #7271, #14937, #25648, #7420, #17972, #33020 ) ),
 .UNSPECIFIED., .F., .F., .F. ) 
 B_SPLINE_SURFACE_WITH_KNOTS ( ( 4, 4 ),
 ( 4, 2, 2, 2, 2, 2, 2, 4 ),
 ( 0.000000000000000000, 1.000000000000000000 ),
 ( 0.000000000000000000, 0.5000000000000000000, 0.6250000000000000000, 0.7500000000000000000, 0.8125000000000000000, 0.8750000000000000000, 0.9375000000000000000, 1.000000000000000000 ),
 .UNSPECIFIED. ) 
 GEOMETRIC_REPRESENTATION_ITEM ( )  RATIONAL_B_SPLINE_SURFACE ( (
 ( 1.000000000000000000, 1.000000000000000000, 1.000000000000000000, 1.000000000000000000, 1.000000000000000000, 1.000000000000000000, 1.000000000000000000, 1.000000000000000000, 1.000000000000000000, 1.000000000000000000, 1.000000000000000000, 1.000000000000000000, 1.000000000000000000, 1.000000000000000000, 1.000000000000000000, 1.000000000000000000),
 ( 0.5895302151065218155, 0.5895302151065218155, 0.5895302151065218155, 0.5895302151065218155, 0.5895302151065218155, 0.5895302151065218155, 0.5895302151065218155, 0.5895302151065218155, 0.5895302151065218155, 0.5895302151065218155, 0.5895302151065218155, 0.5895302151065218155, 0.5895302151065218155, 0.5895302151065218155, 0.5895302151065218155, 0.5895302151065218155),
 ( 0.5895302151065218155, 0.5895302151065218155, 0.5895302151065218155, 0.5895302151065218155, 0.5895302151065218155, 0.5895302151065218155, 0.5895302151065218155, 0.5895302151065218155, 0.5895302151065218155, 0.5895302151065218155, 0.5895302151065218155, 0.5895302151065218155, 0.5895302151065218155, 0.5895302151065218155, 0.5895302151065218155, 0.5895302151065218155),
 ( 1.000000000000000000, 1.000000000000000000, 1.000000000000000000, 1.000000000000000000, 1.000000000000000000, 1.000000000000000000, 1.000000000000000000, 1.000000000000000000, 1.000000000000000000, 1.000000000000000000, 1.000000000000000000, 1.000000000000000000, 1.000000000000000000, 1.000000000000000000, 1.000000000000000000, 1.000000000000000000) ) ) 
 REPRESENTATION_ITEM ( '' )  SURFACE ( )  );
#18566 = VERTEX_POINT ( 'NONE', #8873 ) ;
#18565 = CARTESIAN_POINT ( 'NONE',  ( 5.612718622971683224, 7.650113768151216576, -2.996580135471449413 ) ) ;
#18567 = CARTESIAN_POINT ( 'NONE',  ( -7.237550801365592257, 3.675193018007247403, -1.088641768524161391 ) ) ;
#18568 = CARTESIAN_POINT ( 'NONE',  ( 15.21374380700450146, 10.74503379549556037, 1.500000000000000000 ) ) ;
#18569 = CARTESIAN_POINT ( 'NONE',  ( 17.37538333147201186, -21.16291065652713854, 1.500000000000001332 ) ) ;
#18571 = EDGE_CURVE ( 'NONE', #26955, #16550, #10320, .T. ) ;
#18570 = CARTESIAN_POINT ( 'NONE',  ( 21.54750000136559507, 3.024605502323846729, -0.3178988483021056854 ) ) ;
#18572 = PLANE ( 'NONE',  #28833 ) ;
#18574 = EDGE_LOOP ( 'NONE', ( #3971, #9931, #8099, #23298 ) ) ;
#18573 = CARTESIAN_POINT ( 'NONE',  ( 10.00000000000000000, 4.753758587302147731, -3.462581523170085693E-33 ) ) ;
#18575 = EDGE_CURVE ( 'NONE', #6678, #26955, #26344, .T. ) ;
#18576 = B_SPLINE_CURVE_WITH_KNOTS ( 'NONE', 3,
 ( #30397, #14988, #20547, #7976, #12810, #23024, #25207, #2330 ),
 .UNSPECIFIED., .F., .F.,
 ( 4, 2, 2, 4 ),
 ( -5.677916165041726082E-06, 0.0007318671105578830301, 0.001100639623919344836, 0.001469412137280806750 ),
 .UNSPECIFIED. ) ;
#18577 = DIRECTION ( 'NONE',  ( -0.1587661886299353009, -0.9873162094019949375, 0.000000000000000000 ) ) ;
#18578 = CARTESIAN_POINT ( 'NONE',  ( 22.54750000273119070, -0.7685399846772070775, 2.594547506269381465 ) ) ;
#18579 = ADVANCED_FACE ( 'NONE', ( #17400 ), #8388, .T. ) ;
#18580 = CARTESIAN_POINT ( 'NONE',  ( 7.249760686538667009, 6.139290821770257089, 5.151476664237498504 ) ) ;
#18581 = CARTESIAN_POINT ( 'NONE',  ( 18.72466669454978927, -6.254896501190466473, -3.387719717048244483 ) ) ;
#18582 = CARTESIAN_POINT ( 'NONE',  ( -17.45597128428593336, -25.93932300454937945, 10.99999999999999822 ) ) ;
#18583 = LINE ( 'NONE', #28279, #3880 ) ;
#18584 = DIRECTION ( 'NONE',  ( 0.9947025833170223263, 0.1027947991993880261, 0.000000000000000000 ) ) ;
#18585 = ORIENTED_EDGE ( 'NONE', *, *, #11689, .T. ) ;
#18586 = EDGE_CURVE ( 'NONE', #31286, #29455, #30133, .T. ) ;
#18587 = CARTESIAN_POINT ( 'NONE',  ( -2.562942409646512321, -5.022711880624455567E-15, 2.999999999999999556 ) ) ;
#18588 = CARTESIAN_POINT ( 'NONE',  ( -2.976964752645617107, -0.1884360924510954383, -1.392852931015429174 ) ) ;
#18589 = CARTESIAN_POINT ( 'NONE',  ( 23.58234648083103124, -8.048792613723655620, -0.07017451552783530999 ) ) ;
#18591 = CARTESIAN_POINT ( 'NONE',  ( 108.0159574833865292, -18.29914590766157900, 4.591531417968990780 ) ) ;
#18590 = CARTESIAN_POINT ( 'NONE',  ( 3.499999999999999556, 5.241389472434663688, 4.711457988287072851 ) ) ;
#18592 = ORIENTED_EDGE ( 'NONE', *, *, #23692, .F. ) ;
#18593 = LINE ( 'NONE', #28963, #31541 ) ;
#18594 = EDGE_LOOP ( 'NONE', ( #26562, #19209, #28053, #3898 ) ) ;
#18595 = FACE_OUTER_BOUND ( 'NONE', #12397, .T. ) ;
#18597 = ORIENTED_EDGE ( 'NONE', *, *, #489, .T. ) ;
#18596 = CARTESIAN_POINT ( 'NONE',  ( 7.249760686538667009, -8.721381771256204729, -0.7071067811865429098 ) ) ;
#18598 = VERTEX_POINT ( 'NONE', #9698 ) ;
#18599 = DIRECTION ( 'NONE',  ( 1.000000000000000000, -8.574039729943018344E-17, -0.000000000000000000 ) ) ;
#18600 = EDGE_CURVE ( 'NONE', #13681, #19944, #9519, .T. ) ;
#18601 = DIRECTION ( 'NONE',  ( 0.06927878976713817971, -0.9975973382524637723, 0.000000000000000000 ) ) ;
#18603 = ORIENTED_EDGE ( 'NONE', *, *, #24835, .F. ) ;
#18602 = CARTESIAN_POINT ( 'NONE',  ( 107.9842833620133149, 18.09064348308214321, 4.146048564489902333 ) ) ;
#18604 = ORIENTED_EDGE ( 'NONE', *, *, #16898, .T. ) ;
#18605 = CARTESIAN_POINT ( 'NONE',  ( -32.99635089100451069, 0.06958667959533217096, -0.9963508910045062450 ) ) ;
#18606 = CARTESIAN_POINT ( 'NONE',  ( 4.749760686538667009, -7.530955069117533540, 2.741043480754901118 ) ) ;
#18607 = EDGE_CURVE ( 'NONE', #681, #30241, #31177, .T. ) ;
#18608 = CARTESIAN_POINT ( 'NONE',  ( -33.81874022276151237, 20.00000000000000000, -1.818740222761504599 ) ) ;
#18609 = DIRECTION ( 'NONE',  ( 1.000000000000000000, -8.574039729943018344E-17, -0.000000000000000000 ) ) ;
#18610 = PLANE ( 'NONE',  #32662 ) ;
#18611 = CARTESIAN_POINT ( 'NONE',  ( 12.21775235206943755, -15.17036961632329373, 1.500000000000000000 ) ) ;
#18612 = CARTESIAN_POINT ( 'NONE',  ( 23.24967726704456084, -21.43932300456764750, 1.500000000000000000 ) ) ;
#18613 = EDGE_CURVE ( 'NONE', #10070, #26504, #25066, .T. ) ;
#18614 = CARTESIAN_POINT ( 'NONE',  ( 2.974466146320851934, 0.1107971263338725920, 0.9540093664865986200 ) ) ;
#18615 = ORIENTED_EDGE ( 'NONE', *, *, #12169, .F. ) ;
#18616 = CARTESIAN_POINT ( 'NONE',  ( -23.54713438637982748, 6.328288363227374980, 7.813326153826580800 ) ) ;
#18617 = CARTESIAN_POINT ( 'NONE',  ( 107.8323272165537929, 17.24449170613202753, 2.334489955268165939 ) ) ;
#18618 = CARTESIAN_POINT ( 'NONE',  ( 7.249760686538667009, 2.741043480754926875, 7.530955069117522882 ) ) ;
#18619 = ORIENTED_EDGE ( 'NONE', *, *, #2050, .F. ) ;
#18620 = CARTESIAN_POINT ( 'NONE',  ( 24.48500000136559507, 0.9349337715887185984, -3.156283516753368268 ) ) ;
#18621 = EDGE_CURVE ( 'NONE', #228, #7359, #17720, .T. ) ;
#18622 = CC_DESIGN_PERSON_AND_ORGANIZATION_ASSIGNMENT ( #16863, #29400, ( #14051 ) ) ;
#18623 = CARTESIAN_POINT ( 'NONE',  ( 25.56220348721820201, -1.341958225229829886E-11, -2.827203487218203914 ) ) ;
#18624 = CARTESIAN_POINT ( 'NONE',  ( 21.07900179210031411, -21.69205259094561100, -1.492586111082710110 ) ) ;
#18625 = ORIENTED_EDGE ( 'NONE', *, *, #29954, .F. ) ;
#18626 = CARTESIAN_POINT ( 'NONE',  ( 0.6377051968875022681, -7.657409712011349789, -1.500000000000000000 ) ) ;
#18627 = ORIENTED_EDGE ( 'NONE', *, *, #4183, .F. ) ;
#18628 = ORIENTED_EDGE ( 'NONE', *, *, #24798, .F. ) ;
#18629 = CARTESIAN_POINT ( 'NONE',  ( 25.45368006873471955, -17.55541207042469765, -1.083666005368261409 ) ) ;
#18631 = VERTEX_POINT ( 'NONE', #10027 ) ;
#18630 = CARTESIAN_POINT ( 'NONE',  ( 10.55147673363118876, 2.285372942705016452, -4.458382051008168645 ) ) ;
#18632 = ORIENTED_EDGE ( 'NONE', *, *, #1018, .F. ) ;
#18633 = DIRECTION ( 'NONE',  ( 1.000000000000000000, 0.000000000000000000, 0.000000000000000000 ) ) ;
#18634 = ADVANCED_FACE ( 'NONE', ( #32805 ), #3637, .T. ) ;
#18635 = ORIENTED_EDGE ( 'NONE', *, *, #17157, .T. ) ;
#18636 = CARTESIAN_POINT ( 'NONE',  ( 6.357667408475528248, 0.5738000813810777423, -8.588075071450642639 ) ) ;
#18638 = ORIENTED_EDGE ( 'NONE', *, *, #20097, .F. ) ;
#18637 = CARTESIAN_POINT ( 'NONE',  ( 0.9499999999999995115, 8.572527594031471218E-16, 6.999999999999998224 ) ) ;
#18639 = CARTESIAN_POINT ( 'NONE',  ( 21.86000000273118715, -1.942864903642428587, -1.573300977624592756 ) ) ;
#18640 = DIRECTION ( 'NONE',  ( 0.000000000000000000, 0.000000000000000000, 1.000000000000000000 ) ) ;
#18641 = EDGE_CURVE ( 'NONE', #18983, #23564, #27511, .T. ) ;
#18642 = LINE ( 'NONE', #28839, #29894 ) ;
#18643 = DIRECTION ( 'NONE',  ( -0.000000000000000000, 0.000000000000000000, 1.000000000000000000 ) ) ;
#18644 = CARTESIAN_POINT ( 'NONE',  ( 107.5592006082064529, -18.94629055990540678, 4.613091233250001366 ) ) ;
#18645 = CARTESIAN_POINT ( 'NONE',  ( -56.28351068137280322, 0.4500000000000000111, 1.500000000000000000 ) ) ;
#18646 = CYLINDRICAL_SURFACE ( 'NONE', #1734, 8.500000000000000000 ) ;
#18647 = CARTESIAN_POINT ( 'NONE',  ( 47.95695783165756154, -8.278479088712042966, -1.169950612933553513 ) ) ;
#18648 = CARTESIAN_POINT ( 'NONE',  ( -6.562942409646512765, -8.831141768130910875E-16, 2.999999999999999556 ) ) ;
#18649 = CYLINDRICAL_SURFACE ( 'NONE', #23021, 2.099999999999994316 ) ;
#18650 = DIRECTION ( 'NONE',  ( -1.000000000000000000, -0.000000000000000000, 0.000000000000000000 ) ) ;
#18651 = CARTESIAN_POINT ( 'NONE',  ( 2.274274201627289216, 9.680994141364161365, 5.222868219167314585 ) ) ;
#18652 = LINE ( 'NONE', #18351, #25201 ) ;
#18653 = CARTESIAN_POINT ( 'NONE',  ( 21.73499999999999943, -0.2613211581691358698, -2.486304738420681559 ) ) ;
#18654 = CARTESIAN_POINT ( 'NONE',  ( -3.412550801365593411, -3.368539882008727115, -1.828967928396028064 ) ) ;
#18655 = VERTEX_POINT ( 'NONE', #7358 ) ;
#18656 = CARTESIAN_POINT ( 'NONE',  ( -5.100050799999999995, 2.983565686104819648, 0.3135853898029609677 ) ) ;
#18657 = AXIS2_PLACEMENT_3D ( 'NONE', #11063, #31462, #15589 ) ;
#18658 = B_SPLINE_CURVE_WITH_KNOTS ( 'NONE', 3,
 ( #17218, #6841, #9180, #11690, #21888, #14703 ),
 .UNSPECIFIED., .F., .F.,
 ( 4, 2, 4 ),
 ( -2.095334690189621038E-05, 0.001971868223395999934, 0.003964689793693895736 ),
 .UNSPECIFIED. ) ;
#18659 = VECTOR ( 'NONE', #16393, 1000.000000000000114 ) ;
#18660 = CARTESIAN_POINT ( 'NONE',  ( 8.007433738499960540, 15.00000000000002132, -5.396302277755718357 ) ) ;
#18661 = DIRECTION ( 'NONE',  ( 1.000000000000000000, -0.000000000000000000, -0.000000000000000000 ) ) ;
#18662 = CARTESIAN_POINT ( 'NONE',  ( 7.502484982177588080, -10.19046547981977291, 1.500000000000000000 ) ) ;
#18663 = EDGE_LOOP ( 'NONE', ( #21761, #6167, #9141, #2781 ) ) ;
#18664 = CARTESIAN_POINT ( 'NONE',  ( 84.96516786084956152, -4.058994088351913554, -3.993433528812653677 ) ) ;
#18665 = AXIS2_PLACEMENT_3D ( 'NONE', #10969, #21654, #26653 ) ;
#18666 = ORIENTED_EDGE ( 'NONE', *, *, #12253, .T. ) ;
#18667 = CARTESIAN_POINT ( 'NONE',  ( 7.249760686538667009, 5.064320921489820826, 7.135485519862015735 ) ) ;
#18668 = PERSON_AND_ORGANIZATION_ROLE ( 'design_supplier' ) ;
#18669 = CARTESIAN_POINT ( 'NONE',  ( 54.96481031288562491, -6.058022586631627959, 4.312042181580753031 ) ) ;
#18670 = EDGE_CURVE ( 'NONE', #19623, #14119, #17547, .T. ) ;
#18671 = ADVANCED_FACE ( 'NONE', ( #848 ), #9787, .T. ) ;
#18672 = DIRECTION ( 'NONE',  ( -1.000000000000000000, 0.000000000000000000, 0.000000000000000000 ) ) ;
#18673 = CARTESIAN_POINT ( 'NONE',  ( 10.47272779071480819, 17.64623289522323191, 5.412820279296879811 ) ) ;
#18674 = ORIENTED_EDGE ( 'NONE', *, *, #30206, .F. ) ;
#18675 = DIRECTION ( 'NONE',  ( 1.000000000000000000, 0.000000000000000000, 0.000000000000000000 ) ) ;
#18676 = FACE_OUTER_BOUND ( 'NONE', #6107, .T. ) ;
#18677 = CARTESIAN_POINT ( 'NONE',  ( 7.249760686538667009, 8.711672189281440382, -0.8180878109960949551 ) ) ;
#18678 = AXIS2_PLACEMENT_3D ( 'NONE', #12360, #17895, #22579 ) ;
#18680 = VERTEX_POINT ( 'NONE', #16012 ) ;
#18679 = LINE ( 'NONE', #26406, #8016 ) ;
#18681 = CARTESIAN_POINT ( 'NONE',  ( -2.062550801365593323, -0.3701630799359326152, 3.521866450007987037 ) ) ;
#18682 = AXIS2_PLACEMENT_3D ( 'NONE', #25673, #17999, #22841 ) ;
#18683 = B_SPLINE_CURVE_WITH_KNOTS ( 'NONE', 3,
 ( #22669, #27335, #4450, #16960 ),
 .UNSPECIFIED., .F., .F.,
 ( 4, 4 ),
 ( 0.001719859957800634609, 0.002523933526961084049 ),
 .UNSPECIFIED. ) ;
#18684 = CARTESIAN_POINT ( 'NONE',  ( 3.499999999999999556, -0.1221666339523235223, -6.247805719894684806 ) ) ;
#18685 = LINE ( 'NONE', #26065, #10734 ) ;
#18686 = ORIENTED_EDGE ( 'NONE', *, *, #27160, .T. ) ;
#18687 = VERTEX_POINT ( 'NONE', #30937 ) ;
#18688 = CARTESIAN_POINT ( 'NONE',  ( 7.249760686538667009, 8.466096581343482086, 2.210816291636243047 ) ) ;
#18689 = CARTESIAN_POINT ( 'NONE',  ( 0.000000000000000000, 0.000000000000000000, 0.000000000000000000 ) ) ;
#18690 = DIRECTION ( 'NONE',  ( -0.1385137909583552540, 0.9903605049245174374, 0.000000000000000000 ) ) ;
#18691 = CARTESIAN_POINT ( 'NONE',  ( 72.52374898132083558, -19.78015497543642809, 4.522129901861156931 ) ) ;
#18692 = ORIENTED_EDGE ( 'NONE', *, *, #16688, .F. ) ;
#18693 = CARTESIAN_POINT ( 'NONE',  ( 25.02099912015120609, -17.46522996914712422, 1.208347673492914165 ) ) ;
#18694 = DIRECTION ( 'NONE',  ( -1.000000000000000000, 0.000000000000000000, 0.000000000000000000 ) ) ;
#18695 = CARTESIAN_POINT ( 'NONE',  ( -1.783740934873500272, -0.1784080614500640760, 3.046698672529837726 ) ) ;
#18696 = CARTESIAN_POINT ( 'NONE',  ( -4.537550801365592967, -1.828967928396026732, 3.368539882008728004 ) ) ;
#18697 = AXIS2_PLACEMENT_3D ( 'NONE', #5504, #23526, #3014 ) ;
#18698 = DIRECTION ( 'NONE',  ( -6.062761635205527683E-17, -0.7071067811865410224, -0.7071067811865540120 ) ) ;
#18699 = CARTESIAN_POINT ( 'NONE',  ( 55.02542983044660474, -8.237060396196270062, 0.07017451552781985014 ) ) ;
#18700 = ORIENTED_EDGE ( 'NONE', *, *, #7055, .F. ) ;
#18701 = CARTESIAN_POINT ( 'NONE',  ( 7.249760686538667009, 3.748318449932293905, 7.906491560603678082 ) ) ;
#18702 = AXIS2_PLACEMENT_3D ( 'NONE', #31566, #16340, #16839 ) ;
#18703 = EDGE_CURVE ( 'NONE', #15236, #27172, #3356, .T. ) ;
#18704 = AXIS2_PLACEMENT_3D ( 'NONE', #13247, #23447, #5598 ) ;
#18705 = VERTEX_POINT ( 'NONE', #31423 ) ;
#18706 = APPROVAL_ROLE ( '' ) ;
#18707 = CARTESIAN_POINT ( 'NONE',  ( 18.75842578876440214, -5.877537581689508350, 3.995970707747694473 ) ) ;
#18708 = AXIS2_PLACEMENT_3D ( 'NONE', #4289, #19845, #4481 ) ;
#18709 = AXIS2_PLACEMENT_3D ( 'NONE', #16992, #21695, #32561 ) ;
#18710 = CARTESIAN_POINT ( 'NONE',  ( 17.19530788743130145, -15.12182558545884525, -1.000000000000000000 ) ) ;
#18711 = ORIENTED_EDGE ( 'NONE', *, *, #9397, .T. ) ;
#18712 = CARTESIAN_POINT ( 'NONE',  ( 5.834205823644816213, 18.00000000000000355, 2.241549108841682791 ) ) ;
#18713 = ORIENTED_EDGE ( 'NONE', *, *, #11285, .T. ) ;
#18714 = ORIENTED_EDGE ( 'NONE', *, *, #20269, .T. ) ;
#18715 = CARTESIAN_POINT ( 'NONE',  ( 107.4500373638804120, -17.36019379023677089, -4.522129901861164036 ) ) ;
#18716 = CARTESIAN_POINT ( 'NONE',  ( -4.312550801365593323, -3.675193018007245627, 1.088641768524163389 ) ) ;
#18717 = CARTESIAN_POINT ( 'NONE',  ( 7.249760686538667009, -4.007137495034861274, 6.940565734314584567 ) ) ;
#18718 = CARTESIAN_POINT ( 'NONE',  ( 0.6728940978343175283, -5.225733934469498188, -1.500000000000000000 ) ) ;
#18720 = ORIENTED_EDGE ( 'NONE', *, *, #24656, .F. ) ;
#18719 = CARTESIAN_POINT ( 'NONE',  ( 6.356382228872880624, 7.873648075250545553, -3.475951004017252988 ) ) ;
#18721 = CARTESIAN_POINT ( 'NONE',  ( -7.837550801365593678, 1.088641768524161613, 3.675193018007247403 ) ) ;
#18722 = CARTESIAN_POINT ( 'NONE',  ( 9.302055952181040865, 0.2457637073014105056, 1.050000000000000044 ) ) ;
#18723 = ADVANCED_BREP_SHAPE_REPRESENTATION ( '', ( #10233, #2865 ), #179 ) ;
#18724 = AXIS2_PLACEMENT_3D ( 'NONE', #2551, #12881, #15238 ) ;
#18725 = CARTESIAN_POINT ( 'NONE',  ( 6.530491482054472385, 2.114164693852704335, -8.398420403995354278 ) ) ;
#18726 = CARTESIAN_POINT ( 'NONE',  ( 22.17250000136559507, -2.363507492473152283, -1.913930629741525280 ) ) ;
#18727 = AXIS2_PLACEMENT_3D ( 'NONE', #21800, #4099, #9265 ) ;
#18729 = ORIENTED_EDGE ( 'NONE', *, *, #24945, .F. ) ;
#18728 = CARTESIAN_POINT ( 'NONE',  ( 2.437082427505617321, -4.432669656489553134, 9.703015696712942173 ) ) ;
#18730 = CIRCLE ( 'NONE', #19902, 5.100000000000000533 ) ;
#18731 = CIRCLE ( 'NONE', #26721, 4.000000000000000000 ) ;
#18732 = AXIS2_PLACEMENT_3D ( 'NONE', #28074, #32936, #30919 ) ;
#18733 = FACE_OUTER_BOUND ( 'NONE', #17054, .T. ) ;
#18734 = CARTESIAN_POINT ( 'NONE',  ( 20.79750000273119070, -2.594547506269383685, -0.7685399846772043020 ) ) ;
#18735 = EDGE_CURVE ( 'NONE', #17249, #17751, #25820, .T. ) ;
#18736 = CARTESIAN_POINT ( 'NONE',  ( 6.038144853276843804, -1.027626812407944179, -8.412419482080418121 ) ) ;
#18737 = CARTESIAN_POINT ( 'NONE',  ( 101.8147510725781473, -4.230945185443697909, -3.690576987646877249 ) ) ;
#18738 = CARTESIAN_POINT ( 'NONE',  ( 0.000000000000000000, 0.000000000000000000, 0.000000000000000000 ) ) ;
#18739 = AXIS2_PLACEMENT_3D ( 'NONE', #355, #30941, #22906 ) ;
#18740 = CARTESIAN_POINT ( 'NONE',  ( 2.857987896746962075, -2.305585824582580656, 9.278099925236432455 ) ) ;
#18741 = ADVANCED_FACE ( 'NONE', ( #26424 ), #31358, .F. ) ;
#18742 = FACE_OUTER_BOUND ( 'NONE', #23255, .T. ) ;
#18743 = CARTESIAN_POINT ( 'NONE',  ( -5.287550801365593856, -2.752080473201636845, 2.228590825266444586 ) ) ;
#18744 = EDGE_LOOP ( 'NONE', ( #3282, #22919, #9865, #13839 ) ) ;
#18745 = DIRECTION ( 'NONE',  ( 0.000000000000000000, 1.000000000000000000, 0.000000000000000000 ) ) ;
#18746 = ADVANCED_FACE ( 'NONE', ( #29394 ), #32079, .F. ) ;
#18747 = CIRCLE ( 'NONE', #11287, 4.000000000000001776 ) ;
#18748 = DIRECTION ( 'NONE',  ( -0.8660254037844409281, 0.4999999999999960587, 0.000000000000000000 ) ) ;
#18750 = CARTESIAN_POINT ( 'NONE',  ( 107.4495527293423578, -17.35289746557307211, 4.502194843723872353 ) ) ;
#18749 = LINE ( 'NONE', #24080, #13943 ) ;
#18751 = EDGE_CURVE ( 'NONE', #11524, #7301, #11924, .T. ) ;
#18752 = ORIENTED_EDGE ( 'NONE', *, *, #13686, .T. ) ;
#18753 = AXIS2_PLACEMENT_3D ( 'NONE', #4536, #12192, #22392 ) ;
#18754 = VECTOR ( 'NONE', #14163, 1000.000000000000000 ) ;
#18755 =( BOUNDED_CURVE ( )  B_SPLINE_CURVE ( 3, ( #22078, #14198, #6691, #1364 ),
 .UNSPECIFIED., .F., .F. ) 
 B_SPLINE_CURVE_WITH_KNOTS ( ( 4, 4 ),
 ( 4.712388980384689674, 6.283185307179586232 ),
 .UNSPECIFIED. ) 
 CURVE ( )  GEOMETRIC_REPRESENTATION_ITEM ( )  RATIONAL_B_SPLINE_CURVE ( ( 1.000000000000000000, 0.8047378541243649375, 0.8047378541243649375, 1.000000000000000000 ) ) 
 REPRESENTATION_ITEM ( '' )  );
#18756 = LINE ( 'NONE', #892, #2723 ) ;
#18757 = AXIS2_PLACEMENT_3D ( 'NONE', #1049, #3725, #19103 ) ;
#18758 = ORIENTED_EDGE ( 'NONE', *, *, #18765, .F. ) ;
#18759 = CARTESIAN_POINT ( 'NONE',  ( 21.33742408005867830, -21.80181733054034154, -1.346293739632234088 ) ) ;
#18761 = EDGE_LOOP ( 'NONE', ( #26394, #351, #11074, #24623 ) ) ;
#18760 = DIRECTION ( 'NONE',  ( 1.000000000000000000, 0.000000000000000000, 0.000000000000000000 ) ) ;
#18762 = ORIENTED_EDGE ( 'NONE', *, *, #3822, .F. ) ;
#18763 = CARTESIAN_POINT ( 'NONE',  ( 5.377543748152549874, -6.940565734314570356, -4.007137495034885255 ) ) ;
#18764 = AXIS2_PLACEMENT_3D ( 'NONE', #16758, #26616, #31475 ) ;
#18765 = EDGE_CURVE ( 'NONE', #20892, #29013, #14585, .T. ) ;
#18766 = VECTOR ( 'NONE', #9414, 1000.000000000000000 ) ;
#18768 = AXIS2_PLACEMENT_3D ( 'NONE', #5245, #12436, #15419 ) ;
#18767 = DIRECTION ( 'NONE',  ( -0.9975973382524639943, -0.06927878976713693071, 0.000000000000000000 ) ) ;
#18770 = VERTEX_POINT ( 'NONE', #16359 ) ;
#18769 = LINE ( 'NONE', #28973, #15503 ) ;
#18771 = CARTESIAN_POINT ( 'NONE',  ( 9.924500721667349978, 1.154815372884564928, -1.500000000000000000 ) ) ;
#18772 = CARTESIAN_POINT ( 'NONE',  ( 0.9575256569274729346, -15.55590288271891630, -1.746220241394478290 ) ) ;
#18773 = FACE_OUTER_BOUND ( 'NONE', #32005, .T. ) ;
#18774 = CARTESIAN_POINT ( 'NONE',  ( 8.103242287716716064, -10.98376420866757464, -1.500000000000000000 ) ) ;
#18775 = CARTESIAN_POINT ( 'NONE',  ( 107.9731642803859444, -17.68293443006343324, -4.116431948592269130 ) ) ;
#18776 = CARTESIAN_POINT ( 'NONE',  ( -1.152183934781129714E-14, 21.49000000000002331, -1.500000000000000000 ) ) ;
#18777 = EDGE_CURVE ( 'NONE', #25199, #22329, #25549, .T. ) ;
#18778 = DIRECTION ( 'NONE',  ( 0.000000000000000000, -0.08715574274766814400, 0.9961946980917446570 ) ) ;
#18779 = CARTESIAN_POINT ( 'NONE',  ( 23.68974245684579927, -6.697273116530260140, 3.390608483628176018 ) ) ;
#18780 = AXIS2_PLACEMENT_3D ( 'NONE', #13813, #21701, #3515 ) ;
#18781 = VECTOR ( 'NONE', #16580, 1000.000000000000000 ) ;
#18782 = CARTESIAN_POINT ( 'NONE',  ( -2.957304906975409597, -1.062355717592093463, -3.000000000000000888 ) ) ;
#18783 = DIRECTION ( 'NONE',  ( -1.000000000000000000, 0.000000000000000000, 0.000000000000000000 ) ) ;
#18784 = ORIENTED_EDGE ( 'NONE', *, *, #29281, .T. ) ;
#18785 = CARTESIAN_POINT ( 'NONE',  ( -6.112942406915326643, -3.366872799099910998E-15, -3.000000000000000000 ) ) ;
#18786 = CIRCLE ( 'NONE', #17183, 0.4999999999999995559 ) ;
#18787 = AXIS2_PLACEMENT_3D ( 'NONE', #7492, #2661, #336 ) ;
#18788 = DIRECTION ( 'NONE',  ( -0.4999999999999978906, -0.8660254037844399289, 0.000000000000000000 ) ) ;
#18789 = EDGE_CURVE ( 'NONE', #389, #9926, #27054, .T. ) ;
#18790 = CARTESIAN_POINT ( 'NONE',  ( -31.69232733568932403, -28.43932300454937590, -1.595404497688272638 ) ) ;
#18791 = ORIENTED_EDGE ( 'NONE', *, *, #20734, .T. ) ;
#18792 = VECTOR ( 'NONE', #25315, 1000.000000000000000 ) ;
#18793 = AXIS2_PLACEMENT_3D ( 'NONE', #13170, #28570, #5663 ) ;
#18794 = DIRECTION ( 'NONE',  ( 0.000000000000000000, 0.000000000000000000, 1.000000000000000000 ) ) ;
#18795 = ADVANCED_FACE ( 'NONE', ( #14175 ), #19044, .F. ) ;
#18796 = CARTESIAN_POINT ( 'NONE',  ( 2.661997781067683366, 9.315861390595088665, 3.981025027156513296 ) ) ;
#18797 = EDGE_LOOP ( 'NONE', ( #16971, #7765, #27494, #24419 ) ) ;
#18798 = CARTESIAN_POINT ( 'NONE',  ( 0.5291759363107053638, -6.520544204277276101, -1.500000000000001110 ) ) ;
#18799 =( LENGTH_UNIT ( ) NAMED_UNIT ( * ) SI_UNIT ( .MILLI., .METRE. ) );
#18800 = ADVANCED_FACE ( 'NONE', ( #4159 ), #14325, .T. ) ;
#18801 = EDGE_LOOP ( 'NONE', ( #26079, #14960, #1716, #20516 ) ) ;
#18803 = VERTEX_POINT ( 'NONE', #31587 ) ;
#18802 = B_SPLINE_CURVE_WITH_KNOTS ( 'NONE', 3,
 ( #232, #7551, #12725, #15897, #30821, #5222 ),
 .UNSPECIFIED., .F., .F.,
 ( 4, 2, 4 ),
 ( 2.333100327427146720E-07, 0.0008600466339166887254, 0.001719859957800634609 ),
 .UNSPECIFIED. ) ;
#18804 = CARTESIAN_POINT ( 'NONE',  ( 25.48003136492769372, -17.55790038815476350, -1.043845799725529710 ) ) ;
#18805 = B_SPLINE_SURFACE_WITH_KNOTS ( 'NONE', 1, 3, ( 
 ( #15646, #22988, #23331, #22688, #107, #23182, #25857, #291, #20022, #5451, #30214, #10464, #28029, #2975, #17828, #435 ),
 ( #2613, #20514, #5126, #25506, #20329, #30727, #7799, #27677, #20675, #12476, #17636, #30877, #13129, #7948, #28337, #7287 ),
 ( #32891, #9957, #27842, #20998, #31360, #21305, #5628, #8773, #16119, #18978, #15806, #23818, #5925, #26168, #21162, #930 ) ),
 .UNSPECIFIED., .F., .F., .F.,
 ( 2, 1, 2 ),
 ( 4, 2, 2, 2, 2, 2, 2, 4 ),
 ( 0.000000000000000000, 1.000000000000000000, 1.172438907772619610 ),
 ( 0.000000000000000000, 0.5000000000000000000, 0.6250000000000000000, 0.7500000000000000000, 0.8125000000000000000, 0.8750000000000000000, 0.9375000000000000000, 1.000000000000000000 ),
 .UNSPECIFIED. ) ;
#18806 = CALENDAR_DATE ( 2026, 6, 10 ) ;
#18807 = AXIS2_PLACEMENT_3D ( 'NONE', #9058, #16277, #916 ) ;
#18809 = VERTEX_POINT ( 'NONE', #3833 ) ;
#18808 = CARTESIAN_POINT ( 'NONE',  ( 7.577572045913244736, 15.00000000000000178, 4.629213727441584325 ) ) ;
#18810 = ORIENTED_EDGE ( 'NONE', *, *, #7423, .T. ) ;
#18811 = DIRECTION ( 'NONE',  ( -8.541412920197209954E-17, -0.9961946980917446570, -0.08715574274766894891 ) ) ;
#18812 = AXIS2_PLACEMENT_3D ( 'NONE', #6471, #24513, #1639 ) ;
#18813 = VECTOR ( 'NONE', #1244, 1000.000000000000000 ) ;
#18814 = AXIS2_PLACEMENT_3D ( 'NONE', #8141, #18837, #951 ) ;
#18815 = ORIENTED_EDGE ( 'NONE', *, *, #32948, .T. ) ;
#18816 = CARTESIAN_POINT ( 'NONE',  ( 5.377543748152548986, -7.530955069117495349, -2.741043480755002371 ) ) ;
#18818 = ORIENTED_EDGE ( 'NONE', *, *, #30261, .F. ) ;
#18817 = CARTESIAN_POINT ( 'NONE',  ( 84.87411226253082930, -2.587501188392339113, -1.529339190611058052 ) ) ;
#18819 = AXIS2_PLACEMENT_3D ( 'NONE', #13325, #23537, #24204 ) ;
#18820 = CARTESIAN_POINT ( 'NONE',  ( 0.7632845268429988561, 7.360373001717848140, -4.729683950891435451 ) ) ;
#18821 = CARTESIAN_POINT ( 'NONE',  ( 12.44989959798878232, 0.4999999999999998890, 2.482234843104758060 ) ) ;
#18822 = AXIS2_PLACEMENT_3D ( 'NONE', #23868, #975, #3653 ) ;
#18823 = VECTOR ( 'NONE', #21076, 1000.000000000000000 ) ;
#18824 = CYLINDRICAL_SURFACE ( 'NONE', #31515, 5.000000000000002665 ) ;
#18825 = LINE ( 'NONE', #14271, #27953 ) ;
#18826 = CARTESIAN_POINT ( 'NONE',  ( 7.249760686538667009, 8.014274990069656823, -8.669741416787380218E-17 ) ) ;
#18827 = EDGE_CURVE ( 'NONE', #17238, #28583, #9333, .T. ) ;
#18828 = CC_DESIGN_PERSON_AND_ORGANIZATION_ASSIGNMENT ( #14688, #3840, ( #1036 ) ) ;
#18829 = DIRECTION ( 'NONE',  ( -1.000000000000000000, 0.000000000000000000, 0.000000000000000000 ) ) ;
#18830 = CARTESIAN_POINT ( 'NONE',  ( 17.36028307726380504, -18.11957666779667875, -4.522129901861164925 ) ) ;
#18831 = DIRECTION ( 'NONE',  ( 0.000000000000000000, 1.000000000000000000, 0.000000000000000000 ) ) ;
#18832 = CARTESIAN_POINT ( 'NONE',  ( 0.000000000000000000, -6.700937042937042065, -2.183447440113257976 ) ) ;
#18833 = DIRECTION ( 'NONE',  ( -1.000000000000000000, 8.574039729943018344E-17, -0.000000000000000000 ) ) ;
#18834 = VECTOR ( 'NONE', #15233, 1000.000000000000000 ) ;
#18835 = DIRECTION ( 'NONE',  ( 0.000000000000000000, 0.000000000000000000, 1.000000000000000000 ) ) ;
#18836 = CARTESIAN_POINT ( 'NONE',  ( 2.326102263860147179, 9.559024163330285262, 5.234081561440546260 ) ) ;
#18837 = DIRECTION ( 'NONE',  ( -1.000000000000000000, 0.000000000000000000, 0.000000000000000000 ) ) ;
#18838 = VECTOR ( 'NONE', #10722, 1000.000000000000114 ) ;
#18839 = CARTESIAN_POINT ( 'NONE',  ( 10.56870887191539587, 1.946309384392590047, 4.616489984850538519 ) ) ;
#18840 = CARTESIAN_POINT ( 'NONE',  ( -4.362550801365593145, -2.752080473201636845, 2.228590825266444586 ) ) ;
#18841 = ORIENTED_EDGE ( 'NONE', *, *, #6048, .T. ) ;
#18842 = EDGE_CURVE ( 'NONE', #30055, #8068, #8674, .T. ) ;
#18843 = AXIS2_PLACEMENT_3D ( 'NONE', #7069, #29975, #2407 ) ;
#18844 = AXIS2_PLACEMENT_3D ( 'NONE', #22486, #32701, #9782 ) ;
#18845 = CARTESIAN_POINT ( 'NONE',  ( -6.400050800000000706, -2.331437884370912705, 1.887961173149512062 ) ) ;
#18846 = CIRCLE ( 'NONE', #4442, 8.500000000000000000 ) ;
#18847 = DIRECTION ( 'NONE',  ( -1.000000000000000000, 8.574039729943017111E-17, -0.000000000000000000 ) ) ;
#18848 = LINE ( 'NONE', #31389, #10861 ) ;
#18849 = CARTESIAN_POINT ( 'NONE',  ( 7.278212736155783347, -5.482579125108129503, 1.499999999999858113 ) ) ;
#18850 = AXIS2_PLACEMENT_3D ( 'NONE', #23516, #23698, #31065 ) ;
#18851 = VERTEX_POINT ( 'NONE', #3668 ) ;
#18852 = AXIS2_PLACEMENT_3D ( 'NONE', #3015, #31079, #23370 ) ;
#18853 = ORIENTED_EDGE ( 'NONE', *, *, #7960, .T. ) ;
#18854 = CARTESIAN_POINT ( 'NONE',  ( 4.832184221226294873, -12.72809002048187388, 1.499999999999788391 ) ) ;
#18855 = CALENDAR_DATE ( 2026, 6, 10 ) ;
#18856 = CARTESIAN_POINT ( 'NONE',  ( 18.78723038048892846, -5.555560056377619738, 4.275175838841520637 ) ) ;
#18857 = CARTESIAN_POINT ( 'NONE',  ( 108.1156589233279419, 18.82219444680297116, 4.414476567109417715 ) ) ;
#18858 = VECTOR ( 'NONE', #1814, 1000.000000000000000 ) ;
#18859 = CARTESIAN_POINT ( 'NONE',  ( 25.75999999999999801, -2.208672634433321348E-15, 0.000000000000000000 ) ) ;
#18860 = DIRECTION ( 'NONE',  ( 0.000000000000000000, 0.000000000000000000, 1.000000000000000000 ) ) ;
#18861 = AXIS2_PLACEMENT_3D ( 'NONE', #31108, #24031, #1157 ) ;
#18862 = ORIENTED_EDGE ( 'NONE', *, *, #25697, .T. ) ;
#18863 = AXIS2_PLACEMENT_3D ( 'NONE', #16931, #11587, #19115 ) ;
#18864 = CARTESIAN_POINT ( 'NONE',  ( 1.624999999999999778, 10.82112760146739383, -1.975651141462126947 ) ) ;
#18865 = ADVANCED_FACE ( 'NONE', ( #12512 ), #2341, .T. ) ;
#18866 = CARTESIAN_POINT ( 'NONE',  ( -47.64323377349501243, 16.45499999999998408, -1.050000000000000044 ) ) ;
#18867 = AXIS2_PLACEMENT_3D ( 'NONE', #4656, #15182, #30248 ) ;
#18868 = LINE ( 'NONE', #16339, #6039 ) ;
#18869 = VECTOR ( 'NONE', #31953, 1000.000000000000000 ) ;
#18871 = VERTEX_POINT ( 'NONE', #17186 ) ;
#18870 = DIRECTION ( 'NONE',  ( 0.000000000000000000, -1.000000000000000000, 0.000000000000000000 ) ) ;
#18872 = CARTESIAN_POINT ( 'NONE',  ( -3.712550801365592790, 1.088641768524161613, 3.675193018007247403 ) ) ;
#18873 = CARTESIAN_POINT ( 'NONE',  ( 0.000000000000000000, 0.000000000000000000, 0.000000000000000000 ) ) ;
#18874 = CARTESIAN_POINT ( 'NONE',  ( 10.00000000000000178, -8.574039729943018837E-16, 0.000000000000000000 ) ) ;
#18875 = APPROVAL_PERSON_ORGANIZATION ( #20587, #29060, #27750 ) ;
#18876 = EDGE_LOOP ( 'NONE', ( #22326, #22296, #14767, #13646 ) ) ;
#18877 = DIRECTION ( 'NONE',  ( 0.000000000000000000, 0.000000000000000000, -1.000000000000000000 ) ) ;
#18878 = CARTESIAN_POINT ( 'NONE',  ( -23.54713438637982748, 18.90773822806172433, 1.500000000000000000 ) ) ;
#18879 = DIRECTION ( 'NONE',  ( 0.000000000000000000, 0.08715574274764703588, 0.9961946980917465444 ) ) ;
#18880 = DIRECTION ( 'NONE',  ( -1.000000000000000000, 0.000000000000000000, 0.000000000000000000 ) ) ;
#18881 = B_SPLINE_CURVE_WITH_KNOTS ( 'NONE', 3,
 ( #523, #6693, #26929, #4032, #32448, #6344, #9010, #24555, #27425, #4532, #1677, #4179 ),
 .UNSPECIFIED., .F., .F.,
 ( 4, 2, 2, 2, 2, 4 ),
 ( 0.000000000000000000, 0.0007208007047092903361, 0.001081201057063939461, 0.001261401233241265379, 0.001351501321329926387, 0.001441601409418587394 ),
 .UNSPECIFIED. ) ;
#18882 = EDGE_CURVE ( 'NONE', #24347, #8396, #20480, .T. ) ;
#18883 = CARTESIAN_POINT ( 'NONE',  ( 0.000000000000000000, 0.000000000000000000, 0.000000000000000000 ) ) ;
#18884 = ORIENTED_EDGE ( 'NONE', *, *, #15175, .T. ) ;
#18885 = ADVANCED_FACE ( 'NONE', ( #12324 ), #15667, .T. ) ;
#18886 = CARTESIAN_POINT ( 'NONE',  ( 7.064423637758999952, 2.318425219013722227, -8.437262856155470558 ) ) ;
#18887 = AXIS2_PLACEMENT_3D ( 'NONE', #8932, #23829, #24323 ) ;
#18888 = CARTESIAN_POINT ( 'NONE',  ( -57.64077562173743985, -3.382820725347776225, 5.845255965757654160 ) ) ;
#18889 = EDGE_CURVE ( 'NONE', #6370, #6440, #4012, .T. ) ;
#18890 = CARTESIAN_POINT ( 'NONE',  ( -4.187550801365593323, 0.3701630799359330593, -3.521866450007987037 ) ) ;
#18891 = CARTESIAN_POINT ( 'NONE',  ( 3.093679806470315263, -0.1913619822784921320, -1.398088436977038773 ) ) ;
#18892 = DIRECTION ( 'NONE',  ( 0.000000000000000000, 0.000000000000000000, 1.000000000000000000 ) ) ;
#18893 = ORIENTED_EDGE ( 'NONE', *, *, #29807, .T. ) ;
#18894 = CARTESIAN_POINT ( 'NONE',  ( 7.249760686538667009, -2.318425219014288885, 8.437262856154156054 ) ) ;
#18895 = CIRCLE ( 'NONE', #22645, 5.000000000000000888 ) ;
#18896 = ORIENTED_EDGE ( 'NONE', *, *, #27526, .T. ) ;
#18897 = CIRCLE ( 'NONE', #14050, 10.94895958125474245 ) ;
#18898 = APPLICATION_PROTOCOL_DEFINITION ( 'international standard', 'config_control_design', 1994, #25714 ) ;
#18900 = DIRECTION ( 'NONE',  ( 0.9563911903463302444, 0.000000000000000000, 0.2920888409849467515 ) ) ;
#18899 = LOCAL_TIME ( 16, 7, 10.00000000000000000, #30253 ) ;
#18901 = DIRECTION ( 'NONE',  ( 8.574039729943018344E-17, 1.000000000000000000, 0.000000000000000000 ) ) ;
#18902 = ORIENTED_EDGE ( 'NONE', *, *, #28371, .T. ) ;
#18903 = CARTESIAN_POINT ( 'NONE',  ( -2.775296318097017156, 4.123808329995814975E-33, -1.260187769642231226 ) ) ;
#18904 = ORIENTED_EDGE ( 'NONE', *, *, #22303, .T. ) ;
#18905 = ORIENTED_EDGE ( 'NONE', *, *, #25914, .F. ) ;
#18906 = CARTESIAN_POINT ( 'NONE',  ( 0.000000000000000000, 6.478011392632891052, 6.807171995660606711 ) ) ;
#18907 = CARTESIAN_POINT ( 'NONE',  ( -2.962550801365593234, 2.228590825266444142, 2.752080473201636845 ) ) ;
#18908 = DIRECTION ( 'NONE',  ( -1.000000000000000000, -0.000000000000000000, 0.000000000000000000 ) ) ;
#18909 = CARTESIAN_POINT ( 'NONE',  ( 9.999999999999998224, -4.681538312723512618, -0.8254815157535732029 ) ) ;
#18911 = ORIENTED_EDGE ( 'NONE', *, *, #2603, .F. ) ;
#18910 = CARTESIAN_POINT ( 'NONE',  ( 18.74139243898558149, 14.92200307055332509, -1.499999999999999556 ) ) ;
#18912 = VECTOR ( 'NONE', #21698, 1000.000000000000000 ) ;
#18913 = CIRCLE ( 'NONE', #29054, 10.64228691119593151 ) ;
#18914 = CARTESIAN_POINT ( 'NONE',  ( -7.337550801365593678, 1.828967928396027176, -3.368539882008727115 ) ) ;
#18915 = FACE_OUTER_BOUND ( 'NONE', #11944, .T. ) ;
#18916 = FACE_OUTER_BOUND ( 'NONE', #486, .T. ) ;
#18917 = CARTESIAN_POINT ( 'NONE',  ( 21.92250000136559507, -1.913930629741527500, 2.363507492473149618 ) ) ;
#18919 = ORIENTED_EDGE ( 'NONE', *, *, #7544, .F. ) ;
#18918 = FACE_OUTER_BOUND ( 'NONE', #12353, .T. ) ;
#18920 = EDGE_CURVE ( 'NONE', #17843, #536, #22544, .T. ) ;
#18921 = CARTESIAN_POINT ( 'NONE',  ( -59.37247738224319704, -6.026451378431820771, 5.500000000000000000 ) ) ;
#18922 = CARTESIAN_POINT ( 'NONE',  ( 0.000000000000000000, 0.000000000000000000, 0.000000000000000000 ) ) ;
#18923 = CC_DESIGN_APPROVAL ( #17997, ( #8747 ) ) ;
#18924 = EDGE_CURVE ( 'NONE', #2818, #14512, #12020, .T. ) ;
#18925 = CARTESIAN_POINT ( 'NONE',  ( 0.000000000000000000, 5.904264776415128146, -2.046865518294647579 ) ) ;
#18926 = EDGE_CURVE ( 'NONE', #9926, #2614, #8710, .T. ) ;
#18927 = CARTESIAN_POINT ( 'NONE',  ( 101.8212854292504090, -4.325038295980876413, -3.539148343398925700 ) ) ;
#18928 = CARTESIAN_POINT ( 'NONE',  ( -4.037226184167227672, -8.274238725605433942, -1.744146341608699746 ) ) ;
#18929 = CARTESIAN_POINT ( 'NONE',  ( 0.000000000000000000, -7.533794289457995674, -7.944914065997195074 ) ) ;
#18930 = CARTESIAN_POINT ( 'NONE',  ( 3.499999999999999556, 5.904264776415098837, 2.046865518294726183 ) ) ;
#18931 = CARTESIAN_POINT ( 'NONE',  ( -2.587550801365593678, 0.3701630799359330593, -3.521866450007987037 ) ) ;
#18932 = ORIENTED_EDGE ( 'NONE', *, *, #526, .T. ) ;
#18933 = AXIS2_PLACEMENT_3D ( 'NONE', #32908, #14975, #4981 ) ;
#18934 = CARTESIAN_POINT ( 'NONE',  ( 1.750000000000000222, 4.438567988583082879, 7.249076783337693008 ) ) ;
#18935 = LINE ( 'NONE', #21752, #13525 ) ;
#18937 = CARTESIAN_POINT ( 'NONE',  ( 107.9477478514680371, -17.31694417646615136, 4.497024978861354327 ) ) ;
#18936 = CARTESIAN_POINT ( 'NONE',  ( 1.750000000000000222, -2.834406817834963732, 8.013497238472769624 ) ) ;
#18938 = ORIENTED_EDGE ( 'NONE', *, *, #29059, .F. ) ;
#18939 = DIRECTION ( 'NONE',  ( -1.000000000000000000, 0.000000000000000000, 0.000000000000000000 ) ) ;
#18940 = ORIENTED_EDGE ( 'NONE', *, *, #9536, .F. ) ;
#18941 = CARTESIAN_POINT ( 'NONE',  ( 0.000000000000000000, 0.000000000000000000, -1.500000000000000000 ) ) ;
#18943 = VERTEX_POINT ( 'NONE', #27884 ) ;
#18942 = LINE ( 'NONE', #13098, #32032 ) ;
#18944 = ORIENTED_EDGE ( 'NONE', *, *, #19732, .F. ) ;
#18945 = CARTESIAN_POINT ( 'NONE',  ( 40.73236281613284149, -5.747100024560975129, 3.993433057584553580 ) ) ;
#18946 = CARTESIAN_POINT ( 'NONE',  ( 72.25703127509153489, -22.87839253411022611, -1.499999999999999556 ) ) ;
#18948 = EDGE_LOOP ( 'NONE', ( #13908, #12381, #4753, #13230 ) ) ;
#18947 = CARTESIAN_POINT ( 'NONE',  ( 8.911384905465473238, 0.2172754300402719996, 1.412391582771868492 ) ) ;
#18949 = LINE ( 'NONE', #29465, #28438 ) ;
#18950 = DIRECTION ( 'NONE',  ( 1.000000000000000000, -8.574039729943018344E-17, -0.000000000000000000 ) ) ;
#18951 = EDGE_CURVE ( 'NONE', #10585, #25735, #27705, .T. ) ;
#18952 = CARTESIAN_POINT ( 'NONE',  ( 108.1288400433390393, -19.92462668933126579, -1.384270303710054328 ) ) ;
#18953 = CARTESIAN_POINT ( 'NONE',  ( 10.63777811968158993, -12.44241537618683147, -1.500000000000426104 ) ) ;
#18954 = CARTESIAN_POINT ( 'NONE',  ( 0.000000000000000000, -1.179494851233943598, 6.136676046192483192 ) ) ;
#18955 = CARTESIAN_POINT ( 'NONE',  ( -4.962942409646514008, 3.284080845023683730E-15, 3.000000000000000000 ) ) ;
#18956 = ADVANCED_FACE ( 'NONE', ( #32761 ), #2493, .T. ) ;
#18957 = AXIS2_PLACEMENT_3D ( 'NONE', #11879, #1871, #25057 ) ;
#18958 = DIRECTION ( 'NONE',  ( 1.000000000000000000, -0.000000000000000000, 0.000000000000000000 ) ) ;
#18959 = DIRECTION ( 'NONE',  ( 1.000000000000000000, -8.574039729943018344E-17, -0.000000000000000000 ) ) ;
#18960 = EDGE_CURVE ( 'NONE', #4750, #17249, #9838, .T. ) ;
#18961 = CARTESIAN_POINT ( 'NONE',  ( 6.880159540721329847, 8.414807581959459881, 2.328896285337215488 ) ) ;
#18962 = DIRECTION ( 'NONE',  ( -4.917867153433037856E-17, -0.5735764363510502672, 0.8191520442889889120 ) ) ;
#18963 = ORIENTED_EDGE ( 'NONE', *, *, #10994, .F. ) ;
#18964 = CARTESIAN_POINT ( 'NONE',  ( -6.400050800000000706, -2.331437884370912705, 1.887961173149512062 ) ) ;
#18965 = ADVANCED_FACE ( 'NONE', ( #4508 ), #29900, .T. ) ;
#18966 = DIRECTION ( 'NONE',  ( 1.000000000000000000, 0.000000000000000000, 0.000000000000000000 ) ) ;
#18967 = DIRECTION ( 'NONE',  ( 1.000000000000000000, -0.000000000000000000, -0.000000000000000000 ) ) ;
#18968 = ORIENTED_EDGE ( 'NONE', *, *, #24798, .T. ) ;
#18969 = CARTESIAN_POINT ( 'NONE',  ( -2.556376981307135754, -0.1572233378491262878, 2.999999999999999556 ) ) ;
#18970 = CARTESIAN_POINT ( 'NONE',  ( 0.000000000000000000, 4.472189673936786569, 8.264486777890123648 ) ) ;
#18971 = ORIENTED_EDGE ( 'NONE', *, *, #27021, .F. ) ;
#18972 = CARTESIAN_POINT ( 'NONE',  ( 12.21818417105343713, -15.17047698692286239, -1.499999999999999112 ) ) ;
#18973 = DIRECTION ( 'NONE',  ( 7.838856478428783661E-17, -8.063469270749811750E-19, 1.000000000000000000 ) ) ;
#18974 = ORIENTED_EDGE ( 'NONE', *, *, #21438, .T. ) ;
#18975 = EDGE_CURVE ( 'NONE', #685, #10104, #14764, .T. ) ;
#18976 = ORIENTED_EDGE ( 'NONE', *, *, #19958, .F. ) ;
#18977 = CARTESIAN_POINT ( 'NONE',  ( 25.24493059864625977, -17.53551310887482373, -1.328338028042538976 ) ) ;
#18979 = VERTEX_POINT ( 'NONE', #22865 ) ;
#18978 = CARTESIAN_POINT ( 'NONE',  ( -3.142639414282944799, -12.00291247001954531, -0.9788672205760856615 ) ) ;
#18980 = ORIENTED_EDGE ( 'NONE', *, *, #15093, .T. ) ;
#18981 = CARTESIAN_POINT ( 'NONE',  ( 25.42250000136559507, 1.913930629741522838, -2.363507492473150062 ) ) ;
#18982 = ADVANCED_FACE ( 'NONE', ( #28062 ), #30089, .T. ) ;
#18983 = VERTEX_POINT ( 'NONE', #9485 ) ;
#18984 = CARTESIAN_POINT ( 'NONE',  ( -2.786590204610738475, -5.640011313470055576, 4.522129901861158707 ) ) ;
#18985 = CARTESIAN_POINT ( 'NONE',  ( 7.249760686538667009, -7.953573330858190182, -3.647351267791651974 ) ) ;
#18987 = ORIENTED_EDGE ( 'NONE', *, *, #19034, .T. ) ;
#18986 = LINE ( 'NONE', #16298, #8017 ) ;
#18988 = DIRECTION ( 'NONE',  ( -1.000000000000000000, 0.000000000000000000, 0.000000000000000000 ) ) ;
#18989 = CARTESIAN_POINT ( 'NONE',  ( 6.883866357751289300, -0.6899766464188280546, 8.704251636488461230 ) ) ;
#18990 = CARTESIAN_POINT ( 'NONE',  ( -56.72341663440466419, 0.2675318231349337328, 1.614498169334199984 ) ) ;
#18991 = PLANE ( 'NONE',  #2334 ) ;
#18992 = CARTESIAN_POINT ( 'NONE',  ( 108.0613718287933978, -18.95310118385105369, 4.512205001694104212 ) ) ;
#18993 =( BOUNDED_CURVE ( )  B_SPLINE_CURVE ( 3, ( #14309, #32253, #27376, #21846 ),
 .UNSPECIFIED., .F., .F. ) 
 B_SPLINE_CURVE_WITH_KNOTS ( ( 4, 4 ),
 ( 4.712388980384689674, 6.091199089460276106 ),
 .UNSPECIFIED. ) 
 CURVE ( )  GEOMETRIC_REPRESENTATION_ITEM ( )  RATIONAL_B_SPLINE_CURVE ( ( 1.000000000000000000, 0.8477497222584658987, 0.8477497222584658987, 1.000000000000000000 ) ) 
 REPRESENTATION_ITEM ( '' )  );
#18994 = DIRECTION ( 'NONE',  ( -1.000000000000000000, 0.000000000000000000, -8.673617379884027583E-16 ) ) ;
#18995 = CARTESIAN_POINT ( 'NONE',  ( 69.15470699321888048, -7.794592769514103736, -0.8105619180604369811 ) ) ;
#18996 = CARTESIAN_POINT ( 'NONE',  ( 14.23800746264082839, 22.11259878822726321, 1.508259000770582059 ) ) ;
#18997 = ADVANCED_FACE ( 'NONE', ( #19876 ), #32579, .F. ) ;
#18998 = ADVANCED_FACE ( 'NONE', ( #27397 ), #25412, .T. ) ;
#18999 = CARTESIAN_POINT ( 'NONE',  ( 110.2535626002996310, 19.41193660949215882, -0.4463807625373771293 ) ) ;
#19000 = DIRECTION ( 'NONE',  ( 1.000000000000000000, -0.000000000000000000, -0.000000000000000000 ) ) ;
#19001 = DIRECTION ( 'NONE',  ( 1.000000000000000000, 0.000000000000000000, -0.000000000000000000 ) ) ;
#19002 = CARTESIAN_POINT ( 'NONE',  ( 5.377543748152549874, 4.007137495034909236, -6.940565734314555257 ) ) ;
#19003 = DIRECTION ( 'NONE',  ( 0.000000000000000000, 0.000000000000000000, 1.000000000000000000 ) ) ;
#19004 = ADVANCED_FACE ( 'NONE', ( #29196 ), #6284, .F. ) ;
#19005 = CARTESIAN_POINT ( 'NONE',  ( -7.750050802731187183, 0.3135853898029611342, -2.983565686104819648 ) ) ;
#19006 = ORIENTED_EDGE ( 'NONE', *, *, #28804, .T. ) ;
#19007 = CARTESIAN_POINT ( 'NONE',  ( -7.900050800000000706, -2.983565686104819648, -0.3135853898029605791 ) ) ;
#19008 = CARTESIAN_POINT ( 'NONE',  ( 107.4500593345382811, -17.36019228850094720, 4.522129901861156931 ) ) ;
#19009 = CARTESIAN_POINT ( 'NONE',  ( 3.249999999999999556, 0.000000000000000000, 0.000000000000000000 ) ) ;
#19010 = CARTESIAN_POINT ( 'NONE',  ( 8.254683653268195087, -1.057518490445428672, 1.500000000000000000 ) ) ;
#19011 = ORIENTED_EDGE ( 'NONE', *, *, #4072, .T. ) ;
#19012 = CARTESIAN_POINT ( 'NONE',  ( 6.840024017557566616, -8.509480309817710975, -1.500000000000000222 ) ) ;
#19013 = EDGE_CURVE ( 'NONE', #28345, #15521, #27927, .T. ) ;
#19014 = B_SPLINE_CURVE_WITH_KNOTS ( 'NONE', 3,
 ( #28134, #12907, #25461, #17284, #2570, #7754, #27636, #12587, #10068, #12736 ),
 .UNSPECIFIED., .F., .F.,
 ( 4, 2, 2, 2, 4 ),
 ( 1.968338519013029732E-07, 0.0005467926395225671107, 0.001093388445193233232, 0.001639984250863899245, 0.002186580056534565691 ),
 .UNSPECIFIED. ) ;
#19015 = CC_DESIGN_DATE_AND_TIME_ASSIGNMENT ( #2108, #4779, ( #26402 ) ) ;
#19016 = ORIENTED_EDGE ( 'NONE', *, *, #2861, .F. ) ;
#19017 = CARTESIAN_POINT ( 'NONE',  ( 0.5876463044851316653, -8.554742072817132836, 1.500000000000176303 ) ) ;
#19018 = APPROVAL_STATUS ( 'not_yet_approved' ) ;
#19019 = CARTESIAN_POINT ( 'NONE',  ( 28.67557137524189770, -6.315853537245688543, 4.312042181580753031 ) ) ;
#19020 = CARTESIAN_POINT ( 'NONE',  ( 26.08945412691624099, 19.05746434167065928, -1.050000000000000044 ) ) ;
#19021 = CARTESIAN_POINT ( 'NONE',  ( 69.01977195939538490, -5.101425094635309243, -4.150066331406297770 ) ) ;
#19022 = FACE_OUTER_BOUND ( 'NONE', #28228, .T. ) ;
#19023 = CARTESIAN_POINT ( 'NONE',  ( -5.362942409646513475, -3.366872799099910998E-15, -3.000000000000000000 ) ) ;
#19024 = EDGE_LOOP ( 'NONE', ( #15018, #28637, #14404, #11553 ) ) ;
#19025 = DIRECTION ( 'NONE',  ( -1.000000000000000000, 0.000000000000000000, -0.000000000000000000 ) ) ;
#19026 = CARTESIAN_POINT ( 'NONE',  ( -60.07995281065674931, -10.96999999999998465, 8.549999999999998934 ) ) ;
#19027 = DIRECTION ( 'NONE',  ( -1.000000000000000000, 0.000000000000000000, 0.000000000000000000 ) ) ;
#19029 = ORIENTED_EDGE ( 'NONE', *, *, #18402, .T. ) ;
#19028 = CARTESIAN_POINT ( 'NONE',  ( -23.35000000000000142, -10.96966150227469505, -11.00000000000000000 ) ) ;
#19030 = CARTESIAN_POINT ( 'NONE',  ( -4.412550801365593856, -1.828967928396026510, 3.368539882008728004 ) ) ;
#19031 = CARTESIAN_POINT ( 'NONE',  ( -40.71733131760397129, -12.43974741078717372, 5.871858320049880398 ) ) ;
#19032 = DIRECTION ( 'NONE',  ( 0.000000000000000000, 0.7071067811865465735, -0.7071067811865484609 ) ) ;
#19033 = CARTESIAN_POINT ( 'NONE',  ( 0.1606232843943592725, 10.56438947504861936, 1.177222770082250847 ) ) ;
#19034 = EDGE_CURVE ( 'NONE', #11008, #15051, #19507, .T. ) ;
#19035 = FACE_OUTER_BOUND ( 'NONE', #27952, .T. ) ;
#19036 = DIRECTION ( 'NONE',  ( 1.000000000000000000, 0.000000000000000000, 0.000000000000000000 ) ) ;
#19037 = CARTESIAN_POINT ( 'NONE',  ( 109.7220438555052056, -17.55815402607574782, 5.485967528433933538 ) ) ;
#19038 = DIRECTION ( 'NONE',  ( 1.000000000000000000, -8.574039729943018344E-17, -0.000000000000000000 ) ) ;
#19039 = ORIENTED_EDGE ( 'NONE', *, *, #25482, .F. ) ;
#19040 = CARTESIAN_POINT ( 'NONE',  ( 25.82046699000660439, 24.17190842697640818, -2.806473568333519353 ) ) ;
#19041 = CARTESIAN_POINT ( 'NONE',  ( -2.039411552024039231, 1.053646271254045308, 3.241837583267886291 ) ) ;
#19042 = CARTESIAN_POINT ( 'NONE',  ( -4.387550801365594388, -3.521866450007987037, -0.3701630799359323931 ) ) ;
#19043 = CARTESIAN_POINT ( 'NONE',  ( 3.286352104298968069, -0.1045966074583460359, -1.312070483712308056 ) ) ;
#19044 = PLANE ( 'NONE',  #4984 ) ;
#19045 = ORIENTED_EDGE ( 'NONE', *, *, #24802, .T. ) ;
#19046 = DIRECTION ( 'NONE',  ( 0.000000000000000000, 0.9659258262890664248, 0.2588190451025276784 ) ) ;
#19047 = EDGE_CURVE ( 'NONE', #7898, #112, #11938, .T. ) ;
#19048 = APPROVAL ( #31772, 'UNSPECIFIED' ) ;
#19049 = VERTEX_POINT ( 'NONE', #32711 ) ;
#19050 = APPROVAL_DATE_TIME ( #13346, #9628 ) ;
#19051 = B_SPLINE_CURVE_WITH_KNOTS ( 'NONE', 3,
 ( #25294, #17577, #15076, #11208, #18581, #1194, #28940, #29264, #29117, #3069 ),
 .UNSPECIFIED., .F., .F.,
 ( 4, 3, 3, 4 ),
 ( 0.000000000000000000, 0.0005352024010578534073, 0.001070404802115707682, 0.002130599681840941728 ),
 .UNSPECIFIED. ) ;
#19052 = CARTESIAN_POINT ( 'NONE',  ( 69.07040690273157679, -6.115505791281661274, 3.995007138404602198 ) ) ;
#19053 = CARTESIAN_POINT ( 'NONE',  ( -3.407304909706596607, 1.062355717592091686, 3.000000000000001332 ) ) ;
#19054 = VERTEX_POINT ( 'NONE', #4772 ) ;
#19055 = CARTESIAN_POINT ( 'NONE',  ( 8.454317476977939450, 15.00000000000000178, -4.131740999229418954 ) ) ;
#19056 = EDGE_LOOP ( 'NONE', ( #2078, #22803, #14327, #32605 ) ) ;
#19057 = VERTEX_POINT ( 'NONE', #32537 ) ;
#19058 = LINE ( 'NONE', #11373, #28892 ) ;
#19059 = CARTESIAN_POINT ( 'NONE',  ( -3.562550801365592879, -2.752080473201636845, 2.228590825266444586 ) ) ;
#19060 = EDGE_CURVE ( 'NONE', #10466, #25076, #30122, .T. ) ;
#19061 = CARTESIAN_POINT ( 'NONE',  ( 22.04750000000000298, 2.594547506269380133, 0.7685399846772031918 ) ) ;
#19062 = CARTESIAN_POINT ( 'NONE',  ( 3.249999999999999556, -4.729683950898923683, 7.360373001730901699 ) ) ;
#19064 = ORIENTED_EDGE ( 'NONE', *, *, #423, .F. ) ;
#19063 = CYLINDRICAL_SURFACE ( 'NONE', #9600, 11.00000000000000000 ) ;
#19065 = CARTESIAN_POINT ( 'NONE',  ( -7.187550801365593323, 3.521866450007987037, 0.3701630799359328372 ) ) ;
#19066 = CARTESIAN_POINT ( 'NONE',  ( 68.76824089134483131, -7.257250553459372533, 2.184958019057942735 ) ) ;
#19067 = EDGE_CURVE ( 'NONE', #1268, #16013, #31691, .T. ) ;
#19068 = CARTESIAN_POINT ( 'NONE',  ( 14.53973501903505294, -20.67384794426875061, 1.499999999998431477 ) ) ;
#19069 = DIRECTION ( 'NONE',  ( -1.000000000000000000, -0.000000000000000000, -0.000000000000000000 ) ) ;
#19070 = VERTEX_POINT ( 'NONE', #17470 ) ;
#19072 = VERTEX_POINT ( 'NONE', #30360 ) ;
#19071 = CARTESIAN_POINT ( 'NONE',  ( 7.249760686538667009, -7.199384779417084879, -4.973063321323951236 ) ) ;
#19073 = B_SPLINE_CURVE_WITH_KNOTS ( 'NONE', 3,
 ( #21742, #23590, #8868, #11391, #6046, #18736, #21413, #11054, #1192, #13859 ),
 .UNSPECIFIED., .F., .F.,
 ( 4, 2, 2, 2, 4 ),
 ( 1.968338519010599806E-07, 0.0005467928198071728228, 0.001093388805762444439, 0.001639984791717716056, 0.002186580777672988106 ),
 .UNSPECIFIED. ) ;
#19074 = CARTESIAN_POINT ( 'NONE',  ( 21.61000000273118715, -1.573300977624594976, 1.942864903642425700 ) ) ;
#19075 = DIRECTION ( 'NONE',  ( 1.000000000000000000, -8.574039729943018344E-17, -0.000000000000000000 ) ) ;
#19076 = DIRECTION ( 'NONE',  ( -1.000000000000000000, 0.000000000000000000, -0.000000000000000000 ) ) ;
#19077 = CARTESIAN_POINT ( 'NONE',  ( -3.467105996041551119, -1.941686652642359512, -1.500000000000638156 ) ) ;
#19078 = DIRECTION ( 'NONE',  ( 8.574039729943018344E-17, 1.000000000000000000, 0.000000000000000000 ) ) ;
#19079 = B_SPLINE_SURFACE_WITH_KNOTS ( 'NONE', 3, 3, ( 
 ( #11456, #28835, #13282, #29323, #5931, #11281, #29172, #21651, #16128, #23665 ),
 ( #16445, #6260, #3281, #18490, #3761, #13926, #24148, #31857, #8925, #1275 ),
 ( #13620, #26175, #10791, #19132, #13448, #21006, #26021, #3127, #23824, #26509 ),
 ( #786, #31517, #8297, #28683, #11115, #21311, #5780, #15956, #31366, #8599 ),
 ( #936, #18817, #29020, #3610, #14772, #16800, #4439, #6912, #9425, #24817 ),
 ( #27317, #19640, #22154, #17108, #6603, #4100, #24970, #6759, #17301, #32365 ),
 ( #14616, #32517, #29509, #12257, #29836, #19989, #19304, #1936, #9578, #22468 ) ),
 .UNSPECIFIED., .F., .F., .F.,
 ( 4, 3, 4 ),
 ( 4, 3, 3, 4 ),
 ( -3.163060390574985741E-14, 0.4999999999999841793, 1.000000000000000000 ),
 ( 0.003598893295621919015, 0.5017994466481711102, 0.7508997233244456559, 1.000000000000720313 ),
 .UNSPECIFIED. ) ;
#19080 = DIRECTION ( 'NONE',  ( -1.000000000000000000, 8.574039729943019576E-17, -0.000000000000000000 ) ) ;
#19081 = CARTESIAN_POINT ( 'NONE',  ( 25.75999999999999801, -2.208672634433321348E-15, 0.000000000000000000 ) ) ;
#19082 = ORIENTED_EDGE ( 'NONE', *, *, #4266, .F. ) ;
#19083 = CARTESIAN_POINT ( 'NONE',  ( 19.75018141866911847, -21.43174828998465031, 1.668660430087062219 ) ) ;
#19084 = CARTESIAN_POINT ( 'NONE',  ( 6.037141812302426302, 8.256172215043603657, -1.911013226338322157 ) ) ;
#19086 = CARTESIAN_POINT ( 'NONE',  ( 23.67724090058579733, -17.25947716274867716, 1.422757073343390521 ) ) ;
#19085 = CARTESIAN_POINT ( 'NONE',  ( 0.000000000000000000, 0.000000000000000000, 0.000000000000000000 ) ) ;
#19087 = VERTEX_POINT ( 'NONE', #7280 ) ;
#19088 = DIRECTION ( 'NONE',  ( 0.000000000000000000, 0.000000000000000000, 1.000000000000000000 ) ) ;
#19089 = ORIENTED_EDGE ( 'NONE', *, *, #7202, .F. ) ;
#19090 = B_SPLINE_CURVE_WITH_KNOTS ( 'NONE', 3,
 ( #19790, #14258, #29498, #19125, #17099, #16792, #29316, #1929, #11448, #11758 ),
 .UNSPECIFIED., .F., .F.,
 ( 4, 2, 2, 2, 4 ),
 ( 1.968338519010600071E-07, 0.0005467928198071723891, 0.001093388805762443572, 0.001639984791717714755, 0.002186580777672986371 ),
 .UNSPECIFIED. ) ;
#19091 = CARTESIAN_POINT ( 'NONE',  ( -7.850050800000000883, -2.853674364686378695, -1.549418761218566809 ) ) ;
#19093 = EDGE_LOOP ( 'NONE', ( #1853, #16521, #8920, #180 ) ) ;
#19092 = CARTESIAN_POINT ( 'NONE',  ( 84.96587235352457412, -4.063769032899242184, -4.001039873161198024 ) ) ;
#19094 = ORIENTED_EDGE ( 'NONE', *, *, #32948, .F. ) ;
#19095 = CARTESIAN_POINT ( 'NONE',  ( 56.97280603064898941, -277.2763395528616002, -0.4463807625373443777 ) ) ;
#19096 = EDGE_CURVE ( 'NONE', #28338, #3987, #14447, .T. ) ;
#19097 = EDGE_CURVE ( 'NONE', #32424, #17772, #25345, .T. ) ;
#19098 = CARTESIAN_POINT ( 'NONE',  ( 10.00000000000000178, -4.787500056513379398, 1.476463073999621622 ) ) ;
#19100 = ORIENTED_EDGE ( 'NONE', *, *, #4474, .T. ) ;
#19099 = CARTESIAN_POINT ( 'NONE',  ( 3.063284526839887167, 0.000000000000000000, 0.000000000000000000 ) ) ;
#19101 = CARTESIAN_POINT ( 'NONE',  ( 15.00732532868866542, 9.584243418233409528, -1.499999999999998446 ) ) ;
#19102 = CARTESIAN_POINT ( 'NONE',  ( 2.453231587674435055, -16.55902999108526430, -1.747541913858293050 ) ) ;
#19103 = DIRECTION ( 'NONE',  ( 0.000000000000000000, -0.5735764363510502672, 0.8191520442889889120 ) ) ;
#19104 = CARTESIAN_POINT ( 'NONE',  ( 9.827398781245305415, -12.51289689083529488, -1.500000000000000000 ) ) ;
#19106 = ORIENTED_EDGE ( 'NONE', *, *, #3702, .F. ) ;
#19105 = CARTESIAN_POINT ( 'NONE',  ( -50.81000000000000227, -10.96999999999998643, 5.871858320049875957 ) ) ;
#19107 = CARTESIAN_POINT ( 'NONE',  ( 2.382865613620175349, 0.000000000000000000, 1.508259000770581615 ) ) ;
#19108 = B_SPLINE_CURVE_WITH_KNOTS ( 'NONE', 3,
 ( #26359, #8445, #6119, #31706 ),
 .UNSPECIFIED., .F., .F.,
 ( 4, 4 ),
 ( 2.049880227751406910E-07, 0.0008064882591616886988 ),
 .UNSPECIFIED. ) ;
#19109 = CARTESIAN_POINT ( 'NONE',  ( 18.75828436641558028, -5.879118399717574661, 3.993434336035622589 ) ) ;
#19110 = CARTESIAN_POINT ( 'NONE',  ( -1.694237876703138967, -1.500727999663424184, 4.522129901861158707 ) ) ;
#19111 = DIRECTION ( 'NONE',  ( -8.281886410780485142E-17, -0.9659258262890653146, -0.2588190451025318417 ) ) ;
#19112 = ORIENTED_EDGE ( 'NONE', *, *, #13108, .F. ) ;
#19113 = CARTESIAN_POINT ( 'NONE',  ( 7.077711312404307767E-17, 0.8254815157535250192, 4.681538312723519724 ) ) ;
#19114 = DIRECTION ( 'NONE',  ( -8.281886410780502398E-17, -0.9659258262890674240, -0.2588190451025242367 ) ) ;
#19115 = DIRECTION ( 'NONE',  ( -8.574039729943018344E-17, -1.000000000000000000, 0.000000000000000000 ) ) ;
#19116 = ORIENTED_EDGE ( 'NONE', *, *, #14282, .T. ) ;
#19117 = CARTESIAN_POINT ( 'NONE',  ( 21.34740231350966866, -21.82855858833832485, -1.313840182778319932 ) ) ;
#19118 = ORIENTED_EDGE ( 'NONE', *, *, #12326, .F. ) ;
#19119 = DIRECTION ( 'NONE',  ( -0.000000000000000000, -0.000000000000000000, -1.000000000000000000 ) ) ;
#19120 = ORIENTED_EDGE ( 'NONE', *, *, #6788, .F. ) ;
#19121 = ADVANCED_FACE ( 'NONE', ( #25159 ), #1957, .T. ) ;
#19122 = ORIENTED_EDGE ( 'NONE', *, *, #23713, .F. ) ;
#19123 = CARTESIAN_POINT ( 'NONE',  ( 47.99837860531643940, -3.577301031424836353, -2.713652344655540727 ) ) ;
#19124 = PERSON_AND_ORGANIZATION ( #8372, #9331 ) ;
#19126 = EDGE_LOOP ( 'NONE', ( #21644, #21031, #32487, #14614 ) ) ;
#19125 = CARTESIAN_POINT ( 'NONE',  ( 6.530491482054475050, -8.615020591497808411, 0.8857639883442617323 ) ) ;
#19127 = ORIENTED_EDGE ( 'NONE', *, *, #461, .F. ) ;
#19128 = CARTESIAN_POINT ( 'NONE',  ( 25.71477796605636001, 1.827236184277983400, 2.576170543363066834 ) ) ;
#19129 = VERTEX_POINT ( 'NONE', #24659 ) ;
#19130 = CARTESIAN_POINT ( 'NONE',  ( 17.97422212134408781, -19.86246923125032282, 4.522129901861158707 ) ) ;
#19131 = LINE ( 'NONE', #16799, #9115 ) ;
#19133 = ORIENTED_EDGE ( 'NONE', *, *, #5068, .T. ) ;
#19132 = CARTESIAN_POINT ( 'NONE',  ( 54.89858654026014051, -3.680211708401539106, -0.8105616792978018736 ) ) ;
#19134 = CARTESIAN_POINT ( 'NONE',  ( 22.61756301589401374, -21.90439283146508131, 1.185951968833306003 ) ) ;
#19135 = CARTESIAN_POINT ( 'NONE',  ( 17.75999999999999801, -1.902510934646483477E-15, 2.499999999999996891 ) ) ;
#19136 = EDGE_CURVE ( 'NONE', #3718, #15097, #32218, .T. ) ;
#19137 = CARTESIAN_POINT ( 'NONE',  ( 101.8666520922540002, -4.978306957426977597, 2.487811139442396957 ) ) ;
#19138 = CARTESIAN_POINT ( 'NONE',  ( 34.99999999999999289, -0.06979899340500209104, 1.001218345962048062 ) ) ;
#19139 = CARTESIAN_POINT ( 'NONE',  ( 107.5613070931556194, -18.97684952450245888, 4.540105482573447482 ) ) ;
#19140 = CARTESIAN_POINT ( 'NONE',  ( 73.25280475358511012, -21.01694209560737292, -5.485967528433938867 ) ) ;
#19141 = ADVANCED_FACE ( 'NONE', ( #2454 ), #33030, .T. ) ;
#19142 = CARTESIAN_POINT ( 'NONE',  ( 41.35712849199997976, -8.497574858407940468, -0.07017451552783590674 ) ) ;
#19143 = DIRECTION ( 'NONE',  ( 6.062761635205574522E-17, 0.7071067811865465735, 0.7071067811865484609 ) ) ;
#19144 = CARTESIAN_POINT ( 'NONE',  ( 6.357667873252800028, 7.873899671211493256, 3.476490553296878616 ) ) ;
#19145 = CARTESIAN_POINT ( 'NONE',  ( 0.000000000000000000, 0.000000000000000000, 0.000000000000000000 ) ) ;
#19146 = DIRECTION ( 'NONE',  ( -0.9975973382524638833, -0.06927878976713691683, 0.000000000000000000 ) ) ;
#19147 = B_SPLINE_CURVE_WITH_KNOTS ( 'NONE', 3,
 ( #7933, #12948, #28663, #8094, #31198, #18123, #2960, #23319, #18303, #421 ),
 .UNSPECIFIED., .F., .F.,
 ( 4, 2, 2, 2, 4 ),
 ( 1.968338519012285137E-07, 0.0005467926089500455998, 0.001093388384048189993, 0.001639984159146334278, 0.002186579934244478780 ),
 .UNSPECIFIED. ) ;
#19148 = EDGE_CURVE ( 'NONE', #28448, #3025, #13015, .T. ) ;
#19149 = CARTESIAN_POINT ( 'NONE',  ( 10.00000000000000178, -8.574039729943018837E-16, 0.000000000000000000 ) ) ;
#19150 = CARTESIAN_POINT ( 'NONE',  ( -6.550050802731187005, -0.3135853898029607456, 2.983565686104819648 ) ) ;
#19151 = VERTEX_POINT ( 'NONE', #29700 ) ;
#19152 = CARTESIAN_POINT ( 'NONE',  ( -6.250050800000000351, -2.853674364686378695, -1.549418761218566809 ) ) ;
#19153 = EDGE_CURVE ( 'NONE', #8114, #7359, #6781, .T. ) ;
#19154 = CARTESIAN_POINT ( 'NONE',  ( 107.3483866128421056, 17.35711432068121596, -3.537658942756404912 ) ) ;
#19155 = CARTESIAN_POINT ( 'NONE',  ( 18.86054332783516330, -4.736068442360130248, -3.993434336035624366 ) ) ;
#19156 = CARTESIAN_POINT ( 'NONE',  ( 7.168700580349852025, -6.410142746795773228, 1.000000000000000000 ) ) ;
#19157 = VERTEX_POINT ( 'NONE', #25850 ) ;
#19158 = CARTESIAN_POINT ( 'NONE',  ( 6.682200477904348901, -7.715721153620951789, -1.500000000000000000 ) ) ;
#19159 = ORIENTED_EDGE ( 'NONE', *, *, #16968, .F. ) ;
#19160 = CARTESIAN_POINT ( 'NONE',  ( 2.895885197758577334, -11.44804382260450204, 1.500000000000177858 ) ) ;
#19161 = DATE_AND_TIME ( #1963, #32803 ) ;
#19162 = B_SPLINE_CURVE_WITH_KNOTS ( 'NONE', 3,
 ( #22864, #9989, #4996, #7828, #4655, #14828, #32920, #5157 ),
 .UNSPECIFIED., .F., .F.,
 ( 4, 2, 2, 4 ),
 ( 0.000000000000000000, 0.5000000000000000000, 0.7500000000000000000, 1.000000000000000000 ),
 .UNSPECIFIED. ) ;
#19164 = ADVANCED_FACE ( 'NONE', ( #15448 ), #20503, .T. ) ;
#19163 = VERTEX_POINT ( 'NONE', #28171 ) ;
#19165 = CARTESIAN_POINT ( 'NONE',  ( 69.01573535414546257, -5.020529385098173591, 4.074610585184117895 ) ) ;
#19166 = EDGE_CURVE ( 'NONE', #28913, #4370, #18131, .T. ) ;
#19167 = CARTESIAN_POINT ( 'NONE',  ( -6.050050800000001061, 1.549418761218566143, -2.853674364686379583 ) ) ;
#19168 = CARTESIAN_POINT ( 'NONE',  ( 54.94755432114006766, -5.434540051867444710, -4.093303786133176914 ) ) ;
#19169 = CARTESIAN_POINT ( 'NONE',  ( 2.357329895872517955, -1.335530315079604735, 10.75444571268657512 ) ) ;
#19170 = CARTESIAN_POINT ( 'NONE',  ( 16.10106094948406863, 19.71584668020014419, 5.412820279296879811 ) ) ;
#19171 =( BOUNDED_CURVE ( )  B_SPLINE_CURVE ( 2, ( #15347, #30770, #22730, #15509, #17378, #12827, #25723, #23044, #27571 ),
 .UNSPECIFIED., .F., .F. ) 
 B_SPLINE_CURVE_WITH_KNOTS ( ( 3, 2, 2, 2, 3 ),
 ( 0.000000000000000000, 0.01562500000000000000, 0.03125000000000000000, 0.04687500000000000694, 0.06038226199343772749 ),
 .UNSPECIFIED. ) 
 CURVE ( )  GEOMETRIC_REPRESENTATION_ITEM ( )  RATIONAL_B_SPLINE_CURVE ( ( 1.000000000000000000, 0.9238795325112867385, 1.000000000000000000, 0.9238795325112867385, 1.000000000000000000, 0.9238795325112867385, 1.000000000000000000, 0.9341965377642874602, 0.9821626249036858880 ) ) 
 REPRESENTATION_ITEM ( '' )  );
#19172 = ORIENTED_EDGE ( 'NONE', *, *, #11216, .T. ) ;
#19173 = CYLINDRICAL_SURFACE ( 'NONE', #14623, 6.000000000000000000 ) ;
#19174 = CARTESIAN_POINT ( 'NONE',  ( -35.00000000000000000, 0.5174497483512504603, -2.981930256614258923 ) ) ;
#19175 = CARTESIAN_POINT ( 'NONE',  ( 2.661997850953043532, -5.196702353893143389, -8.696442646092096496 ) ) ;
#19177 = EDGE_LOOP ( 'NONE', ( #29133, #505, #15984, #13807 ) ) ;
#19176 = CARTESIAN_POINT ( 'NONE',  ( 34.48223484310469900, 0.5000000000000001110, 2.482234843104949462 ) ) ;
#19178 = DIRECTION ( 'NONE',  ( 0.9916316928896840022, -0.1290991311231002303, 6.658392840697635979E-13 ) ) ;
#19179 = CARTESIAN_POINT ( 'NONE',  ( 102.5305753040692878, -0.1042037546421146210, -0.07017451552781628354 ) ) ;
#19180 = DIRECTION ( 'NONE',  ( -0.8896831085035101783, 0.4565785435645562940, 0.000000000000000000 ) ) ;
#19181 = CARTESIAN_POINT ( 'NONE',  ( 12.44989959798877699, 0.000000000000000000, 3.000000000000044409 ) ) ;
#19182 = CARTESIAN_POINT ( 'NONE',  ( 2.592584690696360106, -9.468199582994124341, 4.120115534657283973 ) ) ;
#19183 = EDGE_CURVE ( 'NONE', #19677, #12332, #5011, .T. ) ;
#19184 = CARTESIAN_POINT ( 'NONE',  ( 0.000000000000000000, -1.464956435139616930, 10.90201369670498011 ) ) ;
#19185 = FACE_OUTER_BOUND ( 'NONE', #8550, .T. ) ;
#19186 = DIRECTION ( 'NONE',  ( -1.000000000000000000, 0.000000000000000000, -0.000000000000000000 ) ) ;
#19187 = AXIS2_PLACEMENT_3D ( 'NONE', #14609, #6407, #24810 ) ;
#19188 = CARTESIAN_POINT ( 'NONE',  ( -0.7867377105083910305, -2.707992247746365599, 5.485967528433933538 ) ) ;
#19189 = ORIENTED_EDGE ( 'NONE', *, *, #9172, .T. ) ;
#19190 = CARTESIAN_POINT ( 'NONE',  ( 20.67250000273118715, -2.378061970571983430, 1.291182301015471490 ) ) ;
#19191 = ORIENTED_EDGE ( 'NONE', *, *, #9690, .T. ) ;
#19192 = FACE_OUTER_BOUND ( 'NONE', #19444, .T. ) ;
#19193 = VECTOR ( 'NONE', #7919, 999.9999999999998863 ) ;
#19194 = CARTESIAN_POINT ( 'NONE',  ( 3.249999999999999556, 0.000000000000000000, 0.000000000000000000 ) ) ;
#19195 = CARTESIAN_POINT ( 'NONE',  ( 107.4543400279316216, -17.42228489399607128, -4.691808660060365455 ) ) ;
#19196 = DIRECTION ( 'NONE',  ( 2.219124775574870561E-17, 0.2588190451025141336, 0.9659258262890700886 ) ) ;
#19197 = CARTESIAN_POINT ( 'NONE',  ( 0.7632845268398871230, -4.729683950898817102, -7.360373001730970977 ) ) ;
#19198 = ORIENTED_EDGE ( 'NONE', *, *, #30836, .F. ) ;
#19199 = CARTESIAN_POINT ( 'NONE',  ( -57.64172636127213423, -3.383636359799072846, 5.845147464816284000 ) ) ;
#19200 = EDGE_CURVE ( 'NONE', #26609, #11371, #1287, .T. ) ;
#19201 = VERTEX_POINT ( 'NONE', #7615 ) ;
#19202 = COORDINATED_UNIVERSAL_TIME_OFFSET ( 0, 0, .AHEAD. ) ;
#19203 = EDGE_CURVE ( 'NONE', #17832, #8403, #14604, .T. ) ;
#19204 = CARTESIAN_POINT ( 'NONE',  ( 69.07045576165747036, -6.116484151792160873, 3.993434826686585115 ) ) ;
#19205 = ADVANCED_FACE ( 'NONE', ( #30870 ), #23473, .T. ) ;
#19206 = AXIS2_PLACEMENT_3D ( 'NONE', #30362, #32714, #4954 ) ;
#19207 = DIRECTION ( 'NONE',  ( 1.000000000000000000, 0.000000000000000000, 1.388624693425297016E-14 ) ) ;
#19208 = AXIS2_PLACEMENT_3D ( 'NONE', #26989, #16605, #9570 ) ;
#19209 = ORIENTED_EDGE ( 'NONE', *, *, #20906, .T. ) ;
#19210 = CARTESIAN_POINT ( 'NONE',  ( 5.612974384376779646, 3.934067627273206025, 7.213266193303272011 ) ) ;
#19211 = B_SPLINE_CURVE_WITH_KNOTS ( 'NONE', 3,
 ( #5069, #28622, #10899, #27965 ),
 .UNSPECIFIED., .F., .F.,
 ( 4, 4 ),
 ( 0.005731821976040855568, 0.005732069968807134569 ),
 .UNSPECIFIED. ) ;
#19212 = B_SPLINE_CURVE_WITH_KNOTS ( 'NONE', 3,
 ( #6557, #21924, #32144, #9217, #19447, #16911, #29640, #19597, #6721, #32327 ),
 .UNSPECIFIED., .F., .F.,
 ( 4, 2, 2, 2, 4 ),
 ( 1.968338519003748898E-07, 0.0005467926089500447324, 0.001093388384048189126, 0.001639984159146333411, 0.002186579934244477913 ),
 .UNSPECIFIED. ) ;
#19213 = ORIENTED_EDGE ( 'NONE', *, *, #7278, .F. ) ;
#19214 = VERTEX_POINT ( 'NONE', #28022 ) ;
#19215 = CARTESIAN_POINT ( 'NONE',  ( 24.67249999999999943, -1.291182301015472600, -2.378061970571982098 ) ) ;
#19216 = CARTESIAN_POINT ( 'NONE',  ( -3.822634483660923045E-16, -4.458382051008209501, 2.285372942704937849 ) ) ;
#19217 = CARTESIAN_POINT ( 'NONE',  ( 21.79750000000000654, 0.7685399846772009713, -2.594547506269381909 ) ) ;
#19218 = LINE ( 'NONE', #19062, #16099 ) ;
#19219 = AXIS2_PLACEMENT_3D ( 'NONE', #10086, #14619, #32688 ) ;
#19221 = VERTEX_POINT ( 'NONE', #15943 ) ;
#19220 = DIRECTION ( 'NONE',  ( -1.000000000000000000, 0.000000000000000000, 0.000000000000000000 ) ) ;
#19222 = CARTESIAN_POINT ( 'NONE',  ( -7.787550801365593856, -0.3701630799359326152, 3.521866450007987037 ) ) ;
#19223 = CARTESIAN_POINT ( 'NONE',  ( -38.14293509397969473, 10.97000000000000419, -1.050000000000000044 ) ) ;
#19224 = CARTESIAN_POINT ( 'NONE',  ( 5.377543748152547209, 1.391664247347333294, -7.892520144992419162 ) ) ;
#19225 = LINE ( 'NONE', #29762, #19957 ) ;
#19226 = EDGE_LOOP ( 'NONE', ( #23919, #29161, #9416, #6184 ) ) ;
#19227 = VERTEX_POINT ( 'NONE', #99 ) ;
#19228 = ADVANCED_FACE ( 'NONE', ( #7941 ), #584, .T. ) ;
#19229 = APPROVAL ( #2649, 'UNSPECIFIED' ) ;
#19230 = CARTESIAN_POINT ( 'NONE',  ( 4.749760686538667009, 4.007137495034909236, -6.940565734314555257 ) ) ;
#19231 = CARTESIAN_POINT ( 'NONE',  ( 21.98500000273118715, -0.2613211581691358698, -2.486304738420681559 ) ) ;
#19232 = CIRCLE ( 'NONE', #29392, 0.5000000000000000000 ) ;
#19233 = LINE ( 'NONE', #24560, #5510 ) ;
#19234 = AXIS2_PLACEMENT_3D ( 'NONE', #11007, #23866, #21207 ) ;
#19235 = CARTESIAN_POINT ( 'NONE',  ( -30.67627260417763679, 12.22102706438213460, 1.500000000000000000 ) ) ;
#19236 = DIRECTION ( 'NONE',  ( 0.000000000000000000, 0.000000000000000000, -1.000000000000000000 ) ) ;
#19237 = CARTESIAN_POINT ( 'NONE',  ( 2.037945749704312686E-16, 2.376879293651064540, 4.116875700062091248 ) ) ;
#19238 = VECTOR ( 'NONE', #3945, 1000.000000000000000 ) ;
#19239 = CARTESIAN_POINT ( 'NONE',  ( 35.34133959475772713, -3.844168172129504679, 0.8105616794551323556 ) ) ;
#19240 = CARTESIAN_POINT ( 'NONE',  ( 0.000000000000000000, 0.000000000000000000, 0.000000000000000000 ) ) ;
#19241 = CARTESIAN_POINT ( 'NONE',  ( 101.7156419778298471, -2.803798876308493782, 3.841991596727068359 ) ) ;
#19242 = EDGE_LOOP ( 'NONE', ( #26196, #7579, #22065, #18729 ) ) ;
#19243 = EDGE_CURVE ( 'NONE', #31676, #8978, #5118, .T. ) ;
#19244 = LINE ( 'NONE', #21751, #5008 ) ;
#19245 = CARTESIAN_POINT ( 'NONE',  ( 10.56183597391177464, -1.750323540954535505E-14, 4.753758587302147731 ) ) ;
#19247 = CARTESIAN_POINT ( 'NONE',  ( 6.530491712438077023, -7.792522225867670294, 3.778856441136694500 ) ) ;
#19246 = CARTESIAN_POINT ( 'NONE',  ( -3.450050800000000084, 2.853674364686379583, 1.549418761218565921 ) ) ;
#19248 = ORIENTED_EDGE ( 'NONE', *, *, #28587, .T. ) ;
#19249 = DIRECTION ( 'NONE',  ( 0.000000000000000000, 2.486899575160350335E-14, 1.000000000000000000 ) ) ;
#19250 = ORIENTED_EDGE ( 'NONE', *, *, #6005, .T. ) ;
#19251 = DIRECTION ( 'NONE',  ( 0.000000000000000000, -0.9510565162951566398, 0.3090169943749382364 ) ) ;
#19253 = EDGE_LOOP ( 'NONE', ( #8254, #22368, #32622, #1385 ) ) ;
#19252 = CARTESIAN_POINT ( 'NONE',  ( 40.87774300910533753, -5.750695475552364044, -3.996604168388419698 ) ) ;
#19254 = VECTOR ( 'NONE', #14527, 1000.000000000000000 ) ;
#19255 = VERTEX_POINT ( 'NONE', #15636 ) ;
#19256 = AXIS2_PLACEMENT_3D ( 'NONE', #14037, #21891, #14347 ) ;
#19257 = CARTESIAN_POINT ( 'NONE',  ( -5.900050802731187538, 2.853674364686379583, 1.549418761218565921 ) ) ;
#19259 = ORIENTED_EDGE ( 'NONE', *, *, #2657, .F. ) ;
#19258 = CARTESIAN_POINT ( 'NONE',  ( -3.828276826527910348, -10.43768764654175918, -1.500000000000000222 ) ) ;
#19260 = CARTESIAN_POINT ( 'NONE',  ( -4.112942406915325755, -5.022711880624455567E-15, 2.999999999999999556 ) ) ;
#19261 = CIRCLE ( 'NONE', #36, 0.5000000000000004441 ) ;
#19262 = CARTESIAN_POINT ( 'NONE',  ( 9.127968561342507670, 0.03517121848167529402, -1.257822814154247126 ) ) ;
#19263 = DIRECTION ( 'NONE',  ( 8.574039729943018344E-17, 1.000000000000000000, 0.000000000000000000 ) ) ;
#19264 = CARTESIAN_POINT ( 'NONE',  ( 10.90710808056851278, -12.60204455863677531, -1.499999999999860112 ) ) ;
#19267 = EDGE_CURVE ( 'NONE', #19723, #15877, #2847, .T. ) ;
#19266 = ORIENTED_EDGE ( 'NONE', *, *, #24186, .F. ) ;
#19265 = CARTESIAN_POINT ( 'NONE',  ( 108.0601201328837817, -18.93507707413851904, -4.559426007957987359 ) ) ;
#19268 = DIRECTION ( 'NONE',  ( 0.000000000000000000, 1.000000000000000000, 0.000000000000000000 ) ) ;
#19269 = TOROIDAL_SURFACE ( 'NONE', #23010, 3.895301350492843540, 15.00000000000000178 ) ;
#19270 = B_SPLINE_CURVE_WITH_KNOTS ( 'NONE', 3,
 ( #29634, #22417, #24420, #32629, #6715, #16906, #27099, #9710 ),
 .UNSPECIFIED., .F., .F.,
 ( 4, 2, 2, 4 ),
 ( 2.851296507450002721E-07, 0.001262135616845466582, 0.001893060860442827027, 0.002523986104040187688 ),
 .UNSPECIFIED. ) ;
#19271 = DIRECTION ( 'NONE',  ( 0.07591486983599084193, 0.4227239498239174220, 0.9030733053208088723 ) ) ;
#19272 = CARTESIAN_POINT ( 'NONE',  ( 41.35325844292899689, -7.141637217102140056, 3.390608916434175057 ) ) ;
#19273 = DESIGN_CONTEXT ( 'detailed design', #7986, 'design' ) ;
#19274 = CARTESIAN_POINT ( 'NONE',  ( -2.794738735352967574, 0.000000000000000000, 1.292893218813452538 ) ) ;
#19275 = CARTESIAN_POINT ( 'NONE',  ( 0.000000000000000000, -4.472189673936727949, -8.264486777890155622 ) ) ;
#19276 = ORIENTED_EDGE ( 'NONE', *, *, #10839, .T. ) ;
#19277 = CARTESIAN_POINT ( 'NONE',  ( 7.249760686538667009, 2.741043480754926875, 7.530955069117522882 ) ) ;
#19278 = B_SPLINE_CURVE_WITH_KNOTS ( 'NONE', 3,
 ( #19071, #11540, #27077, #4352, #12190, #19410, #32297, #24397, #26744, #1366 ),
 .UNSPECIFIED., .F., .F.,
 ( 4, 2, 2, 2, 4 ),
 ( 1.968338519011545042E-07, 0.0005467926395225672191, 0.001093388445193233232, 0.001639984250863899245, 0.002186580056534565258 ),
 .UNSPECIFIED. ) ;
#19279 = AXIS2_PLACEMENT_3D ( 'NONE', #24330, #6128, #1441 ) ;
#19280 = CARTESIAN_POINT ( 'NONE',  ( -10.00000000000000000, 0.000000000000000000, 0.000000000000000000 ) ) ;
#19281 = EDGE_CURVE ( 'NONE', #23666, #24626, #30718, .T. ) ;
#19282 = CARTESIAN_POINT ( 'NONE',  ( 25.23499999999999943, 0.2613211581691317065, 2.486304738420681559 ) ) ;
#19283 = ORIENTED_EDGE ( 'NONE', *, *, #27162, .T. ) ;
#19284 = ADVANCED_FACE ( 'NONE', ( #17983 ), #8119, .F. ) ;
#19285 = AXIS2_PLACEMENT_3D ( 'NONE', #27239, #4181, #22578 ) ;
#19286 = VECTOR ( 'NONE', #1284, 1000.000000000000000 ) ;
#19287 = VECTOR ( 'NONE', #20382, 1000.000000000000000 ) ;
#19288 = EDGE_CURVE ( 'NONE', #21586, #12444, #30664, .T. ) ;
#19289 = DIRECTION ( 'NONE',  ( 0.000000000000000000, 1.000000000000000000, 0.000000000000000000 ) ) ;
#19290 = CARTESIAN_POINT ( 'NONE',  ( 2.976845773540289564, 8.532418605434726189, 3.349682859779522737 ) ) ;
#19291 = ORIENTED_EDGE ( 'NONE', *, *, #25534, .T. ) ;
#19292 = CARTESIAN_POINT ( 'NONE',  ( 2.318812167152461967, -10.58295493561522882, -1.500000000000000444 ) ) ;
#19293 = ORIENTED_EDGE ( 'NONE', *, *, #22273, .T. ) ;
#19294 = CIRCLE ( 'NONE', #17684, 12.62979293944910353 ) ;
#19295 = ORIENTED_EDGE ( 'NONE', *, *, #13858, .T. ) ;
#19296 = CARTESIAN_POINT ( 'NONE',  ( 7.249760686538667009, 3.647351267791679508, -7.953573330858177748 ) ) ;
#19298 = ORIENTED_EDGE ( 'NONE', *, *, #12396, .T. ) ;
#19297 = DIRECTION ( 'NONE',  ( 0.1437473352845037022, 0.000000000000000000, -0.9896144216807900573 ) ) ;
#19299 = EDGE_LOOP ( 'NONE', ( #6582, #31173, #9532, #17984 ) ) ;
#19300 = CARTESIAN_POINT ( 'NONE',  ( 22.04750000136559507, -3.024605502323851169, 0.3178988483021052969 ) ) ;
#19301 = VERTEX_POINT ( 'NONE', #16108 ) ;
#19302 = CARTESIAN_POINT ( 'NONE',  ( 10.00000000000000178, -8.574039729943018837E-16, 0.000000000000000000 ) ) ;
#19303 = DIRECTION ( 'NONE',  ( -0.4999999999999981126, -0.8660254037844395958, 0.000000000000000000 ) ) ;
#19305 = VERTEX_POINT ( 'NONE', #31352 ) ;
#19304 = CARTESIAN_POINT ( 'NONE',  ( 35.33267181913306842, -4.397467831974085861, -2.184956776455117211 ) ) ;
#19306 = CARTESIAN_POINT ( 'NONE',  ( 0.7632845268398871230, 0.000000000000000000, 0.000000000000000000 ) ) ;
#19307 = CARTESIAN_POINT ( 'NONE',  ( 34.62197427260419147, 18.00000000000000355, -0.3975189810868455798 ) ) ;
#19308 = VECTOR ( 'NONE', #15249, 1000.000000000000000 ) ;
#19309 = CARTESIAN_POINT ( 'NONE',  ( -56.76951762135347224, 0.4049278075578381930, 1.763939777626597705 ) ) ;
#19310 = DIRECTION ( 'NONE',  ( 1.000000000000000000, -0.000000000000000000, -0.000000000000000000 ) ) ;
#19311 = CIRCLE ( 'NONE', #3852, 2.999999999999999112 ) ;
#19312 = AXIS2_PLACEMENT_3D ( 'NONE', #10272, #10595, #20799 ) ;
#19313 = AXIS2_PLACEMENT_3D ( 'NONE', #20647, #30853, #7922 ) ;
#19314 = CARTESIAN_POINT ( 'NONE',  ( 0.5220033361344523781, 0.000000000000000000, -5.485967528433937979 ) ) ;
#19315 = CARTESIAN_POINT ( 'NONE',  ( 110.8079127523828618, 15.75827621748124940, 1.508259000770581615 ) ) ;
#19316 = LINE ( 'NONE', #8936, #21066 ) ;
#19317 = APPLICATION_CONTEXT ( 'configuration controlled 3d designs of mechanical parts and assemblies' ) ;
#19318 = AXIS2_PLACEMENT_3D ( 'NONE', #25132, #24969, #2253 ) ;
#19319 = CIRCLE ( 'NONE', #16105, 5.500000000000001776 ) ;
#19320 = VECTOR ( 'NONE', #32773, 1000.000000000000000 ) ;
#19321 = EDGE_CURVE ( 'NONE', #3441, #20330, #28325, .T. ) ;
#19322 = CARTESIAN_POINT ( 'NONE',  ( 6.530491627857224479, 7.903708701126691771, 3.540416224243698284 ) ) ;
#19323 = CARTESIAN_POINT ( 'NONE',  ( 3.936147556303794648, 18.00000000000000355, -4.854816414140051606 ) ) ;
#19324 = CARTESIAN_POINT ( 'NONE',  ( -31.18783180709124636, -25.43932300454937234, 1.500000000000000000 ) ) ;
#19325 = CARTESIAN_POINT ( 'NONE',  ( 3.499999999999999556, -5.979767908488853756, 1.814490771706161354 ) ) ;
#19326 = CARTESIAN_POINT ( 'NONE',  ( -6.600050802731186828, 0.9222479816126443186, 3.113457007523260156 ) ) ;
#19327 = ORIENTED_EDGE ( 'NONE', *, *, #10481, .T. ) ;
#19328 = CARTESIAN_POINT ( 'NONE',  ( -5.850050800000001772, 2.853674364686379583, 1.549418761218565921 ) ) ;
#19329 = AXIS2_PLACEMENT_3D ( 'NONE', #2415, #16969, #14907 ) ;
#19330 = AXIS2_PLACEMENT_3D ( 'NONE', #14396, #22286, #12236 ) ;
#19331 = CARTESIAN_POINT ( 'NONE',  ( 107.4385791398478602, 17.85938043952733878, -4.612695725900422872 ) ) ;
#19332 = CARTESIAN_POINT ( 'NONE',  ( -5.762942409646513831, 3.284080845023683730E-15, 3.000000000000000000 ) ) ;
#19333 = CARTESIAN_POINT ( 'NONE',  ( -40.76530497340966264, -12.76917967239650942, 5.871858320049882174 ) ) ;
#19335 = VERTEX_POINT ( 'NONE', #29490 ) ;
#19334 = AXIS2_PLACEMENT_3D ( 'NONE', #32074, #1154, #24217 ) ;
#19336 = CARTESIAN_POINT ( 'NONE',  ( 6.680689650589764383, -6.092366900306257271, -1.500000000000000000 ) ) ;
#19337 = AXIS2_PLACEMENT_3D ( 'NONE', #29527, #6772, #29847 ) ;
#19338 = VECTOR ( 'NONE', #21816, 1000.000000000000000 ) ;
#19339 = AXIS2_PLACEMENT_3D ( 'NONE', #1674, #29761, #27232 ) ;
#19340 = ORIENTED_EDGE ( 'NONE', *, *, #21438, .F. ) ;
#19341 = CARTESIAN_POINT ( 'NONE',  ( 1.653004494525485146, -10.31337013662990998, 1.499999999999999556 ) ) ;
#19342 = APPROVAL_STATUS ( 'not_yet_approved' ) ;
#19343 = CYLINDRICAL_SURFACE ( 'NONE', #3264, 11.00000000000000000 ) ;
#19344 = ORIENTED_EDGE ( 'NONE', *, *, #6356, .F. ) ;
#19345 = CARTESIAN_POINT ( 'NONE',  ( -4.176545177854389834, -3.225705193879217170, 1.500000000000000888 ) ) ;
#19346 = AXIS2_PLACEMENT_3D ( 'NONE', #19926, #9521, #21906 ) ;
#19347 = AXIS2_PLACEMENT_3D ( 'NONE', #5591, #15774, #5736 ) ;
#19348 = CARTESIAN_POINT ( 'NONE',  ( 0.000000000000000000, 18.00000000000000355, 0.000000000000000000 ) ) ;
#19349 = CARTESIAN_POINT ( 'NONE',  ( 54.97582481754341899, -6.455996908956627145, -4.074610066671311870 ) ) ;
#19350 = CARTESIAN_POINT ( 'NONE',  ( 2.976845687893342696, -0.5490754078163165852, 9.149921655307466040 ) ) ;
#19351 = DIRECTION ( 'NONE',  ( 8.519590295723598769E-19, 5.916484360648977690E-20, 1.000000000000000000 ) ) ;
#19352 = VERTEX_POINT ( 'NONE', #29307 ) ;
#19353 = EDGE_CURVE ( 'NONE', #17584, #1029, #20765, .T. ) ;
#19354 = CARTESIAN_POINT ( 'NONE',  ( 9.174708406371134828, 0.09531162291655140284, 1.030456265918283210 ) ) ;
#19355 = CARTESIAN_POINT ( 'NONE',  ( 22.65740490676343555, -21.90673157959303197, -1.180310388834369784 ) ) ;
#19356 = CARTESIAN_POINT ( 'NONE',  ( 18.86054332783516330, -4.736068442360130248, -3.993434336035624366 ) ) ;
#19358 = ORIENTED_EDGE ( 'NONE', *, *, #20254, .F. ) ;
#19357 = FACE_OUTER_BOUND ( 'NONE', #30176, .T. ) ;
#19359 = VECTOR ( 'NONE', #3612, 1000.000000000000000 ) ;
#19360 = CARTESIAN_POINT ( 'NONE',  ( -28.35000000000000497, -10.96966150227469505, 1.500000000000000000 ) ) ;
#19361 = EDGE_CURVE ( 'NONE', #16234, #10253, #29035, .T. ) ;
#19362 = AXIS2_PLACEMENT_3D ( 'NONE', #15033, #25256, #30790 ) ;
#19363 = DIRECTION ( 'NONE',  ( 0.7071067811865449082, 8.659560562354964906E-17, 0.7071067811865501263 ) ) ;
#19364 = CARTESIAN_POINT ( 'NONE',  ( -4.350050802731187716, 2.983565686104819648, 0.3135853898029609677 ) ) ;
#19365 = DIRECTION ( 'NONE',  ( -3.020323503847002675E-16, -0.9993908270190956511, 0.03489949670250104552 ) ) ;
#19366 = CARTESIAN_POINT ( 'NONE',  ( 7.249760686538667009, -7.530955069117495349, -2.741043480755002371 ) ) ;
#19367 = VECTOR ( 'NONE', #20768, 1000.000000000000000 ) ;
#19368 = AXIS2_PLACEMENT_3D ( 'NONE', #29434, #3554, #27085 ) ;
#19369 = AXIS2_PLACEMENT_3D ( 'NONE', #12763, #19816, #7783 ) ;
#19370 = DIRECTION ( 'NONE',  ( 1.000000000000000000, -0.000000000000000000, -0.000000000000000000 ) ) ;
#19371 = CARTESIAN_POINT ( 'NONE',  ( 25.96712173632212384, 22.75279134953750670, -5.471072653611063430 ) ) ;
#19372 = CARTESIAN_POINT ( 'NONE',  ( 3.499999999999999556, 6.704570150427012543, -2.172265885002588437 ) ) ;
#19373 = ORIENTED_EDGE ( 'NONE', *, *, #6641, .T. ) ;
#19374 = ADVANCED_FACE ( 'NONE', ( #3744 ), #19648, .T. ) ;
#19375 = VECTOR ( 'NONE', #16860, 1000.000000000000000 ) ;
#19376 = EDGE_CURVE ( 'NONE', #31676, #21250, #18895, .T. ) ;
#19377 = CARTESIAN_POINT ( 'NONE',  ( -2.956376981307136553, 0.1572233378491263989, -2.999999999999999556 ) ) ;
#19378 = ORIENTED_EDGE ( 'NONE', *, *, #29402, .F. ) ;
#19379 = AXIS2_PLACEMENT_3D ( 'NONE', #30292, #4555, #9381 ) ;
#19380 = DIRECTION ( 'NONE',  ( 1.000000000000000000, 0.000000000000000000, -0.000000000000000000 ) ) ;
#19381 = CARTESIAN_POINT ( 'NONE',  ( 0.000000000000000000, -0.5000000000000000000, -1.500000000000000000 ) ) ;
#19382 = CYLINDRICAL_SURFACE ( 'NONE', #31176, 2.999999999999999112 ) ;
#19383 = CARTESIAN_POINT ( 'NONE',  ( 109.4269204146996515, 20.46634128623930948, -2.043459231800118125 ) ) ;
#19384 = DIRECTION ( 'NONE',  ( 0.000000000000000000, 0.2588190451025359495, -0.9659258262890643154 ) ) ;
#19385 = EDGE_LOOP ( 'NONE', ( #17413, #21476, #3893 ) ) ;
#19386 = CARTESIAN_POINT ( 'NONE',  ( 10.00000000000000000, -0.8254815157534940440, -4.681538312723525053 ) ) ;
#19387 = EDGE_CURVE ( 'NONE', #24063, #4399, #8232, .T. ) ;
#19388 = CIRCLE ( 'NONE', #22586, 6.500000000000002665 ) ;
#19389 = ORIENTED_EDGE ( 'NONE', *, *, #14754, .T. ) ;
#19390 = APPROVAL_DATE_TIME ( #14328, #28044 ) ;
#19391 = CARTESIAN_POINT ( 'NONE',  ( 69.07035661562366613, -6.114499741367263042, 3.996605157046045687 ) ) ;
#19392 = VECTOR ( 'NONE', #5345, 1000.000000000000114 ) ;
#19393 = VECTOR ( 'NONE', #8982, 1000.000000000000000 ) ;
#19395 = ADVANCED_FACE ( 'NONE', ( #27637 ), #14909, .T. ) ;
#19394 = AXIS2_PLACEMENT_3D ( 'NONE', #25572, #2681, #5531 ) ;
#19396 = CARTESIAN_POINT ( 'NONE',  ( -5.750050799999999462, 0.000000000000000000, 0.000000000000000000 ) ) ;
#19397 = CARTESIAN_POINT ( 'NONE',  ( 4.749760686538667009, 1.391664247347333294, -7.892520144992419162 ) ) ;
#19398 = EDGE_LOOP ( 'NONE', ( #27426, #12288, #3227, #20163 ) ) ;
#19399 = ORIENTED_EDGE ( 'NONE', *, *, #14146, .F. ) ;
#19400 = CARTESIAN_POINT ( 'NONE',  ( 24.74290772321993970, -0.1310194482076044442, -2.499999999999998668 ) ) ;
#19401 = CARTESIAN_POINT ( 'NONE',  ( 5.489344046532323773, -7.082516960462288402, -3.969101778623997046 ) ) ;
#19402 = CARTESIAN_POINT ( 'NONE',  ( 24.48499999999999943, -2.486304738420683780, 0.2613211581691335383 ) ) ;
#19403 = CARTESIAN_POINT ( 'NONE',  ( 3.708298821157957725, -12.03564075718119852, -1.499999999999999556 ) ) ;
#19405 = EDGE_LOOP ( 'NONE', ( #20250, #2434, #32196, #4150 ) ) ;
#19404 = CARTESIAN_POINT ( 'NONE',  ( 6.356382399260308347, 3.797266095948589992, -7.723816458760309089 ) ) ;
#19406 = CARTESIAN_POINT ( 'NONE',  ( -3.087550801365593234, 2.228590825266444142, 2.752080473201636845 ) ) ;
#19407 = DIRECTION ( 'NONE',  ( 0.000000000000000000, 0.000000000000000000, -1.000000000000000000 ) ) ;
#19408 = DIRECTION ( 'NONE',  ( 1.000000000000000000, -0.000000000000000000, -0.000000000000000000 ) ) ;
#19409 = ORIENTED_EDGE ( 'NONE', *, *, #32089, .T. ) ;
#19411 = EDGE_LOOP ( 'NONE', ( #7430, #13827, #8357, #13351 ) ) ;
#19410 = CARTESIAN_POINT ( 'NONE',  ( 6.038145208238973716, -7.104833038995682415, -4.620191422127199132 ) ) ;
#19412 = CIRCLE ( 'NONE', #11939, 299.3348442831094758 ) ;
#19413 = CIRCLE ( 'NONE', #9247, 3.000000000000000444 ) ;
#19414 = CARTESIAN_POINT ( 'NONE',  ( 20.33529679551776681, 16.25852880933178213, 1.500000000000000444 ) ) ;
#19415 = AXIS2_PLACEMENT_3D ( 'NONE', #11554, #21598, #21421 ) ;
#19416 = DIRECTION ( 'NONE',  ( 0.000000000000000000, -0.4067366430757887175, -0.9135454576426059736 ) ) ;
#19417 = EDGE_CURVE ( 'NONE', #32515, #14230, #4585, .T. ) ;
#19418 = VECTOR ( 'NONE', #3785, 1000.000000000000000 ) ;
#19419 = EDGE_CURVE ( 'NONE', #3811, #22609, #17290, .T. ) ;
#19420 = AXIS2_PLACEMENT_3D ( 'NONE', #27482, #24448, #19472 ) ;
#19421 = CARTESIAN_POINT ( 'NONE',  ( -19.95676506897028091, 17.93667199019918357, 1.500000000000000000 ) ) ;
#19422 = CIRCLE ( 'NONE', #26374, 300.9381170038701612 ) ;
#19423 = CARTESIAN_POINT ( 'NONE',  ( -6.250050802731187183, -1.887961173149512062, -2.331437884370912261 ) ) ;
#19424 = DIRECTION ( 'NONE',  ( 0.000000000000000000, -1.000000000000000000, 0.000000000000000000 ) ) ;
#19425 = DIRECTION ( 'NONE',  ( -1.000000000000000000, 0.000000000000000000, -8.673617379884027583E-16 ) ) ;
#19426 = APPROVAL_PERSON_ORGANIZATION ( #1656, #8398, #4163 ) ;
#19427 = CARTESIAN_POINT ( 'NONE',  ( 54.89716490668162407, -3.628845007888942042, 0.4367666026990714156 ) ) ;
#19428 = CARTESIAN_POINT ( 'NONE',  ( 3.249999999999999556, -1.699438267350306120, -9.241976615262172956 ) ) ;
#19429 = VERTEX_POINT ( 'NONE', #2070 ) ;
#19430 = ADVANCED_FACE ( 'NONE', ( #17285 ), #19622, .T. ) ;
#19431 = CARTESIAN_POINT ( 'NONE',  ( 4.749760686538667009, 4.007137495034812424, 6.940565734314612101 ) ) ;
#19432 = VERTEX_POINT ( 'NONE', #27300 ) ;
#19433 = FACE_OUTER_BOUND ( 'NONE', #9571, .T. ) ;
#19434 = CARTESIAN_POINT ( 'NONE',  ( 0.000000000000000000, 0.000000000000000000, 0.000000000000000000 ) ) ;
#19436 = CARTESIAN_POINT ( 'NONE',  ( 107.4497430981611075, -17.35563866676828582, 4.509685912366180105 ) ) ;
#19435 = PLANE ( 'NONE',  #1161 ) ;
#19437 = ORIENTED_EDGE ( 'NONE', *, *, #32044, .T. ) ;
#19438 = ADVANCED_FACE ( 'NONE', ( #32667 ), #7246, .F. ) ;
#19439 = CIRCLE ( 'NONE', #10909, 7.482234843104714983 ) ;
#19440 = CARTESIAN_POINT ( 'NONE',  ( 19.66689578795203985, -21.64324770234357587, 1.457654425243584129 ) ) ;
#19441 = ORIENTED_EDGE ( 'NONE', *, *, #22336, .T. ) ;
#19442 = FACE_OUTER_BOUND ( 'NONE', #5282, .T. ) ;
#19444 = EDGE_LOOP ( 'NONE', ( #27176, #18400, #13248, #22041 ) ) ;
#19443 = CARTESIAN_POINT ( 'NONE',  ( 102.3441187013863356, -2.856883908061261579, -3.996604656719260351 ) ) ;
#19445 = VERTEX_POINT ( 'NONE', #4421 ) ;
#19446 = AXIS2_PLACEMENT_3D ( 'NONE', #22494, #17818, #30530 ) ;
#19447 = CARTESIAN_POINT ( 'NONE',  ( 6.357668022120091855, 5.959864878090759710, -6.210015626210324768 ) ) ;
#19448 = CARTESIAN_POINT ( 'NONE',  ( -12.44989959798873791, 0.5000000000000000000, -2.482234843104710986 ) ) ;
#19450 = EDGE_LOOP ( 'NONE', ( #19191, #14149, #20460, #18627 ) ) ;
#19449 = CARTESIAN_POINT ( 'NONE',  ( 17.33093461831547444, -21.43932300456618378, -1.500000000000000000 ) ) ;
#19451 = CARTESIAN_POINT ( 'NONE',  ( 12.93640105133131257, 7.016868255687757738, -1.500000000000000000 ) ) ;
#19452 = CARTESIAN_POINT ( 'NONE',  ( 22.74290772321994325, -0.1310194482076041944, -2.499999999999998224 ) ) ;
#19453 = CARTESIAN_POINT ( 'NONE',  ( 5.377543748152549874, -2.741043480754977946, 7.530955069117504230 ) ) ;
#19454 = CC_DESIGN_SECURITY_CLASSIFICATION ( #15168, ( #7706 ) ) ;
#19455 = CARTESIAN_POINT ( 'NONE',  ( 7.154313482939221203, -6.723190066306958812, -1.500000000000143219 ) ) ;
#19457 = VERTEX_POINT ( 'NONE', #4739 ) ;
#19456 = CARTESIAN_POINT ( 'NONE',  ( 107.5591617223737018, -18.94572639363423860, -4.614305386542819853 ) ) ;
#19458 = CARTESIAN_POINT ( 'NONE',  ( 2.502438769489224502, 0.2071067811865478503, 1.500000000000000444 ) ) ;
#19459 = CARTESIAN_POINT ( 'NONE',  ( 7.249760686538667009, -7.135485519862032611, 5.064320921489797733 ) ) ;
#19460 = CARTESIAN_POINT ( 'NONE',  ( 101.8797206818347973, -5.166491396334524033, 2.184956718991889257 ) ) ;
#19461 = EDGE_CURVE ( 'NONE', #27353, #25919, #16207, .T. ) ;
#19462 = CARTESIAN_POINT ( 'NONE',  ( 4.716257286563768858, 20.00000000000000000, 4.924645716438879717 ) ) ;
#19463 = CARTESIAN_POINT ( 'NONE',  ( 0.5704037183048228377, -8.085411865508387308, -5.066169706250034821 ) ) ;
#19464 = AXIS2_PLACEMENT_3D ( 'NONE', #13294, #7965, #8136 ) ;
#19465 = ORIENTED_EDGE ( 'NONE', *, *, #6735, .T. ) ;
#19466 = CARTESIAN_POINT ( 'NONE',  ( -6.450050800000000528, -1.549418761218565255, 2.853674364686380471 ) ) ;
#19467 = B_SPLINE_CURVE_WITH_KNOTS ( 'NONE', 3,
 ( #765, #13749, #15939, #15629, #31016, #10767, #25845, #578, #5619, #31496, #10451, #23469 ),
 .UNSPECIFIED., .F., .F.,
 ( 4, 2, 2, 2, 2, 4 ),
 ( 1.205172527016783068E-17, 9.147187684556683674E-05, 0.0001829437536911216388, 0.0003658875073822308093, 0.0007317750147644532703, 0.001463550029528898518 ),
 .UNSPECIFIED. ) ;
#19468 = FACE_OUTER_BOUND ( 'NONE', #8650, .T. ) ;
#19469 = CARTESIAN_POINT ( 'NONE',  ( 10.00000000000000000, 0.6226916219172712319, -4.971152295393295617 ) ) ;
#19470 = ORIENTED_EDGE ( 'NONE', *, *, #8358, .F. ) ;
#19471 = CARTESIAN_POINT ( 'NONE',  ( 2.661997627134198297, -6.664939678585230176, 7.629706518865833509 ) ) ;
#19472 = DIRECTION ( 'NONE',  ( 0.000000000000000000, 1.000000000000000000, 0.000000000000000000 ) ) ;
#19473 = CC_DESIGN_SECURITY_CLASSIFICATION ( #26402, ( #33099 ) ) ;
#19474 = EDGE_LOOP ( 'NONE', ( #3332, #16052, #26706 ) ) ;
#19475 = CARTESIAN_POINT ( 'NONE',  ( 8.030511337664275828, -2.816904086294465870, 0.9999999999999997780 ) ) ;
#19476 = ORIENTED_EDGE ( 'NONE', *, *, #17111, .T. ) ;
#19477 = ADVANCED_FACE ( 'NONE', ( #32846 ), #26282, .T. ) ;
#19478 = ORIENTED_EDGE ( 'NONE', *, *, #32087, .T. ) ;
#19479 = DIRECTION ( 'NONE',  ( 0.000000000000000000, 0.000000000000000000, -1.000000000000000000 ) ) ;
#19481 = VERTEX_POINT ( 'NONE', #20942 ) ;
#19480 = DIRECTION ( 'NONE',  ( 0.000000000000000000, 0.000000000000000000, 1.000000000000000000 ) ) ;
#19482 = VERTEX_POINT ( 'NONE', #2734 ) ;
#19483 = CARTESIAN_POINT ( 'NONE',  ( 22.54750000136559507, 3.024605502323846729, -0.3178988483021056854 ) ) ;
#19484 = ORIENTED_EDGE ( 'NONE', *, *, #22846, .T. ) ;
#19485 = DIRECTION ( 'NONE',  ( -0.000000000000000000, -0.000000000000000000, -1.000000000000000000 ) ) ;
#19486 = FACE_OUTER_BOUND ( 'NONE', #17410, .T. ) ;
#19487 = AXIS2_PLACEMENT_3D ( 'NONE', #32795, #30125, #27241 ) ;
#19489 = ORIENTED_EDGE ( 'NONE', *, *, #18207, .F. ) ;
#19488 = DIRECTION ( 'NONE',  ( 1.000000000000000000, -8.574039729943018344E-17, -0.000000000000000000 ) ) ;
#19490 = CYLINDRICAL_SURFACE ( 'NONE', #2844, 5.010000000000000675 ) ;
#19491 = CARTESIAN_POINT ( 'NONE',  ( -56.45356511950618028, 0.03062438154691659795, -1.016704686750477649 ) ) ;
#19492 = CARTESIAN_POINT ( 'NONE',  ( 6.530491482054472385, 0.8857639883442899320, 8.615020591497804858 ) ) ;
#19493 = CARTESIAN_POINT ( 'NONE',  ( 1.147381204815054234, 0.5174497483512505713, -7.899033294795724025 ) ) ;
#19494 = EDGE_CURVE ( 'NONE', #8558, #9572, #32246, .T. ) ;
#19495 = ADVANCED_FACE ( 'NONE', ( #20281 ), #15693, .F. ) ;
#19496 = CARTESIAN_POINT ( 'NONE',  ( 23.61221640758335027, -8.051464822112823327, -0.07017451552783526836 ) ) ;
#19497 = DIRECTION ( 'NONE',  ( 0.000000000000000000, 0.000000000000000000, 1.000000000000000000 ) ) ;
#19498 = CARTESIAN_POINT ( 'NONE',  ( 108.3696618535068126, 20.23658298680886247, -1.378742097822665436 ) ) ;
#19499 = CARTESIAN_POINT ( 'NONE',  ( 25.75999999999999801, -2.208672634433321348E-15, 0.000000000000000000 ) ) ;
#19500 = CARTESIAN_POINT ( 'NONE',  ( 10.00000000000000178, -8.574039729943018837E-16, 0.000000000000000000 ) ) ;
#19501 = CARTESIAN_POINT ( 'NONE',  ( 0.7632845268398871230, -2.223716399045513548, -8.461683424509338636 ) ) ;
#19502 = CARTESIAN_POINT ( 'NONE',  ( -6.950050802731187360, 0.3135853898029611342, -2.983565686104819648 ) ) ;
#19503 = ORIENTED_EDGE ( 'NONE', *, *, #7386, .F. ) ;
#19504 = CARTESIAN_POINT ( 'NONE',  ( -3.900050800000000706, -2.983565686104819648, -0.3135853898029605791 ) ) ;
#19505 = DIRECTION ( 'NONE',  ( 0.2880220749472531261, 0.1662896225033516084, -0.9430753128943477614 ) ) ;
#19506 = DIRECTION ( 'NONE',  ( 0.000000000000000000, -1.000000000000000000, 0.000000000000000000 ) ) ;
#19507 = LINE ( 'NONE', #16970, #17271 ) ;
#19508 = ORIENTED_EDGE ( 'NONE', *, *, #21152, .F. ) ;
#19509 = PLANE ( 'NONE',  #10662 ) ;
#19510 = CARTESIAN_POINT ( 'NONE',  ( 17.05941372759221153, -15.60161612857906910, -1.500000000000001110 ) ) ;
#19511 = VERTEX_POINT ( 'NONE', #17771 ) ;
#19512 = CARTESIAN_POINT ( 'NONE',  ( 0.5363866353863503411, -4.520465117293254842, 1.500000000000034861 ) ) ;
#19513 = PERSON_AND_ORGANIZATION_ROLE ( 'creator' ) ;
#19514 = FACE_OUTER_BOUND ( 'NONE', #9643, .T. ) ;
#19515 = EDGE_LOOP ( 'NONE', ( #14813, #31915, #27946 ) ) ;
#19516 = CARTESIAN_POINT ( 'NONE',  ( -4.075753277656722240, -9.746161035319881094, 1.499999999999999778 ) ) ;
#19517 = CARTESIAN_POINT ( 'NONE',  ( 12.16477365892661489, 4.794553353644049665, -1.050000000000000044 ) ) ;
#19518 = CARTESIAN_POINT ( 'NONE',  ( 102.4077201195266440, -3.775001509843904479, -4.215290384275154345 ) ) ;
#19519 = CARTESIAN_POINT ( 'NONE',  ( 24.43445557112633892, -17.40480440763370495, -1.396984404749928022 ) ) ;
#19520 = CARTESIAN_POINT ( 'NONE',  ( 25.75999999999999801, -2.208672634433321348E-15, 0.000000000000000000 ) ) ;
#19521 = EDGE_LOOP ( 'NONE', ( #18039, #16257, #26076 ) ) ;
#19522 = EDGE_CURVE ( 'NONE', #1245, #24117, #28634, .T. ) ;
#19523 = CARTESIAN_POINT ( 'NONE',  ( 0.000000000000000000, -0.5000000000000000000, 1.000000000000000000 ) ) ;
#19524 = CARTESIAN_POINT ( 'NONE',  ( 107.7536796087345294, 16.80655079293032017, 1.395761063491601783 ) ) ;
#19525 = DIRECTION ( 'NONE',  ( 1.000000000000000000, -0.000000000000000000, 0.000000000000000000 ) ) ;
#19526 = EDGE_CURVE ( 'NONE', #15360, #18631, #23434, .T. ) ;
#19528 = ORIENTED_EDGE ( 'NONE', *, *, #15129, .T. ) ;
#19527 = DIRECTION ( 'NONE',  ( 8.672736310388503609E-16, 0.000000000000000000, 1.000000000000000000 ) ) ;
#19529 = CARTESIAN_POINT ( 'NONE',  ( -23.35000000000000142, -10.96966150227469505, 4.000000000000000000 ) ) ;
#19530 = CARTESIAN_POINT ( 'NONE',  ( -2.223027892448373510, -2.927336879246196677, -4.522129901861166701 ) ) ;
#19531 = CARTESIAN_POINT ( 'NONE',  ( 1.624999999999999778, 5.222868219166857173, 9.680994141368792327 ) ) ;
#19532 = DIRECTION ( 'NONE',  ( 0.000000000000000000, -0.9271838545667856479, -0.3746065934159163446 ) ) ;
#19533 = DIRECTION ( 'NONE',  ( -0.000000000000000000, -0.000000000000000000, 1.000000000000000000 ) ) ;
#19534 = CARTESIAN_POINT ( 'NONE',  ( 25.11449300058561462, -17.48310186013782896, -1.186355288471905300 ) ) ;
#19535 = DIRECTION ( 'NONE',  ( 0.000000000000000000, -0.4226182617407089337, 0.9063077870366456068 ) ) ;
#19536 = CARTESIAN_POINT ( 'NONE',  ( -30.16981175037142293, 11.66754487082764236, 1.941331850688031491 ) ) ;
#19537 = ORIENTED_EDGE ( 'NONE', *, *, #32082, .T. ) ;
#19538 = CARTESIAN_POINT ( 'NONE',  ( -56.32100375116784363, 0.5246615022747116441, -1.500000000000000000 ) ) ;
#19539 = ORIENTED_EDGE ( 'NONE', *, *, #27021, .T. ) ;
#19540 = CARTESIAN_POINT ( 'NONE',  ( -6.654531657079158613, 2.846291840500173365, 1.545410377633946952 ) ) ;
#19541 = LINE ( 'NONE', #4652, #17727 ) ;
#19542 = CARTESIAN_POINT ( 'NONE',  ( 18.93617721851659041, -3.890633339435721982, -4.522129901861162260 ) ) ;
#19543 = CARTESIAN_POINT ( 'NONE',  ( 109.3993806922052840, 20.31298924473512457, -2.334455007174283558 ) ) ;
#19544 = CARTESIAN_POINT ( 'NONE',  ( 35.27668332986760191, -7.991339570345005860, 1.873789188799038774 ) ) ;
#19545 = EDGE_LOOP ( 'NONE', ( #17571, #28139, #26817, #2736, #5879, #11186, #13474, #7806, #12255, #23509 ) ) ;
#19546 = CARTESIAN_POINT ( 'NONE',  ( 108.0068349480237373, 18.21621961241920573, -4.398253369385428435 ) ) ;
#19547 = ORIENTED_EDGE ( 'NONE', *, *, #19572, .F. ) ;
#19548 = DATE_AND_TIME ( #32428, #1790 ) ;
#19549 = CARTESIAN_POINT ( 'NONE',  ( 18.75915348114306269, -5.869403441360198315, 4.008637382310625163 ) ) ;
#19550 = EDGE_CURVE ( 'NONE', #3413, #4708, #14709, .T. ) ;
#19551 = CARTESIAN_POINT ( 'NONE',  ( 8.770293993838562230, -1.124525571980899086, -0.9999999999999997780 ) ) ;
#19552 = FACE_OUTER_BOUND ( 'NONE', #18876, .T. ) ;
#19553 = ORIENTED_EDGE ( 'NONE', *, *, #24186, .T. ) ;
#19554 = EDGE_LOOP ( 'NONE', ( #31931, #2494, #18720 ) ) ;
#19555 = CARTESIAN_POINT ( 'NONE',  ( 0.7632845268398876781, -0.4999240074893807617, -8.734705317681624948 ) ) ;
#19556 = CARTESIAN_POINT ( 'NONE',  ( -2.662550801365593411, -3.521866450007987037, -0.3701630799359323931 ) ) ;
#19557 = EDGE_CURVE ( 'NONE', #15820, #4283, #18935, .T. ) ;
#19558 = CARTESIAN_POINT ( 'NONE',  ( 24.29749999999999943, -0.7685399846772070775, 2.594547506269381465 ) ) ;
#19559 = CARTESIAN_POINT ( 'NONE',  ( 0.7770785076403996516, -9.232944038193473091, -1.768683507966675617 ) ) ;
#19561 = VERTEX_POINT ( 'NONE', #29271 ) ;
#19560 = CARTESIAN_POINT ( 'NONE',  ( 6.524595551582239139, 3.779376390944578556, -7.790581746767696991 ) ) ;
#19562 = CARTESIAN_POINT ( 'NONE',  ( -3.537550801365593411, -3.368539882008727115, -1.828967928396028064 ) ) ;
#19563 = CYLINDRICAL_SURFACE ( 'NONE', #30484, 0.4499999999999990119 ) ;
#19564 = EDGE_CURVE ( 'NONE', #12129, #18566, #20709, .T. ) ;
#19565 = DIRECTION ( 'NONE',  ( -1.000000000000000000, -0.000000000000000000, 0.000000000000000000 ) ) ;
#19566 = FACE_BOUND ( 'NONE', #25264, .T. ) ;
#19567 = VERTEX_POINT ( 'NONE', #21600 ) ;
#19569 = VERTEX_POINT ( 'NONE', #31639 ) ;
#19568 = CARTESIAN_POINT ( 'NONE',  ( 3.285054055080412816, -2.054325274013051460E-30, 1.174876329418460541 ) ) ;
#19570 = CARTESIAN_POINT ( 'NONE',  ( 16.66046955005661800, 12.69976583513764012, 1.500000000000000000 ) ) ;
#19571 = CARTESIAN_POINT ( 'NONE',  ( 25.75999999999999801, -2.208672634433321348E-15, -2.499999999999997780 ) ) ;
#19572 = EDGE_CURVE ( 'NONE', #2424, #19481, #13566, .T. ) ;
#19573 = CARTESIAN_POINT ( 'NONE',  ( 24.61000000136559152, 2.892927487894327410, -1.570731468192931635 ) ) ;
#19574 = CARTESIAN_POINT ( 'NONE',  ( -25.33158220408985883, 18.40448632064655499, 1.499999999999999778 ) ) ;
#19575 = CARTESIAN_POINT ( 'NONE',  ( -4.154892416117755616, -6.512770286199655700, -1.745058604112273981 ) ) ;
#19576 = FACE_OUTER_BOUND ( 'NONE', #9925, .T. ) ;
#19577 = EDGE_CURVE ( 'NONE', #19954, #8466, #26763, .T. ) ;
#19578 = FACE_OUTER_BOUND ( 'NONE', #5590, .T. ) ;
#19579 = CARTESIAN_POINT ( 'NONE',  ( -2.687550801365593323, -2.228590825266444586, -2.752080473201636401 ) ) ;
#19580 = ORIENTED_EDGE ( 'NONE', *, *, #13422, .T. ) ;
#19581 = DIRECTION ( 'NONE',  ( -0.000000000000000000, -0.000000000000000000, -1.000000000000000000 ) ) ;
#19582 = VERTEX_POINT ( 'NONE', #13871 ) ;
#19583 = CARTESIAN_POINT ( 'NONE',  ( 0.000000000000000000, 1.464956435139539659, 10.90201369670498899 ) ) ;
#19584 = EDGE_CURVE ( 'NONE', #5778, #10585, #27081, .T. ) ;
#19585 = CARTESIAN_POINT ( 'NONE',  ( 0.000000000000000000, 0.000000000000000000, 0.000000000000000000 ) ) ;
#19586 = CARTESIAN_POINT ( 'NONE',  ( 108.8978791464556508, 17.52043075494136204, 4.999054092451758358 ) ) ;
#19587 = DIRECTION ( 'NONE',  ( 1.000000000000000000, -0.000000000000000000, -0.000000000000000000 ) ) ;
#19588 = ORIENTED_EDGE ( 'NONE', *, *, #30787, .F. ) ;
#19589 = CARTESIAN_POINT ( 'NONE',  ( 10.52034268205830614, -3.672404558090062832, 3.407865132560167432 ) ) ;
#19590 = ORIENTED_EDGE ( 'NONE', *, *, #13624, .F. ) ;
#19591 = CARTESIAN_POINT ( 'NONE',  ( 7.249760686538667009, 5.151476664237477188, 6.139290821770273077 ) ) ;
#19593 = ORIENTED_EDGE ( 'NONE', *, *, #32476, .F. ) ;
#19592 = CARTESIAN_POINT ( 'NONE',  ( 54.94552861322679149, -5.361349067125541268, -3.996604662717867740 ) ) ;
#19594 = ORIENTED_EDGE ( 'NONE', *, *, #25129, .T. ) ;
#19595 = EDGE_CURVE ( 'NONE', #23529, #29856, #11555, .T. ) ;
#19596 = EDGE_CURVE ( 'NONE', #16296, #10256, #7149, .T. ) ;
#19597 = CARTESIAN_POINT ( 'NONE',  ( 5.612974441954674987, 5.432722698947240580, -6.163896661468919014 ) ) ;
#19598 = CARTESIAN_POINT ( 'NONE',  ( 48.08400536259535585, -8.675012021211061963, -2.713652344655542059 ) ) ;
#19600 = VERTEX_POINT ( 'NONE', #21264 ) ;
#19599 = CARTESIAN_POINT ( 'NONE',  ( 0.5282775464098437013, -15.74330118545617552, -1.499999999999998890 ) ) ;
#19601 = CARTESIAN_POINT ( 'NONE',  ( 5.489344046532323773, 4.149088721182530470, 6.978601450725500754 ) ) ;
#19602 = CARTESIAN_POINT ( 'NONE',  ( 10.57125986779756843, 0.8254815157535241310, 4.681538312723519724 ) ) ;
#19603 = DIRECTION ( 'NONE',  ( 0.000000000000000000, 1.000000000000000000, 0.000000000000000000 ) ) ;
#19604 = CARTESIAN_POINT ( 'NONE',  ( 3.063284526839890720, 8.461683424509336859, -2.223716399045483794 ) ) ;
#19605 = ADVANCED_FACE ( 'NONE', ( #26606 ), #31805, .F. ) ;
#19607 = ORIENTED_EDGE ( 'NONE', *, *, #917, .T. ) ;
#19606 = CARTESIAN_POINT ( 'NONE',  ( 107.9934725388863939, -17.97536830041021005, -4.591573371172586349 ) ) ;
#19608 = DIRECTION ( 'NONE',  ( 0.000000000000000000, 1.000000000000000000, 0.000000000000000000 ) ) ;
#19609 = CARTESIAN_POINT ( 'NONE',  ( 6.530491627857225367, -2.368289848745700699, -8.330327812606284965 ) ) ;
#19610 = CARTESIAN_POINT ( 'NONE',  ( 3.499999999999999556, 5.241389472434663688, 4.711457988287072851 ) ) ;
#19611 = DIRECTION ( 'NONE',  ( -0.000000000000000000, 0.000000000000000000, 1.000000000000000000 ) ) ;
#19612 = EDGE_CURVE ( 'NONE', #29154, #256, #30304, .T. ) ;
#19613 = CARTESIAN_POINT ( 'NONE',  ( 3.499999999999999556, -7.009698679648292519, 3.730838147389666126 ) ) ;
#19614 = CARTESIAN_POINT ( 'NONE',  ( 12.40148790557316794, 21.49000000000003041, 1.500000000000000000 ) ) ;
#19615 = ORIENTED_EDGE ( 'NONE', *, *, #14012, .T. ) ;
#19616 = CARTESIAN_POINT ( 'NONE',  ( 6.038145208238977268, -4.620191422127173375, 7.104833038995700178 ) ) ;
#19617 = CARTESIAN_POINT ( 'NONE',  ( -15.35000000000000320, -10.96966150227469505, 4.000000000000000000 ) ) ;
#19618 = DIRECTION ( 'NONE',  ( 3.410983854926731543E-15, 1.734723475976805714E-15, -1.000000000000000000 ) ) ;
#19619 = ORIENTED_EDGE ( 'NONE', *, *, #12415, .T. ) ;
#19620 = ADVANCED_FACE ( 'NONE', ( #5873 ), #31463, .T. ) ;
#19621 = CARTESIAN_POINT ( 'NONE',  ( 25.75999999999999801, -2.208672634433321348E-15, 0.000000000000000000 ) ) ;
#19622 = CYLINDRICAL_SURFACE ( 'NONE', #9255, 0.5000000000000004441 ) ;
#19623 = VERTEX_POINT ( 'NONE', #26292 ) ;
#19624 = CARTESIAN_POINT ( 'NONE',  ( 7.274195578026668052, -5.507181329334641440, 1.000000000000000000 ) ) ;
#19625 = EDGE_CURVE ( 'NONE', #33011, #6174, #26461, .T. ) ;
#19626 = ORIENTED_EDGE ( 'NONE', *, *, #17508, .T. ) ;
#19627 = ORIENTED_EDGE ( 'NONE', *, *, #381, .F. ) ;
#19628 = CARTESIAN_POINT ( 'NONE',  ( -2.837798564937276335, -0.5311976243150138277, 1.513817338014894265 ) ) ;
#19629 = COORDINATED_UNIVERSAL_TIME_OFFSET ( 0, 0, .AHEAD. ) ;
#19631 = EDGE_LOOP ( 'NONE', ( #21798, #31322, #18535, #8156, #11067, #4268, #30535, #21041, #19373, #23717, #8023, #9713 ) ) ;
#19630 = DIRECTION ( 'NONE',  ( 1.000000000000000000, 0.000000000000000000, 0.000000000000000000 ) ) ;
#19632 = VERTEX_POINT ( 'NONE', #3708 ) ;
#19633 = CARTESIAN_POINT ( 'NONE',  ( 22.98500000136559862, -2.892927487894331406, 1.570731468192932523 ) ) ;
#19634 = EDGE_CURVE ( 'NONE', #29013, #31514, #2498, .T. ) ;
#19635 = EDGE_CURVE ( 'NONE', #31221, #16905, #28800, .T. ) ;
#19636 = B_SPLINE_CURVE_WITH_KNOTS ( 'NONE', 3,
 ( #19955, #2401, #24788, #21936, #9398, #24596, #22278, #17069 ),
 .UNSPECIFIED., .F., .F.,
 ( 4, 2, 2, 4 ),
 ( 2.197717205396726239E-07, 0.001262070444981970444, 0.001892995781612686430, 0.002523921118243402199 ),
 .UNSPECIFIED. ) ;
#19637 = VERTEX_POINT ( 'NONE', #32316 ) ;
#19638 = CARTESIAN_POINT ( 'NONE',  ( -3.671580638170519912E-13, 9.620177616658855513, 5.227991826304058343 ) ) ;
#19639 = CARTESIAN_POINT ( 'NONE',  ( 74.30107678963170770, -22.79527490385382649, 1.500000000000000000 ) ) ;
#19641 = VERTEX_POINT ( 'NONE', #32129 ) ;
#19640 = CARTESIAN_POINT ( 'NONE',  ( 84.88357813086332726, -2.741221277473834483, -1.873788409403105426 ) ) ;
#19642 = DIRECTION ( 'NONE',  ( -1.000000000000000000, -0.000000000000000000, -0.000000000000000000 ) ) ;
#19643 = B_SPLINE_CURVE_WITH_KNOTS ( 'NONE', 3,
 ( #13709, #11828, #24871, #31620, #8380, #28767, #5303, #9982 ),
 .UNSPECIFIED., .F., .F.,
 ( 4, 2, 2, 4 ),
 ( 0.009524646911531405372, 0.5047623234557655492, 0.7523811617278827191, 1.000000000000000000 ),
 .UNSPECIFIED. ) ;
#19644 = B_SPLINE_CURVE_WITH_KNOTS ( 'NONE', 3,
 ( #865, #18234, #28447, #6029, #31135, #18910, #23572, #5557, #3377, #11044, #21242, #31440, #26442, #3541, #23901, #14193, #4172, #21578 ),
 .UNSPECIFIED., .F., .F.,
 ( 4, 2, 2, 2, 2, 2, 2, 2, 4 ),
 ( 0.000000000000000000, 0.003093832034890393878, 0.006187664069780787757, 0.009281496104671181635, 0.01237532813956157551, 0.01546916017445196939, 0.01856299220934236327, 0.02165682424423275715, 0.02475065627912315103 ),
 .UNSPECIFIED. ) ;
#19645 = CARTESIAN_POINT ( 'NONE',  ( 3.249999999999999556, 8.475820894093034852, -4.057423117305301474 ) ) ;
#19646 = CARTESIAN_POINT ( 'NONE',  ( 25.04750000136559507, -3.024605502323851169, 0.3178988483021052969 ) ) ;
#19647 = CARTESIAN_POINT ( 'NONE',  ( 108.0633640349754359, -18.98178845727616704, 3.316617650393312466 ) ) ;
#19648 =( BOUNDED_SURFACE ( )  B_SPLINE_SURFACE ( 3, 3, ( 
 ( #8764, #6244, #4085, #3446 ),
 ( #11264, #13912, #21470, #26807 ),
 ( #26494, #24302, #3928, #11591 ),
 ( #769, #1254, #16428, #10952 ) ),
 .UNSPECIFIED., .F., .F., .F. ) 
 B_SPLINE_SURFACE_WITH_KNOTS ( ( 4, 4 ),
 ( 4, 4 ),
 ( 0.000000000000000000, 1.000000000000000000 ),
 ( 0.000000000000000000, 1.000000000000000000 ),
 .UNSPECIFIED. ) 
 GEOMETRIC_REPRESENTATION_ITEM ( )  RATIONAL_B_SPLINE_SURFACE ( (
 ( 1.000000000000000000, 0.9917560313531952332, 0.9917560313531952332, 1.000000000000000000),
 ( 0.6539698177806696489, 0.6485785111069292119, 0.6485785111069292119, 0.6539698177806696489),
 ( 0.6539698177806696489, 0.6485785111069292119, 0.6485785111069292119, 0.6539698177806696489),
 ( 1.000000000000000000, 0.9917560313531952332, 0.9917560313531952332, 1.000000000000000000) ) ) 
 REPRESENTATION_ITEM ( '' )  SURFACE ( )  );
#19649 = CARTESIAN_POINT ( 'NONE',  ( 46.69789307159569347, 25.15383447853596621, -4.612695725900422872 ) ) ;
#19650 = CARTESIAN_POINT ( 'NONE',  ( 3.499999999999999556, -1.471047635026914380, 6.892461014225956362 ) ) ;
#19651 = DIRECTION ( 'NONE',  ( 1.000000000000000000, -8.574039729943018344E-17, -0.000000000000000000 ) ) ;
#19652 = EDGE_CURVE ( 'NONE', #14402, #11109, #23456, .T. ) ;
#19653 = DIRECTION ( 'NONE',  ( -1.000000000000000000, -0.000000000000000000, -0.000000000000000000 ) ) ;
#19654 = CARTESIAN_POINT ( 'NONE',  ( -5.772270645472310946, 14.99679128811752804, -2.402751277358635473 ) ) ;
#19655 = DIRECTION ( 'NONE',  ( -1.000000000000000000, 0.000000000000000000, 0.000000000000000000 ) ) ;
#19656 = B_SPLINE_CURVE_WITH_KNOTS ( 'NONE', 3,
 ( #4909, #25310, #11065, #31318, #10730, #26294, #18443, #23923, #31162, #3404 ),
 .UNSPECIFIED., .F., .F.,
 ( 4, 2, 2, 2, 4 ),
 ( 0.000000000000000000, 0.0002027905827773804999, 0.0004055811655547609997, 0.0006083717483321414996, 0.0008111623311095219994 ),
 .UNSPECIFIED. ) ;
#19657 = LINE ( 'NONE', #22319, #23079 ) ;
#19658 = CARTESIAN_POINT ( 'NONE',  ( -4.400050802731188426, 3.113457007523260156, -0.9222479816126439855 ) ) ;
#19659 = ORIENTED_EDGE ( 'NONE', *, *, #24827, .F. ) ;
#19660 = CARTESIAN_POINT ( 'NONE',  ( -3.400050800000000262, 1.887961173149511618, 2.331437884370912705 ) ) ;
#19661 = CYLINDRICAL_SURFACE ( 'NONE', #29556, 4.000000000000001776 ) ;
#19662 = CARTESIAN_POINT ( 'NONE',  ( -4.112942406915325755, -5.022711880624455567E-15, 2.999999999999999556 ) ) ;
#19663 = VERTEX_POINT ( 'NONE', #12061 ) ;
#19664 = CARTESIAN_POINT ( 'NONE',  ( 8.528645601772334217, -0.5000000000000000000, -1.500000000000000000 ) ) ;
#19665 = EDGE_CURVE ( 'NONE', #29352, #23090, #25612, .T. ) ;
#19666 = ORIENTED_EDGE ( 'NONE', *, *, #13751, .T. ) ;
#19667 = CARTESIAN_POINT ( 'NONE',  ( 19.74808449209627526, -17.01894530462115540, 1.753250788838565777 ) ) ;
#19668 = ADVANCED_FACE ( 'NONE', ( #32924 ), #929, .T. ) ;
#19669 = PERSON_AND_ORGANIZATION_ROLE ( 'creator' ) ;
#19670 = CARTESIAN_POINT ( 'NONE',  ( -2.800050800000000173, 2.331437884370912705, -1.887961173149511618 ) ) ;
#19671 = EDGE_LOOP ( 'NONE', ( #20828, #12434, #17449, #30356 ) ) ;
#19672 = CARTESIAN_POINT ( 'NONE',  ( 18.86054332783663767, -4.736068442360260811, 3.993434336035622589 ) ) ;
#19673 = CARTESIAN_POINT ( 'NONE',  ( 17.41555300807529250, 12.90381744129215669, -1.050000000000000044 ) ) ;
#19674 = CARTESIAN_POINT ( 'NONE',  ( 85.03579748203488009, -5.204477564382398391, -3.993433529979800056 ) ) ;
#19675 = PLANE ( 'NONE',  #24066 ) ;
#19676 = CARTESIAN_POINT ( 'NONE',  ( 0.000000000000000000, 0.000000000000000000, 0.000000000000000000 ) ) ;
#19677 = VERTEX_POINT ( 'NONE', #11899 ) ;
#19678 = DIRECTION ( 'NONE',  ( 0.000000000000000000, 0.000000000000000000, 1.000000000000000000 ) ) ;
#19679 = CARTESIAN_POINT ( 'NONE',  ( 23.03032540518322335, -21.91564990537378321, -1.226001752879117168 ) ) ;
#19680 = LINE ( 'NONE', #30058, #10833 ) ;
#19682 = EDGE_LOOP ( 'NONE', ( #16079, #432, #2073, #25858 ) ) ;
#19681 = CARTESIAN_POINT ( 'NONE',  ( 3.063284526839887167, -8.461683424509331530, 2.223716399045538861 ) ) ;
#19683 = CARTESIAN_POINT ( 'NONE',  ( 5.377543748152548986, -8.014274990069656823, 8.669741416787380218E-17 ) ) ;
#19684 = DIRECTION ( 'NONE',  ( 1.734547262077700722E-15, 0.000000000000000000, 1.000000000000000000 ) ) ;
#19685 = LINE ( 'NONE', #14665, #11867 ) ;
#19686 = DIRECTION ( 'NONE',  ( 0.000000000000000000, 0.000000000000000000, 1.000000000000000000 ) ) ;
#19687 = DIRECTION ( 'NONE',  ( -0.000000000000000000, -0.000000000000000000, -1.000000000000000000 ) ) ;
#19688 = CARTESIAN_POINT ( 'NONE',  ( 7.064423539573518873, 0.7071067811875524356, 8.721381771257245674 ) ) ;
#19689 = LINE ( 'NONE', #9638, #28408 ) ;
#19690 = DIRECTION ( 'NONE',  ( -1.000000000000000000, 0.000000000000000000, -0.000000000000000000 ) ) ;
#19691 = CARTESIAN_POINT ( 'NONE',  ( -25.97738183003427537, 4.497411454590747759, 2.132333938606539636 ) ) ;
#19692 = ORIENTED_EDGE ( 'NONE', *, *, #2301, .F. ) ;
#19693 = CARTESIAN_POINT ( 'NONE',  ( 6.530491627857225367, 2.368289848745754878, 8.330327812606270754 ) ) ;
#19694 = ORIENTED_EDGE ( 'NONE', *, *, #8796, .F. ) ;
#19695 = CARTESIAN_POINT ( 'NONE',  ( -6.154531657079158613, -0.9198621039125872700, -3.105402419394638791 ) ) ;
#19696 = CARTESIAN_POINT ( 'NONE',  ( -2.593512329575616979E-16, -3.024842911000663381, -3.993798362933340229 ) ) ;
#19697 = DIRECTION ( 'NONE',  ( 0.000000000000000000, 0.000000000000000000, -1.000000000000000000 ) ) ;
#19698 = LINE ( 'NONE', #19875, #14578 ) ;
#19699 = CARTESIAN_POINT ( 'NONE',  ( -47.64323377349501243, 16.45499999999998408, 1.500000000000000000 ) ) ;
#19700 = ORIENTED_EDGE ( 'NONE', *, *, #23899, .F. ) ;
#19701 = EDGE_CURVE ( 'NONE', #20949, #33059, #27889, .T. ) ;
#19702 = CARTESIAN_POINT ( 'NONE',  ( 1.624999999999999778, -10.82112760146734765, -1.975651141462353655 ) ) ;
#19703 = EDGE_CURVE ( 'NONE', #6604, #17238, #5003, .T. ) ;
#19704 = ORIENTED_EDGE ( 'NONE', *, *, #10267, .T. ) ;
#19705 = EDGE_CURVE ( 'NONE', #32002, #7398, #24766, .T. ) ;
#19706 = MECHANICAL_CONTEXT ( 'NONE', #520, 'mechanical' ) ;
#19707 = CARTESIAN_POINT ( 'NONE',  ( 69.07029661791293051, -6.113298883570701392, 3.998506773566581352 ) ) ;
#19708 = CARTESIAN_POINT ( 'NONE',  ( 0.000000000000000000, -5.222868219166924675, 9.680994141368749695 ) ) ;
#19709 = AXIS2_PLACEMENT_3D ( 'NONE', #31370, #31042, #28688 ) ;
#19711 = LINE ( 'NONE', #20063, #16106 ) ;
#19710 = CARTESIAN_POINT ( 'NONE',  ( 107.1772993348646281, 16.40207914262226296, -1.491740999229418829 ) ) ;
#19712 = VERTEX_POINT ( 'NONE', #29628 ) ;
#19713 = CARTESIAN_POINT ( 'NONE',  ( 0.7632845268458183785, 8.152713396062706508, 3.174628368984090176 ) ) ;
#19714 = CARTESIAN_POINT ( 'NONE',  ( -2.562550801365592879, -2.228590825266444586, -2.752080473201636401 ) ) ;
#19715 = CARTESIAN_POINT ( 'NONE',  ( 24.79749999999999943, 0.7685399846772009713, -2.594547506269381909 ) ) ;
#19716 = CARTESIAN_POINT ( 'NONE',  ( 4.773718314179047795, -12.83538324571378375, -1.756822410893565278 ) ) ;
#19718 = ORIENTED_EDGE ( 'NONE', *, *, #14697, .T. ) ;
#19717 = CARTESIAN_POINT ( 'NONE',  ( 25.43628654896178176, -17.54453578616395149, 1.000000000000000000 ) ) ;
#19719 = CARTESIAN_POINT ( 'NONE',  ( -4.137550801365594388, 1.828967928396027176, -3.368539882008727115 ) ) ;
#19720 = CARTESIAN_POINT ( 'NONE',  ( 3.499999999999999556, -6.700937042937042065, -2.183447440113257976 ) ) ;
#19721 = DIRECTION ( 'NONE',  ( -0.1385137909583552540, 0.9903605049245174374, 0.000000000000000000 ) ) ;
#19722 = CARTESIAN_POINT ( 'NONE',  ( 3.063284526839887167, 0.000000000000000000, 0.000000000000000000 ) ) ;
#19723 = VERTEX_POINT ( 'NONE', #19586 ) ;
#19725 = ORIENTED_EDGE ( 'NONE', *, *, #1663, .F. ) ;
#19724 = DIRECTION ( 'NONE',  ( -1.000000000000000000, 0.000000000000000000, 0.000000000000000000 ) ) ;
#19726 = AXIS2_PLACEMENT_3D ( 'NONE', #8744, #18950, #29141 ) ;
#19727 = CARTESIAN_POINT ( 'NONE',  ( 11.15780064305207908, 3.972637044352831381, 1.500000000000000222 ) ) ;
#19728 = DIRECTION ( 'NONE',  ( 0.000000000000000000, 0.000000000000000000, 1.000000000000000000 ) ) ;
#19729 = CARTESIAN_POINT ( 'NONE',  ( 24.42250000136559507, -0.3178988483021076838, -3.024605502323848949 ) ) ;
#19730 = CARTESIAN_POINT ( 'NONE',  ( -29.44915099269499947, 14.89308641508704412, 1.500000000000740297 ) ) ;
#19731 = CARTESIAN_POINT ( 'NONE',  ( 11.72335232094827440, -20.06224895199573410, -1.500000000000938583 ) ) ;
#19732 = EDGE_CURVE ( 'NONE', #26130, #12480, #29784, .T. ) ;
#19733 = PLANE ( 'NONE',  #2884 ) ;
#19734 = CARTESIAN_POINT ( 'NONE',  ( 68.95644445485396545, -3.844730188642862423, 2.184957270839068322 ) ) ;
#19735 = CARTESIAN_POINT ( 'NONE',  ( 107.3476768466315008, -15.88628154573193463, 1.499999999999999778 ) ) ;
#19736 = ORIENTED_EDGE ( 'NONE', *, *, #22219, .T. ) ;
#19737 = CARTESIAN_POINT ( 'NONE',  ( 101.6895021285839391, -2.427391549943337612, 3.236220879366405789 ) ) ;
#19738 = ORIENTED_EDGE ( 'NONE', *, *, #20448, .F. ) ;
#19739 = AXIS2_PLACEMENT_3D ( 'NONE', #5445, #10457, #2969 ) ;
#19740 = VECTOR ( 'NONE', #3753, 1000.000000000000000 ) ;
#19741 = DIRECTION ( 'NONE',  ( 0.000000000000000000, 1.000000000000000000, 0.000000000000000000 ) ) ;
#19742 = LINE ( 'NONE', #15223, #70 ) ;
#19743 = ORIENTED_EDGE ( 'NONE', *, *, #19013, .F. ) ;
#19744 = VECTOR ( 'NONE', #32864, 1000.000000000000227 ) ;
#19745 = CARTESIAN_POINT ( 'NONE',  ( 17.33093461831347781, -21.43932300456618378, 1.500000000000000000 ) ) ;
#19746 = ORIENTED_EDGE ( 'NONE', *, *, #327, .T. ) ;
#19747 = FACE_OUTER_BOUND ( 'NONE', #19398, .T. ) ;
#19749 = ORIENTED_EDGE ( 'NONE', *, *, #17978, .F. ) ;
#19748 = CARTESIAN_POINT ( 'NONE',  ( 28.69351768328725782, -5.618942245713509642, -3.998506281427256948 ) ) ;
#19750 = ORIENTED_EDGE ( 'NONE', *, *, #25518, .T. ) ;
#19751 = DIRECTION ( 'NONE',  ( -0.9896144216807901683, 0.000000000000000000, -0.1437473352845036190 ) ) ;
#19752 = CARTESIAN_POINT ( 'NONE',  ( 41.43141396789280151, -2.886852813799071438, 0.07017451552782173751 ) ) ;
#19754 = ORIENTED_EDGE ( 'NONE', *, *, #12047, .F. ) ;
#19753 = CARTESIAN_POINT ( 'NONE',  ( -1.427453063608020711, -14.09184579787261349, -1.500000000000000000 ) ) ;
#19755 = CARTESIAN_POINT ( 'NONE',  ( 22.19886290009631580, 17.51851157713672436, -1.500000000000000000 ) ) ;
#19756 = CYLINDRICAL_SURFACE ( 'NONE', #32017, 4.000000000000001776 ) ;
#19757 = EDGE_CURVE ( 'NONE', #10864, #23529, #6383, .T. ) ;
#19758 = CARTESIAN_POINT ( 'NONE',  ( 0.000000000000000000, 0.000000000000000000, 0.000000000000000000 ) ) ;
#19759 = CYLINDRICAL_SURFACE ( 'NONE', #13329, 8.500000000000000000 ) ;
#19761 = ORIENTED_EDGE ( 'NONE', *, *, #19577, .T. ) ;
#19760 = CARTESIAN_POINT ( 'NONE',  ( 108.0584826075918699, -18.91149711731186756, -4.614517767564248807 ) ) ;
#19762 = DIRECTION ( 'NONE',  ( 0.000000000000000000, 0.000000000000000000, -1.000000000000000000 ) ) ;
#19763 = AXIS2_PLACEMENT_3D ( 'NONE', #26128, #5881, #20951 ) ;
#19764 = EDGE_CURVE ( 'NONE', #7632, #18687, #25071, .T. ) ;
#19765 = CARTESIAN_POINT ( 'NONE',  ( 23.23500000273119070, 2.486304738420679783, -0.2613211581691337604 ) ) ;
#19766 = CARTESIAN_POINT ( 'NONE',  ( 25.36000000136559862, 0.9349337715887185984, -3.156283516753368268 ) ) ;
#19767 = CARTESIAN_POINT ( 'NONE',  ( 107.5966592983129289, 18.76599786124473468, -5.131640265752476893 ) ) ;
#19768 = DIRECTION ( 'NONE',  ( -1.000000000000000000, -0.000000000000000000, 0.000000000000000000 ) ) ;
#19769 = CARTESIAN_POINT ( 'NONE',  ( 21.16281565822855981, -21.79884031534714595, -1.349901004997131615 ) ) ;
#19770 = AXIS2_PLACEMENT_3D ( 'NONE', #25522, #7813, #15316 ) ;
#19771 = EDGE_LOOP ( 'NONE', ( #4122, #26271, #18762 ) ) ;
#19772 = CARTESIAN_POINT ( 'NONE',  ( 3.499999999999999556, 8.357095590591338663, 1.552080310331533486 ) ) ;
#19773 = EDGE_CURVE ( 'NONE', #3605, #31514, #33092, .T. ) ;
#19774 = DIRECTION ( 'NONE',  ( 0.1437473352845080599, 0.000000000000000000, -0.9896144216807893912 ) ) ;
#19775 = ADVANCED_FACE ( 'NONE', ( #13674 ), #29079, .F. ) ;
#19776 = CARTESIAN_POINT ( 'NONE',  ( -5.687550801365593323, 2.752080473201636845, -2.228590825266444142 ) ) ;
#19777 = ORIENTED_EDGE ( 'NONE', *, *, #27813, .T. ) ;
#19778 = DIRECTION ( 'NONE',  ( 0.000000000000000000, 0.000000000000000000, -1.000000000000000000 ) ) ;
#19779 = CIRCLE ( 'NONE', #29927, 3.750000000000000444 ) ;
#19780 = CARTESIAN_POINT ( 'NONE',  ( 5.978127801841131017, -13.24614298058319228, -0.9788672205888330202 ) ) ;
#19781 = ORIENTED_EDGE ( 'NONE', *, *, #29608, .F. ) ;
#19782 = CARTESIAN_POINT ( 'NONE',  ( 108.1156589233279135, 18.82219444680288589, 4.414476567109600680 ) ) ;
#19783 = EDGE_CURVE ( 'NONE', #12125, #16462, #15976, .T. ) ;
#19784 = ADVANCED_FACE ( 'NONE', ( #24022 ), #18564, .T. ) ;
#19785 = ORIENTED_EDGE ( 'NONE', *, *, #17554, .T. ) ;
#19786 = AXIS2_PLACEMENT_3D ( 'NONE', #30046, #29355, #29708 ) ;
#19787 = VECTOR ( 'NONE', #30457, 1000.000000000000000 ) ;
#19788 = ORIENTED_EDGE ( 'NONE', *, *, #3278, .T. ) ;
#19789 = CARTESIAN_POINT ( 'NONE',  ( -2.800010172794385355, -0.4410551771863211457, 1.509141217649250688 ) ) ;
#19791 = ORIENTED_EDGE ( 'NONE', *, *, #9823, .T. ) ;
#19790 = CARTESIAN_POINT ( 'NONE',  ( 7.249760686538667009, -8.711672189281431500, 0.8180878109961559064 ) ) ;
#19792 = ORIENTED_EDGE ( 'NONE', *, *, #19136, .F. ) ;
#19793 = CARTESIAN_POINT ( 'NONE',  ( 21.73500000136559507, 1.570731468192929858, 2.892927487894329630 ) ) ;
#19794 = AXIS2_PLACEMENT_3D ( 'NONE', #14807, #14964, #32240 ) ;
#19795 = ADVANCED_FACE ( 'NONE', ( #14784, #20310 ), #27508, .T. ) ;
#19796 = ORIENTED_EDGE ( 'NONE', *, *, #10816, .T. ) ;
#19798 = AXIS2_PLACEMENT_3D ( 'NONE', #19529, #29726, #27191 ) ;
#19797 = CARTESIAN_POINT ( 'NONE',  ( 0.5704035945090657478, -2.319683995708254010, 9.255216539914220775 ) ) ;
#19800 = ORIENTED_EDGE ( 'NONE', *, *, #2609, .T. ) ;
#19799 = CARTESIAN_POINT ( 'NONE',  ( 10.00000000000000000, 4.467071865485493731, -1.625881193364652866 ) ) ;
#19801 = CARTESIAN_POINT ( 'NONE',  ( 10.00000000000000178, -6.000000000000000000, 7.347880794884119736E-16 ) ) ;
#19802 = LINE ( 'NONE', #32520, #3737 ) ;
#19803 = CARTESIAN_POINT ( 'NONE',  ( 24.73500000136559507, 1.570731468192929858, 2.892927487894329186 ) ) ;
#19804 = CARTESIAN_POINT ( 'NONE',  ( 108.1641292914955699, -20.43278308392471132, 1.481931422883725480 ) ) ;
#19805 = AXIS2_PLACEMENT_3D ( 'NONE', #9006, #12039, #19407 ) ;
#19806 = CARTESIAN_POINT ( 'NONE',  ( 0.3285611067768016147, -13.34342412962908320, -4.522129901861166701 ) ) ;
#19807 = CARTESIAN_POINT ( 'NONE',  ( 107.8771114573266630, -16.29979767294532067, -1.280413873165473060 ) ) ;
#19808 = CARTESIAN_POINT ( 'NONE',  ( 10.00000000000000000, 0.2499999999999812927, 5.003758587302150396 ) ) ;
#19809 = AXIS2_PLACEMENT_3D ( 'NONE', #16444, #6758, #16297 ) ;
#19810 = CIRCLE ( 'NONE', #24065, 5.009999999999999787 ) ;
#19811 = AXIS2_PLACEMENT_3D ( 'NONE', #31051, #28545, #15664 ) ;
#19812 = DIRECTION ( 'NONE',  ( -0.9960221812693187404, 0.08910563629484180570, 0.000000000000000000 ) ) ;
#19813 = CARTESIAN_POINT ( 'NONE',  ( 42.88108885377457824, -22.62752020922544105, 4.522129901861159595 ) ) ;
#19814 = ADVANCED_FACE ( 'NONE', ( #12452 ), #2765, .T. ) ;
#19815 = DIRECTION ( 'NONE',  ( -1.000000000000000000, -0.000000000000000000, 0.000000000000000000 ) ) ;
#19816 = DIRECTION ( 'NONE',  ( 1.000000000000000000, 0.000000000000000000, 0.000000000000000000 ) ) ;
#19817 = AXIS2_PLACEMENT_3D ( 'NONE', #7683, #7334, #27719 ) ;
#19818 = EDGE_CURVE ( 'NONE', #15750, #29889, #20656, .T. ) ;
#19819 = CARTESIAN_POINT ( 'NONE',  ( 4.183205650141505458E-16, -1.999317321091424793, -10.76487093102067050 ) ) ;
#19820 = EDGE_CURVE ( 'NONE', #25887, #1302, #2134, .T. ) ;
#19821 = CARTESIAN_POINT ( 'NONE',  ( -2.900050802731187094, 1.549418761218566143, -2.853674364686379583 ) ) ;
#19822 = ORIENTED_EDGE ( 'NONE', *, *, #328, .T. ) ;
#19823 = CARTESIAN_POINT ( 'NONE',  ( -4.300050800000000173, 2.983565686104819648, 0.3135853898029609677 ) ) ;
#19824 = AXIS2_PLACEMENT_3D ( 'NONE', #20242, #2379, #12207 ) ;
#19825 = DIRECTION ( 'NONE',  ( 0.000000000000000000, 0.9659258262890703106, -0.2588190451025135785 ) ) ;
#19826 = CARTESIAN_POINT ( 'NONE',  ( -4.400050799999999818, 2.331437884370912705, -1.887961173149511618 ) ) ;
#19827 = ORIENTED_EDGE ( 'NONE', *, *, #31553, .T. ) ;
#19828 = DIRECTION ( 'NONE',  ( 0.000000000000000000, -0.2079116908177663092, 0.9781476007338040235 ) ) ;
#19829 = ORIENTED_EDGE ( 'NONE', *, *, #15754, .T. ) ;
#19830 = CARTESIAN_POINT ( 'NONE',  ( 14.65326944990388469, -16.14433300766637203, 1.753659756057876162 ) ) ;
#19831 = SECURITY_CLASSIFICATION_LEVEL ( 'unclassified' ) ;
#19832 = VECTOR ( 'NONE', #16251, 1000.000000000000000 ) ;
#19833 = DIRECTION ( 'NONE',  ( -0.000000000000000000, -0.000000000000000000, -1.000000000000000000 ) ) ;
#19834 = VERTEX_POINT ( 'NONE', #15286 ) ;
#19835 = CARTESIAN_POINT ( 'NONE',  ( 7.381887142741853758, -19.12185317620300040, 1.499999999999999556 ) ) ;
#19836 = AXIS2_PLACEMENT_3D ( 'NONE', #25330, #30514, #7599 ) ;
#19838 = EDGE_CURVE ( 'NONE', #2120, #11002, #2596, .T. ) ;
#19837 = VECTOR ( 'NONE', #12267, 1000.000000000000000 ) ;
#19839 = VERTEX_POINT ( 'NONE', #30709 ) ;
#19840 =( BOUNDED_SURFACE ( )  B_SPLINE_SURFACE ( 3, 2, ( 
 ( #7008, #17222, #21736 ),
 ( #31945, #15019, #25242 ),
 ( #30120, #4683, #30273 ),
 ( #25564, #32788, #22575 ),
 ( #17702, #10016, #7345 ),
 ( #27731, #17389, #33096 ),
 ( #10362, #17536, #22742 ),
 ( #20395, #15208, #32946 ),
 ( #20227, #14853, #27583 ),
 ( #20077, #5029, #4839 ),
 ( #7694, #25409, #9866 ),
 ( #28084, #30612, #2671 ) ),
 .UNSPECIFIED., .F., .F., .F. ) 
 B_SPLINE_SURFACE_WITH_KNOTS ( ( 4, 2, 2, 2, 2, 4 ),
 ( 3, 3 ),
 ( 0.02103335055035494144, 0.02276256425207544981, 0.02362717110293570399, 0.02405947452836583456, 0.02427562624108089984, 0.02449177795379596165 ),
 ( 0.000000000000000000, 1.000000000000000000 ),
 .UNSPECIFIED. ) 
 GEOMETRIC_REPRESENTATION_ITEM ( )  RATIONAL_B_SPLINE_SURFACE ( (
 ( 1.000000000000000000, 0.8477574071937623579, 1.000000000000000000),
 ( 1.000000000000000000, 0.8716452794067105492, 1.000000000000000000),
 ( 1.000000000000000000, 0.8956763213340630525, 1.000000000000000000),
 ( 1.000000000000000000, 0.9319482906210421191, 1.000000000000000000),
 ( 1.000000000000000000, 0.9440737053929729727, 1.000000000000000000),
 ( 1.000000000000000000, 0.9620964665820456174, 1.000000000000000000),
 ( 1.000000000000000000, 0.9681025352175841592, 1.000000000000000000),
 ( 1.000000000000000000, 0.9768916256375786977, 1.000000000000000000),
 ( 1.000000000000000000, 0.9797842808058671027, 1.000000000000000000),
 ( 1.000000000000000000, 0.9854258872291890015, 1.000000000000000000),
 ( 1.000000000000000000, 0.9882007853475265335, 1.000000000000000000),
 ( 1.000000000000000000, 0.9906937806494865439, 1.000000000000000000) ) ) 
 REPRESENTATION_ITEM ( '' )  SURFACE ( )  );
#19841 = CC_DESIGN_PERSON_AND_ORGANIZATION_ASSIGNMENT ( #28216, #22724, ( #2373 ) ) ;
#19842 = CARTESIAN_POINT ( 'NONE',  ( 20.74999999999999645, -1.779113243963176091E-15, 0.000000000000000000 ) ) ;
#19843 = CARTESIAN_POINT ( 'NONE',  ( 18.75828436641558028, -5.879118399717574661, -3.993434336035625254 ) ) ;
#19844 = DIRECTION ( 'NONE',  ( 1.000000000000000000, 0.000000000000000000, -0.000000000000000000 ) ) ;
#19845 = DIRECTION ( 'NONE',  ( -1.000000000000000000, 0.000000000000000000, 0.000000000000000000 ) ) ;
#19846 = ORIENTED_EDGE ( 'NONE', *, *, #21053, .T. ) ;
#19847 = AXIS2_PLACEMENT_3D ( 'NONE', #19302, #26995, #4098 ) ;
#19848 = CARTESIAN_POINT ( 'NONE',  ( 34.48223484310472031, 0.5000000000000000000, -2.999999999999997335 ) ) ;
#19849 = DIRECTION ( 'NONE',  ( 1.000000000000000000, 0.000000000000000000, 0.000000000000000000 ) ) ;
#19850 = AXIS2_PLACEMENT_3D ( 'NONE', #8767, #19119, #29309 ) ;
#19851 = AXIS2_PLACEMENT_3D ( 'NONE', #8595, #18811, #29015 ) ;
#19853 = ORIENTED_EDGE ( 'NONE', *, *, #19572, .T. ) ;
#19852 = CARTESIAN_POINT ( 'NONE',  ( 56.97280603064898941, -277.2763395528616002, 0.000000000000000000 ) ) ;
#19854 = CYLINDRICAL_SURFACE ( 'NONE', #27936, 11.00000000000000000 ) ;
#19855 = DIRECTION ( 'NONE',  ( -1.000000000000000000, 8.574039729943018344E-17, -0.000000000000000000 ) ) ;
#19856 = CARTESIAN_POINT ( 'NONE',  ( 0.7632845268398871230, -0.4999240074895051067, 8.734705317681624948 ) ) ;
#19857 = PLANE ( 'NONE',  #27297 ) ;
#19858 = FACE_OUTER_BOUND ( 'NONE', #8547, .T. ) ;
#19859 = ADVANCED_FACE ( 'NONE', ( #12761 ), #28945, .F. ) ;
#19860 = B_SPLINE_CURVE_WITH_KNOTS ( 'NONE', 3,
 ( #30157, #14579, #30305, #4882, #25280, #2396, #32152, #24782, #11917, #19453 ),
 .UNSPECIFIED., .F., .F.,
 ( 4, 2, 2, 2, 4 ),
 ( 1.968338519012340724E-07, 0.0005467927057105483133, 0.001093388577569195420, 0.001639984449427842527, 0.002186580321286489634 ),
 .UNSPECIFIED. ) ;
#19861 = DIRECTION ( 'NONE',  ( 0.000000000000000000, 0.000000000000000000, -1.000000000000000000 ) ) ;
#19862 = CARTESIAN_POINT ( 'NONE',  ( 4.749760686538667009, -6.940565734314570356, -4.007137495034885255 ) ) ;
#19863 = CARTESIAN_POINT ( 'NONE',  ( 24.05656763645044904, 0.8852964313267430718, -2.499999999999998224 ) ) ;
#19864 = CARTESIAN_POINT ( 'NONE',  ( 4.749760686538667009, -7.530955069117495349, -2.741043480755002371 ) ) ;
#19865 = ORIENTED_EDGE ( 'NONE', *, *, #30881, .T. ) ;
#19866 = CIRCLE ( 'NONE', #28403, 10.87687437218811581 ) ;
#19867 = CARTESIAN_POINT ( 'NONE',  ( -50.60000000000000142, -10.96966150227468972, 1.500000000000000000 ) ) ;
#19868 = ORIENTED_EDGE ( 'NONE', *, *, #11152, .T. ) ;
#19869 = VECTOR ( 'NONE', #21327, 1000.000000000000000 ) ;
#19870 = AXIS2_PLACEMENT_3D ( 'NONE', #2558, #38, #5383 ) ;
#19871 = CARTESIAN_POINT ( 'NONE',  ( -7.354531657079157903, 0.9198621039125853827, 3.105402419394639235 ) ) ;
#19872 = AXIS2_PLACEMENT_3D ( 'NONE', #9676, #4176, #9863 ) ;
#19873 = B_SPLINE_CURVE_WITH_KNOTS ( 'NONE', 3,
 ( #25362, #10304, #7805, #15653, #25864, #2981, #23337, #441, #8121, #15812, #27851, #15154, #6415, #21168, #23490 ),
 .UNSPECIFIED., .F., .F.,
 ( 4, 2, 2, 2, 1, 2, 2, 4 ),
 ( 0.000000000000000000, 0.2500000000000000000, 0.3750000000000000000, 0.5000000000000001110, 0.6250000000000000000, 0.6875000000000000000, 0.7500000000000000000, 1.000000000000000000 ),
 .UNSPECIFIED. ) ;
#19874 = CARTESIAN_POINT ( 'NONE',  ( 69.22368686548675498, -4.843077221813552491, -5.695980980372493008 ) ) ;
#19875 = CARTESIAN_POINT ( 'NONE',  ( -8.000050800000000351, 0.000000000000000000, -3.000000000000000444 ) ) ;
#19876 = FACE_OUTER_BOUND ( 'NONE', #25325, .T. ) ;
#19877 = AXIS2_PLACEMENT_3D ( 'NONE', #27105, #32328, #2203 ) ;
#19878 = VERTEX_POINT ( 'NONE', #18138 ) ;
#19879 = CARTESIAN_POINT ( 'NONE',  ( 21.45589226044351605, -21.75378945804406072, 1.461253459911962871 ) ) ;
#19880 = CIRCLE ( 'NONE', #23608, 5.010000000000000675 ) ;
#19881 = VECTOR ( 'NONE', #23445, 1000.000000000000000 ) ;
#19882 = EDGE_LOOP ( 'NONE', ( #23871, #3370, #13171, #27730, #17779 ) ) ;
#19883 = PERSON_AND_ORGANIZATION ( #6766, #25292 ) ;
#19884 = CARTESIAN_POINT ( 'NONE',  ( 54.97686130719702646, -6.493447402409093350, 4.013697991739336501 ) ) ;
#19885 = ADVANCED_FACE ( 'NONE', ( #30368 ), #5281, .T. ) ;
#19886 = CARTESIAN_POINT ( 'NONE',  ( 6.357667975083867162, 4.790963222208105776, -7.150591204917344790 ) ) ;
#19887 = VECTOR ( 'NONE', #21653, 1000.000000000000000 ) ;
#19889 = CARTESIAN_POINT ( 'NONE',  ( 0.000000000000000000, 7.593217523260579860, 7.958834565716794707 ) ) ;
#19888 = CARTESIAN_POINT ( 'NONE',  ( 6.038145208238974604, 3.842870190353700810, 7.553619661406923314 ) ) ;
#19890 = AXIS2_PLACEMENT_3D ( 'NONE', #27512, #16963, #24651 ) ;
#19891 = ORIENTED_EDGE ( 'NONE', *, *, #13079, .F. ) ;
#19892 = AXIS2_PLACEMENT_3D ( 'NONE', #5951, #16146, #19611 ) ;
#19893 = FACE_OUTER_BOUND ( 'NONE', #20485, .T. ) ;
#19894 = FACE_OUTER_BOUND ( 'NONE', #6290, .T. ) ;
#19895 = CIRCLE ( 'NONE', #25200, 3.499999999999999556 ) ;
#19896 = CARTESIAN_POINT ( 'NONE',  ( 21.23499999999999943, 0.2613211581691317065, 2.486304738420681559 ) ) ;
#19897 = VECTOR ( 'NONE', #26000, 1000.000000000000000 ) ;
#19898 = CARTESIAN_POINT ( 'NONE',  ( 5.359470034614179035, -13.14317863668938990, -1.756412691015132754 ) ) ;
#19900 = ORIENTED_EDGE ( 'NONE', *, *, #19526, .F. ) ;
#19899 = CARTESIAN_POINT ( 'NONE',  ( 16.80274661516410006, -16.53680364986711737, 1.500000000000000444 ) ) ;
#19901 = CARTESIAN_POINT ( 'NONE',  ( -3.037550801365593411, 1.088641768524161613, 3.675193018007247403 ) ) ;
#19902 = AXIS2_PLACEMENT_3D ( 'NONE', #22524, #7453, #27864 ) ;
#19903 = DIRECTION ( 'NONE',  ( 0.03488359650710744914, -0.9989355049964836475, -0.03018263660036422935 ) ) ;
#19904 = CARTESIAN_POINT ( 'NONE',  ( 2.425585535379221280, -9.314797388879910045, 5.239665997526856245 ) ) ;
#19905 = CARTESIAN_POINT ( 'NONE',  ( 1.075551320669168920, 0.000000000000000000, -7.404527507138932485 ) ) ;
#19906 = AXIS2_PLACEMENT_3D ( 'NONE', #25751, #2882, #13048 ) ;
#19907 = ORIENTED_EDGE ( 'NONE', *, *, #9971, .F. ) ;
#19908 = EDGE_CURVE ( 'NONE', #13197, #12969, #13303, .T. ) ;
#19910 = ORIENTED_EDGE ( 'NONE', *, *, #26957, .F. ) ;
#19909 = CARTESIAN_POINT ( 'NONE',  ( 26.29336354336545867, 19.59588486419530184, 5.471072653610988823 ) ) ;
#19911 = EDGE_CURVE ( 'NONE', #19677, #24063, #17581, .T. ) ;
#19912 = AXIS2_PLACEMENT_3D ( 'NONE', #19055, #31287, #29246 ) ;
#19913 = CARTESIAN_POINT ( 'NONE',  ( 107.2415468212143992, 16.76214236186829254, 2.279906962690792849 ) ) ;
#19914 = EDGE_CURVE ( 'NONE', #689, #5903, #7626, .T. ) ;
#19915 = FACE_OUTER_BOUND ( 'NONE', #30002, .T. ) ;
#19916 = CARTESIAN_POINT ( 'NONE',  ( -16.99974336530646113, 13.10954151769649378, 1.499999999999779954 ) ) ;
#19917 = CARTESIAN_POINT ( 'NONE',  ( -23.54713438637982748, 18.60133783399175655, 1.500000000000000000 ) ) ;
#19918 = CARTESIAN_POINT ( 'NONE',  ( 15.90621625741256828, -21.21022000644183692, -1.499999999999999112 ) ) ;
#19919 = VECTOR ( 'NONE', #10392, 999.9999999999998863 ) ;
#19920 = LINE ( 'NONE', #11885, #19929 ) ;
#19921 = VECTOR ( 'NONE', #12854, 1000.000000000000000 ) ;
#19922 = AXIS2_PLACEMENT_3D ( 'NONE', #19867, #29890, #31914 ) ;
#19923 = CARTESIAN_POINT ( 'NONE',  ( 47.88345462389486329, -3.874360026377489774, 0.8105615593680149944 ) ) ;
#19924 = CARTESIAN_POINT ( 'NONE',  ( 107.3822631069532179, -16.38429022892126241, 2.521216264009422670 ) ) ;
#19925 = ORIENTED_EDGE ( 'NONE', *, *, #31821, .F. ) ;
#19926 = CARTESIAN_POINT ( 'NONE',  ( 2.274274201625327230, 0.000000000000000000, 0.000000000000000000 ) ) ;
#19927 = ORIENTED_EDGE ( 'NONE', *, *, #16125, .F. ) ;
#19928 = CIRCLE ( 'NONE', #682, 0.5000000000000000000 ) ;
#19929 = VECTOR ( 'NONE', #17545, 1000.000000000000000 ) ;
#19930 = DIRECTION ( 'NONE',  ( 1.000000000000000000, -8.574039729943018344E-17, -0.000000000000000000 ) ) ;
#19932 = DIRECTION ( 'NONE',  ( 3.623545766764202296E-17, 0.4226182617406974984, 0.9063077870366508249 ) ) ;
#19931 = VECTOR ( 'NONE', #10290, 1000.000000000000000 ) ;
#19933 = ORIENTED_EDGE ( 'NONE', *, *, #29795, .T. ) ;
#19934 = VECTOR ( 'NONE', #25323, 1000.000000000000227 ) ;
#19935 = CARTESIAN_POINT ( 'NONE',  ( 108.0895495799427124, 18.67680732057917581, -4.580456116173253100 ) ) ;
#19936 = ORIENTED_EDGE ( 'NONE', *, *, #27366, .F. ) ;
#19937 = PLANE ( 'NONE',  #23635 ) ;
#19939 = VERTEX_POINT ( 'NONE', #2290 ) ;
#19938 = CARTESIAN_POINT ( 'NONE',  ( 54.94642964003813290, -5.393904110543447317, -4.043900691114545864 ) ) ;
#19940 = ORIENTED_EDGE ( 'NONE', *, *, #6899, .F. ) ;
#19941 = CARTESIAN_POINT ( 'NONE',  ( -50.60000000000000142, -10.96966150227468972, 7.500000000000000000 ) ) ;
#19942 = CARTESIAN_POINT ( 'NONE',  ( 29.41391112839824373, -2.700987858903443950, 0.07017451552782173751 ) ) ;
#19944 = VERTEX_POINT ( 'NONE', #7438 ) ;
#19943 = DIRECTION ( 'NONE',  ( 0.000000000000000000, -0.8090169943749532244, 0.5877852522924653655 ) ) ;
#19945 = AXIS2_PLACEMENT_3D ( 'NONE', #28721, #335, #15702 ) ;
#19946 = CARTESIAN_POINT ( 'NONE',  ( 5.885541806331895387, 4.514241479885547470, 7.076443837533973991 ) ) ;
#19947 = CARTESIAN_POINT ( 'NONE',  ( 8.906813281368055613, 0.1505923090604610048, -1.366675429750782600 ) ) ;
#19948 = CIRCLE ( 'NONE', #3926, 5.500000000000000000 ) ;
#19949 = VECTOR ( 'NONE', #31242, 1000.000000000000114 ) ;
#19950 = CARTESIAN_POINT ( 'NONE',  ( 9.134478070116774262, -0.4075412269878618265, -1.500000000000000000 ) ) ;
#19951 = ADVANCED_FACE ( 'NONE', ( #17478 ), #18805, .T. ) ;
#19952 = EDGE_CURVE ( 'NONE', #61, #8252, #12783, .T. ) ;
#19954 = VERTEX_POINT ( 'NONE', #8112 ) ;
#19953 = CARTESIAN_POINT ( 'NONE',  ( 107.5354980707616761, -18.60211189756912020, -5.018107870159036921 ) ) ;
#19955 = CARTESIAN_POINT ( 'NONE',  ( 2.274274201625327230, -7.958834565716822240, 7.593217523260554103 ) ) ;
#19956 = VECTOR ( 'NONE', #27209, 1000.000000000000000 ) ;
#19958 = EDGE_CURVE ( 'NONE', #24212, #26129, #3274, .T. ) ;
#19957 = VECTOR ( 'NONE', #6516, 1000.000000000000114 ) ;
#19959 = CARTESIAN_POINT ( 'NONE',  ( 0.000000000000000000, 0.000000000000000000, 0.000000000000000000 ) ) ;
#19960 = CARTESIAN_POINT ( 'NONE',  ( 23.54750000136559507, 3.024605502323846729, -0.3178988483021056854 ) ) ;
#19961 = CC_DESIGN_APPROVAL ( #19048, ( #21105 ) ) ;
#19962 = CARTESIAN_POINT ( 'NONE',  ( 0.7632845268398871230, -8.461683424509292450, -2.223716399045660985 ) ) ;
#19963 = CARTESIAN_POINT ( 'NONE',  ( 23.27353278736380204, -21.94187821002792660, -1.000000000000000000 ) ) ;
#19964 = CARTESIAN_POINT ( 'NONE',  ( 19.66689578795281790, -21.64324770234364337, -1.457654425243551266 ) ) ;
#19965 = ORIENTED_EDGE ( 'NONE', *, *, #19376, .F. ) ;
#19966 = CARTESIAN_POINT ( 'NONE',  ( 77.65715268217998357, 26.11770293189133341, 1.508259000770581837 ) ) ;
#19967 = DIRECTION ( 'NONE',  ( -1.000000000000000000, 0.000000000000000000, 0.000000000000000000 ) ) ;
#19968 = CARTESIAN_POINT ( 'NONE',  ( -7.037550801365593856, 1.088641768524161613, 3.675193018007246959 ) ) ;
#19969 = ORIENTED_EDGE ( 'NONE', *, *, #29034, .F. ) ;
#19970 = VECTOR ( 'NONE', #31523, 1000.000000000000000 ) ;
#19971 = CARTESIAN_POINT ( 'NONE',  ( -10.00000000000000000, 0.000000000000000000, 0.000000000000000000 ) ) ;
#19972 = CARTESIAN_POINT ( 'NONE',  ( 2.458207506242386930, -0.2539630985812231234, -1.478790212540520344 ) ) ;
#19974 = ORIENTED_EDGE ( 'NONE', *, *, #19203, .T. ) ;
#19973 = AXIS2_PLACEMENT_3D ( 'NONE', #32348, #29489, #9411 ) ;
#19975 = CARTESIAN_POINT ( 'NONE',  ( 2.274274201625317460, -7.593217523260661572, 7.958834565716747633 ) ) ;
#19976 = VERTEX_POINT ( 'NONE', #20820 ) ;
#19977 = VECTOR ( 'NONE', #32385, 1000.000000000000000 ) ;
#19978 = EDGE_LOOP ( 'NONE', ( #2347, #2656, #8874, #18023, #10516 ) ) ;
#19979 = CARTESIAN_POINT ( 'NONE',  ( 0.000000000000000000, -8.475820894093002877, 4.057423117305364535 ) ) ;
#19980 = EDGE_CURVE ( 'NONE', #13791, #10256, #28827, .T. ) ;
#19982 = ORIENTED_EDGE ( 'NONE', *, *, #2988, .F. ) ;
#19981 = FACE_OUTER_BOUND ( 'NONE', #4094, .T. ) ;
#19983 = EDGE_LOOP ( 'NONE', ( #20054, #7635, #6777, #2989 ) ) ;
#19984 = CARTESIAN_POINT ( 'NONE',  ( 21.61000000136559507, 3.156283516753366047, 0.9349337715887203748 ) ) ;
#19985 = APPROVAL_PERSON_ORGANIZATION ( #18520, #7375, #13795 ) ;
#19986 = ORIENTED_EDGE ( 'NONE', *, *, #8937, .F. ) ;
#19987 = DIRECTION ( 'NONE',  ( 0.000000000000000000, 0.000000000000000000, -1.000000000000000000 ) ) ;
#19988 = ADVANCED_FACE ( 'NONE', ( #11108 ), #23964, .F. ) ;
#19990 = ORIENTED_EDGE ( 'NONE', *, *, #30881, .F. ) ;
#19989 = CARTESIAN_POINT ( 'NONE',  ( 41.34552818481519409, -4.491668296270788119, -2.184957213353903693 ) ) ;
#19991 = DIRECTION ( 'NONE',  ( -8.281886410780491305E-17, -0.9659258262890662028, -0.2588190451025284000 ) ) ;
#19992 = CARTESIAN_POINT ( 'NONE',  ( 85.49734435724840864, -7.913007294147472059, 0.07017451552781736601 ) ) ;
#19993 = CARTESIAN_POINT ( 'NONE',  ( 24.36000000136559507, 0.9349337715887185984, -3.156283516753368268 ) ) ;
#19994 = CARTESIAN_POINT ( 'NONE',  ( 107.4500593345382811, -17.36019228850094720, 4.522129901861156931 ) ) ;
#19995 = VECTOR ( 'NONE', #11502, 1000.000000000000114 ) ;
#19996 = CARTESIAN_POINT ( 'NONE',  ( -50.60000000000000142, -10.96966150227468972, 0.9999999999999991118 ) ) ;
#19997 = EDGE_CURVE ( 'NONE', #32892, #22736, #11706, .T. ) ;
#19998 = CARTESIAN_POINT ( 'NONE',  ( -50.81000000000000227, -10.96999999999998643, 2.028141679950118625 ) ) ;
#19999 = DIRECTION ( 'NONE',  ( 0.000000000000000000, 1.000000000000000000, 0.000000000000000000 ) ) ;
#20000 = DIRECTION ( 'NONE',  ( -1.000000000000000000, -5.361488761196503499E-16, 0.000000000000000000 ) ) ;
#20001 = CARTESIAN_POINT ( 'NONE',  ( 47.75999538435722513, -8.435302152663906483, 0.02339150517593243869 ) ) ;
#20002 = CARTESIAN_POINT ( 'NONE',  ( 0.7632845268398871230, 7.360373001730917686, 4.729683950898899703 ) ) ;
#20003 = CARTESIAN_POINT ( 'NONE',  ( 68.56906952848913761, -3.255983411058663179, -0.02339150518254430253 ) ) ;
#20004 = EDGE_CURVE ( 'NONE', #26351, #29995, #28677, .T. ) ;
#20005 = CIRCLE ( 'NONE', #1035, 8.500000000000000000 ) ;
#20006 = CARTESIAN_POINT ( 'NONE',  ( 0.5640491644726027820, -2.305464659958381901, -9.257234168482330716 ) ) ;
#20007 = CARTESIAN_POINT ( 'NONE',  ( -3.600050802731187272, 3.113457007523260156, -0.9222479816126439855 ) ) ;
#20008 = ORIENTED_EDGE ( 'NONE', *, *, #11645, .T. ) ;
#20009 = ADVANCED_FACE ( 'NONE', ( #31213 ), #9378, .T. ) ;
#20010 = CARTESIAN_POINT ( 'NONE',  ( -2.650050800000000262, 2.853674364686379583, 1.549418761218565921 ) ) ;
#20011 = B_SPLINE_CURVE_WITH_KNOTS ( 'NONE', 3,
 ( #16774, #14092, #24292, #1406, #11581, #21777, #31986, #9054 ),
 .UNSPECIFIED., .F., .F.,
 ( 4, 2, 2, 4 ),
 ( 0.000000000000000000, 0.5000000000000000000, 0.7500000000000000000, 1.000000000000000000 ),
 .UNSPECIFIED. ) ;
#20012 = DIRECTION ( 'NONE',  ( 1.000000000000000000, 1.387778780781445833E-14, 4.846230290920773249E-16 ) ) ;
#20013 = CARTESIAN_POINT ( 'NONE',  ( -4.506376978575949543, 0.1572233378491263989, -2.999999999999999556 ) ) ;
#20014 = ORIENTED_EDGE ( 'NONE', *, *, #31082, .T. ) ;
#20015 = DIRECTION ( 'NONE',  ( 0.000000000000000000, -0.4226182617407038267, 0.9063077870366479383 ) ) ;
#20016 = EDGE_CURVE ( 'NONE', #32756, #14263, #9580, .T. ) ;
#20017 = VECTOR ( 'NONE', #19497, 1000.000000000000000 ) ;
#20018 = ORIENTED_EDGE ( 'NONE', *, *, #837, .T. ) ;
#20019 = CARTESIAN_POINT ( 'NONE',  ( 108.5619817448483531, 15.65002148400668247, -0.4463807625373593657 ) ) ;
#20020 = EDGE_CURVE ( 'NONE', #10748, #22902, #16307, .T. ) ;
#20021 = PERSON_AND_ORGANIZATION ( #9531, #2943 ) ;
#20022 = CARTESIAN_POINT ( 'NONE',  ( -0.5616989984784650503, -12.44624546261628417, -4.522129901861166701 ) ) ;
#20023 = ORIENTED_EDGE ( 'NONE', *, *, #29041, .F. ) ;
#20024 = CARTESIAN_POINT ( 'NONE',  ( 0.5281637029061487798, -15.74321946213827061, 1.500000000000000222 ) ) ;
#20025 = ORIENTED_EDGE ( 'NONE', *, *, #17437, .F. ) ;
#20026 = DIRECTION ( 'NONE',  ( 0.000000000000000000, 0.9961946980917449901, 0.08715574274766461904 ) ) ;
#20027 = CARTESIAN_POINT ( 'NONE',  ( 69.06417839047257701, -5.990839020724394004, -4.155405370686176880 ) ) ;
#20028 = CARTESIAN_POINT ( 'NONE',  ( 12.44989959798868817, 0.000000000000000000, -2.482234843104710986 ) ) ;
#20029 = CARTESIAN_POINT ( 'NONE',  ( 3.499999999999999556, -6.200809695932770538, -0.7745709230445805282 ) ) ;
#20030 = LINE ( 'NONE', #10586, #15081 ) ;
#20031 = EDGE_CURVE ( 'NONE', #1745, #15594, #29344, .T. ) ;
#20032 = CARTESIAN_POINT ( 'NONE',  ( 21.36441059928002417, -21.76424620013107969, -1.417681050192670877 ) ) ;
#20033 = EDGE_CURVE ( 'NONE', #6030, #9245, #30419, .T. ) ;
#20034 = DIRECTION ( 'NONE',  ( 1.000000000000000000, -8.574039729943018344E-17, -0.000000000000000000 ) ) ;
#20036 = ORIENTED_EDGE ( 'NONE', *, *, #11623, .F. ) ;
#20035 = DIRECTION ( 'NONE',  ( -0.000000000000000000, 0.5735764363510439390, 0.8191520442889932418 ) ) ;
#20037 = DIRECTION ( 'NONE',  ( 0.000000000000000000, 0.000000000000000000, 1.000000000000000000 ) ) ;
#20038 = CARTESIAN_POINT ( 'NONE',  ( 107.7536796087345294, 16.80655079293032017, -1.379243061950440108 ) ) ;
#20039 = CARTESIAN_POINT ( 'NONE',  ( 16.36487458112949511, 19.37645981759117575, -4.612695725900422872 ) ) ;
#20040 = CARTESIAN_POINT ( 'NONE',  ( -15.09999999999999609, 0.000000000000000000, 1.500000000000000000 ) ) ;
#20041 = EDGE_CURVE ( 'NONE', #25919, #23564, #14766, .T. ) ;
#20042 = DIRECTION ( 'NONE',  ( -1.000000000000000000, -0.000000000000000000, 0.000000000000000000 ) ) ;
#20043 = LINE ( 'NONE', #32068, #13959 ) ;
#20044 = CARTESIAN_POINT ( 'NONE',  ( -56.63622713806018538, 0.1497937355729806186, -1.035521931139215868 ) ) ;
#20045 = CARTESIAN_POINT ( 'NONE',  ( 23.15652614122341291, -21.92931078907622933, 1.107159753868761198 ) ) ;
#20046 = ORIENTED_EDGE ( 'NONE', *, *, #13088, .T. ) ;
#20047 = CARTESIAN_POINT ( 'NONE',  ( -7.362550801365593145, -2.228590825266444586, -2.752080473201636401 ) ) ;
#20048 = ORIENTED_EDGE ( 'NONE', *, *, #28473, .T. ) ;
#20049 = EDGE_CURVE ( 'NONE', #32897, #6905, #18338, .T. ) ;
#20050 = CARTESIAN_POINT ( 'NONE',  ( -6.904531657079157725, 0.3127741368606810068, -2.975847129947406522 ) ) ;
#20051 = DIRECTION ( 'NONE',  ( -1.000000000000000000, 0.000000000000000000, -0.000000000000000000 ) ) ;
#20052 = CARTESIAN_POINT ( 'NONE',  ( 69.32965659118902124, -6.955028994473984483, -4.522129901861164036 ) ) ;
#20053 = CARTESIAN_POINT ( 'NONE',  ( 1.429697474035917404, -10.23340377719132377, 1.764565172273165228 ) ) ;
#20054 = ORIENTED_EDGE ( 'NONE', *, *, #19288, .T. ) ;
#20055 = CARTESIAN_POINT ( 'NONE',  ( 3.499999999999999556, 0.000000000000000000, 0.000000000000000000 ) ) ;
#20056 = ORIENTED_EDGE ( 'NONE', *, *, #18267, .T. ) ;
#20057 = CARTESIAN_POINT ( 'NONE',  ( 6.356382477965130562, -5.080803740829769488, 6.947086032709915315 ) ) ;
#20058 = PERSON_AND_ORGANIZATION_ROLE ( 'design_owner' ) ;
#20059 = CARTESIAN_POINT ( 'NONE',  ( 54.97711309884392961, -6.502545147706987549, 3.999773680152649558 ) ) ;
#20060 = EDGE_CURVE ( 'NONE', #13510, #31647, #4766, .T. ) ;
#20061 = FACE_OUTER_BOUND ( 'NONE', #2469, .T. ) ;
#20063 = CARTESIAN_POINT ( 'NONE',  ( 102.5305753040692878, -0.1042037546421146210, 0.07017451552781736601 ) ) ;
#20062 = CARTESIAN_POINT ( 'NONE',  ( 3.499999999999999556, 0.000000000000000000, 0.000000000000000000 ) ) ;
#20064 = VERTEX_POINT ( 'NONE', #32186 ) ;
#20065 = ADVANCED_FACE ( 'NONE', ( #9073 ), #1266, .T. ) ;
#20066 = CARTESIAN_POINT ( 'NONE',  ( 7.249760686538667009, 0.000000000000000000, 0.000000000000000000 ) ) ;
#20067 = CARTESIAN_POINT ( 'NONE',  ( 2.440333456259505596, 1.206185435486435864, 10.60697035673404187 ) ) ;
#20068 = CARTESIAN_POINT ( 'NONE',  ( 25.92250000136559507, 0.3178988483021036315, 3.024605502323848949 ) ) ;
#20069 = CARTESIAN_POINT ( 'NONE',  ( 0.9579555755618084367, -9.537443266964631405, -1.767394926759007223 ) ) ;
#20071 = VERTEX_POINT ( 'NONE', #24310 ) ;
#20070 = CARTESIAN_POINT ( 'NONE',  ( 6.038144853276843804, 8.412419482080421673, -1.027626812407915313 ) ) ;
#20072 = CARTESIAN_POINT ( 'NONE',  ( -7.812550801365593323, 3.368539882008727115, 1.828967928396026954 ) ) ;
#20073 = DIRECTION ( 'NONE',  ( 1.000000000000000000, -0.000000000000000000, 8.654346879536960414E-15 ) ) ;
#20074 = CARTESIAN_POINT ( 'NONE',  ( 69.09268213438589612, -2.232183665269761086, 0.07017451552782173751 ) ) ;
#20075 = LINE ( 'NONE', #15357, #28895 ) ;
#20076 = VERTEX_POINT ( 'NONE', #27310 ) ;
#20078 = ORIENTED_EDGE ( 'NONE', *, *, #27716, .F. ) ;
#20077 = CARTESIAN_POINT ( 'NONE',  ( 24.25321317639194163, -17.33169478063257429, 1.345077977218910537 ) ) ;
#20079 = EDGE_CURVE ( 'NONE', #14801, #13430, #19090, .T. ) ;
#20080 = CARTESIAN_POINT ( 'NONE',  ( 2.857988133321602842, 6.150950518050580129, 7.318787950824131805 ) ) ;
#20081 = CYLINDRICAL_SURFACE ( 'NONE', #18678, 5.010000000000000675 ) ;
#20082 =( BOUNDED_CURVE ( )  B_SPLINE_CURVE ( 3, ( #28607, #23748, #13537, #23405 ),
 .UNSPECIFIED., .F., .F. ) 
 B_SPLINE_CURVE_WITH_KNOTS ( ( 4, 4 ),
 ( 3.333578871309104574, 4.712388980384684345 ),
 .UNSPECIFIED. ) 
 CURVE ( )  GEOMETRIC_REPRESENTATION_ITEM ( )  RATIONAL_B_SPLINE_CURVE ( ( 1.000000000000000000, 0.8477497222584673420, 0.8477497222584673420, 1.000000000000000000 ) ) 
 REPRESENTATION_ITEM ( '' )  );
#20083 = CARTESIAN_POINT ( 'NONE',  ( -4.262285728429963137E-16, -4.971152295393305387, 0.6226916219171877431 ) ) ;
#20084 = CARTESIAN_POINT ( 'NONE',  ( -29.41021809322157310, 5.485000000000014531, 1.500000000000000000 ) ) ;
#20085 = ADVANCED_FACE ( 'NONE', ( #4430 ), #3937, .T. ) ;
#20086 = CARTESIAN_POINT ( 'NONE',  ( -26.87870632630977852, 4.906976360849698793, 2.121007814587993590 ) ) ;
#20087 = CARTESIAN_POINT ( 'NONE',  ( -3.446114928647880493, -10.31582149787081981, -1.743523040558758508 ) ) ;
#20088 = PRODUCT_RELATED_PRODUCT_CATEGORY ( 'detail', '', ( #17492 ) ) ;
#20089 = DIRECTION ( 'NONE',  ( 0.000000000000000000, 0.000000000000000000, 1.000000000000000000 ) ) ;
#20090 = DIRECTION ( 'NONE',  ( -0.000000000000000000, -0.5735764363510496011, -0.8191520442889893561 ) ) ;
#20091 = CARTESIAN_POINT ( 'NONE',  ( 102.8580990270160385, -4.820463887425401772, 4.522129901861162260 ) ) ;
#20092 = ORIENTED_EDGE ( 'NONE', *, *, #9421, .T. ) ;
#20093 = DIRECTION ( 'NONE',  ( -1.000000000000000000, -0.000000000000000000, -0.000000000000000000 ) ) ;
#20094 = PERSON_AND_ORGANIZATION ( #6766, #25292 ) ;
#20095 = DIRECTION ( 'NONE',  ( 0.000000000000000000, 0.000000000000000000, 1.000000000000000000 ) ) ;
#20096 = ORIENTED_EDGE ( 'NONE', *, *, #5273, .F. ) ;
#20097 = EDGE_CURVE ( 'NONE', #4314, #32347, #3188, .T. ) ;
#20098 = CARTESIAN_POINT ( 'NONE',  ( 108.0119426754549750, 18.24466145416912610, -4.459116668420948670 ) ) ;
#20099 = ORIENTED_EDGE ( 'NONE', *, *, #24305, .F. ) ;
#20100 = LINE ( 'NONE', #19591, #20461 ) ;
#20101 = EDGE_CURVE ( 'NONE', #20892, #3605, #4591, .T. ) ;
#20103 = ORIENTED_EDGE ( 'NONE', *, *, #14562, .F. ) ;
#20102 = CARTESIAN_POINT ( 'NONE',  ( 84.96723802116302693, -4.086039325506168218, -4.033869228762161363 ) ) ;
#20104 = ORIENTED_EDGE ( 'NONE', *, *, #1172, .F. ) ;
#20105 = PLANE ( 'NONE',  #27349 ) ;
#20106 = LINE ( 'NONE', #7535, #30592 ) ;
#20107 = CARTESIAN_POINT ( 'NONE',  ( 41.43219399715333395, -3.145521524160642457, 1.915219082070892531 ) ) ;
#20109 = ORIENTED_EDGE ( 'NONE', *, *, #5979, .T. ) ;
#20108 = CARTESIAN_POINT ( 'NONE',  ( 22.50111451137534502, -3.256483526998273983E-15, 2.499999999999998668 ) ) ;
#20110 = DIRECTION ( 'NONE',  ( 8.281886410780524585E-17, 0.9659258262890700886, -0.2588190451025141336 ) ) ;
#20111 = DIRECTION ( 'NONE',  ( -1.000000000000000000, -0.000000000000000000, -0.000000000000000000 ) ) ;
#20112 = CARTESIAN_POINT ( 'NONE',  ( 9.038457413085614789, 1.187263343935664605E-16, 1.016831166589732938 ) ) ;
#20113 = LINE ( 'NONE', #30306, #14393 ) ;
#20115 = EDGE_LOOP ( 'NONE', ( #24412, #24423, #13395, #11892 ) ) ;
#20114 = CARTESIAN_POINT ( 'NONE',  ( 9.282537329959909655, 0.2172754300399158400, -1.041239158277187160 ) ) ;
#20116 = CARTESIAN_POINT ( 'NONE',  ( 7.249760686538667009, 8.721381771256204729, 0.7071067811865429098 ) ) ;
#20117 = CARTESIAN_POINT ( 'NONE',  ( 9.999999999999998224, -4.681538312723523276, 0.8254815157535098091 ) ) ;
#20118 = CARTESIAN_POINT ( 'NONE',  ( 23.92250000136559507, -1.913930629741527500, 2.363507492473149618 ) ) ;
#20119 = CARTESIAN_POINT ( 'NONE',  ( 107.5137997967071612, 18.28951216238115762, -5.076820443063085442 ) ) ;
#20120 = CARTESIAN_POINT ( 'NONE',  ( 1.075551320669168476, 0.5000000000000000000, -7.404527507138929820 ) ) ;
#20121 = CARTESIAN_POINT ( 'NONE',  ( 2.382865613620175349, 0.000000000000000000, 1.000000000000000222 ) ) ;
#20122 = EDGE_LOOP ( 'NONE', ( #27143, #21363, #21350, #5665 ) ) ;
#20123 = DIRECTION ( 'NONE',  ( 0.000000000000000000, 0.9063077870366477162, 0.4226182617407044928 ) ) ;
#20124 = FACE_OUTER_BOUND ( 'NONE', #22835, .T. ) ;
#20125 = CARTESIAN_POINT ( 'NONE',  ( -6.087550801365593678, -2.752080473201636845, 2.228590825266444586 ) ) ;
#20126 = ORIENTED_EDGE ( 'NONE', *, *, #2054, .F. ) ;
#20127 = B_SPLINE_CURVE_WITH_KNOTS ( 'NONE', 3,
 ( #10934, #20968, #28654, #8413 ),
 .UNSPECIFIED., .F., .F.,
 ( 4, 4 ),
 ( 0.9237604347401378035, 1.000000000000000000 ),
 .UNSPECIFIED. ) ;
#20128 = CARTESIAN_POINT ( 'NONE',  ( 101.7221769401408409, -2.897900707892763439, -3.993434276071010203 ) ) ;
#20129 = CARTESIAN_POINT ( 'NONE',  ( 5.377543748152548986, -7.530955069117495349, -2.741043480755002371 ) ) ;
#20130 = CARTESIAN_POINT ( 'NONE',  ( 0.000000000000000000, 0.000000000000000000, 0.000000000000000000 ) ) ;
#20131 = ORIENTED_EDGE ( 'NONE', *, *, #24722, .T. ) ;
#20132 = DIRECTION ( 'NONE',  ( -1.000000000000000000, 0.000000000000000000, 0.000000000000000000 ) ) ;
#20133 = ADVANCED_FACE ( 'NONE', ( #14109 ), #16942, .T. ) ;
#20134 = VERTEX_POINT ( 'NONE', #21961 ) ;
#20135 = EDGE_CURVE ( 'NONE', #11370, #25797, #7434, .T. ) ;
#20136 = DIRECTION ( 'NONE',  ( -1.000000000000000000, 8.574039729943019576E-17, 0.000000000000000000 ) ) ;
#20137 = EDGE_LOOP ( 'NONE', ( #12202, #22576, #27419 ) ) ;
#20138 = CARTESIAN_POINT ( 'NONE',  ( -3.082813266614905068, -0.4373090928652427212, 1.500000000000000000 ) ) ;
#20140 = ORIENTED_EDGE ( 'NONE', *, *, #18842, .T. ) ;
#20139 = DIRECTION ( 'NONE',  ( -1.000000000000000000, 0.000000000000000000, 0.000000000000000000 ) ) ;
#20141 = EDGE_LOOP ( 'NONE', ( #9370, #3241, #3409, #26149, #13266 ) ) ;
#20142 = CARTESIAN_POINT ( 'NONE',  ( -23.54713438637982748, 8.275374457817617824, 8.599999999999999645 ) ) ;
#20143 = ORIENTED_EDGE ( 'NONE', *, *, #8715, .F. ) ;
#20144 = FACE_OUTER_BOUND ( 'NONE', #13725, .T. ) ;
#20146 = ORIENTED_EDGE ( 'NONE', *, *, #5403, .T. ) ;
#20145 = CARTESIAN_POINT ( 'NONE',  ( 21.32535692059155963, -21.82495604402122069, 1.318256435726650633 ) ) ;
#20147 = CARTESIAN_POINT ( 'NONE',  ( -5.550050800000001061, -3.113457007523259268, 0.9222479816126455399 ) ) ;
#20148 = FACE_OUTER_BOUND ( 'NONE', #21750, .T. ) ;
#20149 = DIRECTION ( 'NONE',  ( -1.000000000000000000, 0.000000000000000000, -0.000000000000000000 ) ) ;
#20150 = DIRECTION ( 'NONE',  ( 0.000000000000000000, 0.000000000000000000, 1.000000000000000000 ) ) ;
#20151 = DIRECTION ( 'NONE',  ( 0.000000000000000000, 1.000000000000000000, 0.000000000000000000 ) ) ;
#20152 = CARTESIAN_POINT ( 'NONE',  ( -1.176310634206514104E-14, 21.94000000000002260, 1.500000000000000000 ) ) ;
#20153 = CARTESIAN_POINT ( 'NONE',  ( 23.58234648083524121, -8.048792613698569909, -0.02339150517595086839 ) ) ;
#20154 = DIRECTION ( 'NONE',  ( 0.000000000000000000, 1.000000000000000000, 0.000000000000000000 ) ) ;
#20155 = DIRECTION ( 'NONE',  ( 0.000000000000000000, -0.9271838545667855369, -0.3746065934159163446 ) ) ;
#20156 = DIRECTION ( 'NONE',  ( 1.000000000000000000, 0.000000000000000000, 3.469446951953611033E-15 ) ) ;
#20157 = CARTESIAN_POINT ( 'NONE',  ( -3.450050802731187805, 1.887961173149511618, 2.331437884370912705 ) ) ;
#20158 = VERTEX_POINT ( 'NONE', #12595 ) ;
#20159 = CARTESIAN_POINT ( 'NONE',  ( -3.150050800000000262, -3.113457007523259268, 0.9222479816126455399 ) ) ;
#20160 = EDGE_CURVE ( 'NONE', #7529, #6546, #31487, .T. ) ;
#20161 = CARTESIAN_POINT ( 'NONE',  ( 0.5704036742842227836, 3.563415854978491115, 8.851103337321282183 ) ) ;
#20162 = DIRECTION ( 'NONE',  ( -1.000000000000000000, 0.000000000000000000, 0.000000000000000000 ) ) ;
#20163 = ORIENTED_EDGE ( 'NONE', *, *, #23814, .T. ) ;
#20164 = CARTESIAN_POINT ( 'NONE',  ( 3.499999999999999556, -5.349675154362298457, -3.229702268444986757 ) ) ;
#20165 = DIRECTION ( 'NONE',  ( 0.000000000000000000, 1.000000000000000000, 0.000000000000000000 ) ) ;
#20166 = CARTESIAN_POINT ( 'NONE',  ( 107.5223429394918071, -18.41085303761574821, 5.107465446621668903 ) ) ;
#20167 = ORIENTED_EDGE ( 'NONE', *, *, #2673, .T. ) ;
#20168 = CARTESIAN_POINT ( 'NONE',  ( 101.7974586501929366, -3.981938604909214696, -4.091315454904098203 ) ) ;
#20169 = APPROVAL_ROLE ( '' ) ;
#20170 = CARTESIAN_POINT ( 'NONE',  ( 41.20585001718148277, -8.497180311781159290, 0.07017451552781736601 ) ) ;
#20171 = ORIENTED_EDGE ( 'NONE', *, *, #9066, .F. ) ;
#20172 = CARTESIAN_POINT ( 'NONE',  ( 0.4892055063894280575, 9.505891060653322455, 2.300561732651089653 ) ) ;
#20173 = ORIENTED_EDGE ( 'NONE', *, *, #30148, .T. ) ;
#20174 = CARTESIAN_POINT ( 'NONE',  ( 107.9823348541772390, -17.81498841130776256, -4.403862939664326959 ) ) ;
#20176 = ORIENTED_EDGE ( 'NONE', *, *, #4495, .F. ) ;
#20175 = DIRECTION ( 'NONE',  ( -1.000000000000000000, 0.000000000000000000, 0.000000000000000000 ) ) ;
#20177 = DIRECTION ( 'NONE',  ( -1.000000000000000000, 0.000000000000000000, 0.000000000000000000 ) ) ;
#20178 = CARTESIAN_POINT ( 'NONE',  ( 107.3477315916820913, -15.88627780335592732, -1.500000000000000000 ) ) ;
#20179 = EDGE_CURVE ( 'NONE', #593, #5840, #22721, .T. ) ;
#20180 = CARTESIAN_POINT ( 'NONE',  ( 21.86019183973456137, -21.78358645912093294, -1.498801117633766999 ) ) ;
#20181 = CARTESIAN_POINT ( 'NONE',  ( 101.8016823592330127, -4.042758964360499974, 3.993434276137187489 ) ) ;
#20182 = B_SPLINE_CURVE_WITH_KNOTS ( 'NONE', 3,
 ( #27704, #25384, #17863, #20201, #12323, #5310, #15489, #25537, #2492, #25704, #2831, #22543, #27559, #7320, #27883, #13004, #17672, #23215, #20053, #10332, #146, #15332, #2142, #33067, #9837, #10142, #319, #20363, #30247, #4811, #30580, #10491, #7663, #20705, #2643, #17510 ),
 .UNSPECIFIED., .F., .F.,
 ( 4, 2, 2, 2, 2, 2, 2, 2, 2, 2, 2, 2, 2, 2, 2, 2, 2, 4 ),
 ( 0.08639979630981461933, 0.09035893056720895045, 0.09431806482460326768, 0.09827719908199758492, 0.1002567662106947505, 0.1022363333393919160, 0.1042159004680890816, 0.1052056840324376574, 0.1061954675967862471, 0.1081750347254834127, 0.1101546018541805783, 0.1106494936363548731, 0.1111443854185291680, 0.1121341689828777438, 0.1131239525472263197, 0.1141137361115749094, 0.1160933032402720610, 0.1180728703689692266 ),
 .UNSPECIFIED. ) ;
#20183 = ORIENTED_EDGE ( 'NONE', *, *, #12571, .F. ) ;
#20184 = LINE ( 'NONE', #23199, #11764 ) ;
#20185 = CARTESIAN_POINT ( 'NONE',  ( -4.162942409646514186, -5.022711880624455567E-15, 2.999999999999999556 ) ) ;
#20186 = EDGE_CURVE ( 'NONE', #15174, #23664, #22649, .T. ) ;
#20187 = CARTESIAN_POINT ( 'NONE',  ( 2.357329994281655239, -2.053141773251381252, -10.64078702437733881 ) ) ;
#20188 = CARTESIAN_POINT ( 'NONE',  ( -16.96515769256209794, -27.93932300454937590, 11.09540449768827131 ) ) ;
#20189 = CARTESIAN_POINT ( 'NONE',  ( 10.00000000000000000, 3.055657119358849094, -3.641590349731898879 ) ) ;
#20190 = DIRECTION ( 'NONE',  ( -1.000000000000000000, 0.000000000000000000, 0.000000000000000000 ) ) ;
#20191 = CARTESIAN_POINT ( 'NONE',  ( -56.51865391759180568, 0.05810651368888004181, -1.023525953523438226 ) ) ;
#20192 = CARTESIAN_POINT ( 'NONE',  ( 23.11934981620040119, -21.92529594990400099, 1.124851831741630503 ) ) ;
#20193 = EDGE_LOOP ( 'NONE', ( #2582, #20441, #6986, #33008 ) ) ;
#20194 = ADVANCED_FACE ( 'NONE', ( #30497 ), #32854, .T. ) ;
#20195 = CARTESIAN_POINT ( 'NONE',  ( -5.862550801365593145, -3.521866450007987037, -0.3701630799359323931 ) ) ;
#20196 = VERTEX_POINT ( 'NONE', #20636 ) ;
#20197 = CARTESIAN_POINT ( 'NONE',  ( -5.604531657079157903, -2.325406398514293205, 1.883076972206379818 ) ) ;
#20198 = CARTESIAN_POINT ( 'NONE',  ( 23.11000000136559507, -2.892927487894331406, 1.570731468192932301 ) ) ;
#20199 = FACE_OUTER_BOUND ( 'NONE', #21474, .T. ) ;
#20200 = ADVANCED_FACE ( 'NONE', ( #4917 ), #14387, .T. ) ;
#20201 = CARTESIAN_POINT ( 'NONE',  ( 15.82117458021303058, -16.37366068799997265, 1.753541294540382545 ) ) ;
#20202 = CARTESIAN_POINT ( 'NONE',  ( 108.2141344899977895, 20.71717987834380637, 1.495953707351421968 ) ) ;
#20203 = VERTEX_POINT ( 'NONE', #2743 ) ;
#20204 = CARTESIAN_POINT ( 'NONE',  ( 19.01480233883215476, -3.011762293217291830, 0.4426577273443488281 ) ) ;
#20205 = EDGE_CURVE ( 'NONE', #596, #20676, #13864, .T. ) ;
#20206 = CARTESIAN_POINT ( 'NONE',  ( 41.43709133142961321, -4.769546740945156849, -4.522129901861162260 ) ) ;
#20207 = ORIENTED_EDGE ( 'NONE', *, *, #19705, .T. ) ;
#20208 = CARTESIAN_POINT ( 'NONE',  ( 5.489343806296448136, -1.512045527216150598, -7.976812024616041441 ) ) ;
#20209 = APPROVAL_ROLE ( '' ) ;
#20210 = CARTESIAN_POINT ( 'NONE',  ( 28.66435036896872290, -6.755537191812748254, 4.008637382357084888 ) ) ;
#20211 = CARTESIAN_POINT ( 'NONE',  ( 5.377543748152549874, 4.007137495034909236, -6.940565734314555257 ) ) ;
#20213 = CARTESIAN_POINT ( 'NONE',  ( 5.377543748152548098, 8.385837730238846314E-14, -8.014274990069656823 ) ) ;
#20212 = CARTESIAN_POINT ( 'NONE',  ( 108.8978791464556508, 17.52043075494136204, -4.999054092451819642 ) ) ;
#20214 = ORIENTED_EDGE ( 'NONE', *, *, #3314, .F. ) ;
#20215 = CARTESIAN_POINT ( 'NONE',  ( -8.000050800000002127, -2.890068019510989572, 0.8529434025099479344 ) ) ;
#20216 = LINE ( 'NONE', #2853, #17127 ) ;
#20217 = CARTESIAN_POINT ( 'NONE',  ( 22.61000000136559507, 2.892927487894327410, -1.570731468192931635 ) ) ;
#20218 = ADVANCED_FACE ( 'NONE', ( #28294 ), #12433, .T. ) ;
#20219 = FACE_OUTER_BOUND ( 'NONE', #4046, .T. ) ;
#20221 = ORIENTED_EDGE ( 'NONE', *, *, #20577, .T. ) ;
#20220 = CARTESIAN_POINT ( 'NONE',  ( 0.5309851148689820333, -4.399114163800174282, 1.500000000000000444 ) ) ;
#20222 = CARTESIAN_POINT ( 'NONE',  ( -4.612550801365593145, 3.368539882008727115, 1.828967928396026954 ) ) ;
#20223 = CARTESIAN_POINT ( 'NONE',  ( -40.27879340802675046, -12.50360960397076404, 5.500000000000000000 ) ) ;
#20224 = CARTESIAN_POINT ( 'NONE',  ( -23.54713438637982748, 18.90773822806172433, 1.500000000000000000 ) ) ;
#20225 = CARTESIAN_POINT ( 'NONE',  ( 54.97742507208618434, -6.506533559248983245, -3.993434333358883759 ) ) ;
#20226 = EDGE_LOOP ( 'NONE', ( #19750, #8960, #7695, #5119 ) ) ;
#20228 = ORIENTED_EDGE ( 'NONE', *, *, #17343, .F. ) ;
#20227 = CARTESIAN_POINT ( 'NONE',  ( 24.12394826718730556, -17.31889127434072506, 1.369171926258124117 ) ) ;
#20229 = DIRECTION ( 'NONE',  ( -1.000000000000000000, -0.000000000000000000, -0.000000000000000000 ) ) ;
#20230 = CARTESIAN_POINT ( 'NONE',  ( 107.8323134827048619, 20.09434993960548965, -3.035090133884138286 ) ) ;
#20231 = ADVANCED_FACE ( 'NONE', ( #10252 ), #5411, .T. ) ;
#20232 = CARTESIAN_POINT ( 'NONE',  ( 22.36000000136559507, -1.570731468192933633, -2.892927487894330962 ) ) ;
#20233 = CARTESIAN_POINT ( 'NONE',  ( 54.91409664898025511, -4.233361888145934060, 2.184956776138676116 ) ) ;
#20234 = CARTESIAN_POINT ( 'NONE',  ( 6.168868874606070918, -18.37414512067872607, -1.500000000000239142 ) ) ;
#20235 = EDGE_CURVE ( 'NONE', #3680, #26986, #33004, .T. ) ;
#20236 = CARTESIAN_POINT ( 'NONE',  ( 41.34386496145464207, -3.886814715717140878, 0.07017451552807979498 ) ) ;
#20237 = CARTESIAN_POINT ( 'NONE',  ( 102.9361373302715918, -5.944196040818414239, 2.713652344655544724 ) ) ;
#20238 = ORIENTED_EDGE ( 'NONE', *, *, #8796, .T. ) ;
#20239 = CARTESIAN_POINT ( 'NONE',  ( 2.440333863881507526, 7.872241054360261003, -7.210444323284713519 ) ) ;
#20240 = ADVANCED_FACE ( 'NONE', ( #19981 ), #2076, .F. ) ;
#20241 = PERSON_AND_ORGANIZATION_ROLE ( 'creator' ) ;
#20242 = CARTESIAN_POINT ( 'NONE',  ( 3.249999999999999556, 0.000000000000000000, 0.000000000000000000 ) ) ;
#20243 = ORIENTED_EDGE ( 'NONE', *, *, #21351, .T. ) ;
#20244 = B_SPLINE_CURVE_WITH_KNOTS ( 'NONE', 3,
 ( #32394, #24493, #6635, #17334, #27028, #1613, #12137, #29710, #6792, #9453 ),
 .UNSPECIFIED., .F., .F.,
 ( 4, 2, 2, 2, 4 ),
 ( -4.729241382666969782E-06, 0.0005792517583992173695, 0.0008712422582901617647, 0.001017237508235635697, 0.001163232758181109629 ),
 .UNSPECIFIED. ) ;
#20245 = CARTESIAN_POINT ( 'NONE',  ( 0.000000000000000000, -3.573533178329615367, 5.126388750707211450 ) ) ;
#20246 = ORIENTED_EDGE ( 'NONE', *, *, #15349, .F. ) ;
#20247 = CARTESIAN_POINT ( 'NONE',  ( -20.50218941644604698, 17.67398915370758772, 1.791940890631988692 ) ) ;
#20249 = ORIENTED_EDGE ( 'NONE', *, *, #11682, .T. ) ;
#20248 = CARTESIAN_POINT ( 'NONE',  ( 102.3469098519873626, -2.897175310220293731, -4.053847705497527265 ) ) ;
#20250 = ORIENTED_EDGE ( 'NONE', *, *, #12921, .T. ) ;
#20251 = CARTESIAN_POINT ( 'NONE',  ( 33.81874022276149816, 19.50000000000000000, 1.818740222761736414 ) ) ;
#20252 = CARTESIAN_POINT ( 'NONE',  ( -7.362550801365593145, -2.228590825266444586, -2.752080473201636401 ) ) ;
#20253 = FACE_OUTER_BOUND ( 'NONE', #29794, .T. ) ;
#20254 = EDGE_CURVE ( 'NONE', #20076, #30689, #12249, .T. ) ;
#20255 = CARTESIAN_POINT ( 'NONE',  ( 23.57316428367446548, -9.051964865574909425, -1.010822989962099960 ) ) ;
#20256 = CC_DESIGN_PERSON_AND_ORGANIZATION_ASSIGNMENT ( #4471, #21679, ( #3447 ) ) ;
#20258 = ORIENTED_EDGE ( 'NONE', *, *, #4891, .F. ) ;
#20257 = CARTESIAN_POINT ( 'NONE',  ( 10.52034268205830614, 3.024842911000689583, 3.993798362933319357 ) ) ;
#20259 = DIRECTION ( 'NONE',  ( -1.000000000000000000, 0.000000000000000000, -3.469446951953611033E-15 ) ) ;
#20260 = CARTESIAN_POINT ( 'NONE',  ( 2.482257818914018532, 0.000000000000000000, 1.712210361609934672 ) ) ;
#20261 =( BOUNDED_CURVE ( )  B_SPLINE_CURVE ( 3, ( #6239, #3741, #13906, #24121 ),
 .UNSPECIFIED., .F., .F. ) 
 B_SPLINE_CURVE_WITH_KNOTS ( ( 4, 4 ),
 ( 0.6009777071440908225, 1.570796326794896558 ),
 .UNSPECIFIED. ) 
 CURVE ( )  GEOMETRIC_REPRESENTATION_ITEM ( )  RATIONAL_B_SPLINE_CURVE ( ( 1.000000000000000000, 0.9231448173252605471, 0.9231448173252605471, 1.000000000000000000 ) ) 
 REPRESENTATION_ITEM ( '' )  );
#20262 = CARTESIAN_POINT ( 'NONE',  ( -3.789234217576226804, -9.307600915532304953, 1.743674089339463329 ) ) ;
#20263 = CARTESIAN_POINT ( 'NONE',  ( 8.254683653268546806, -1.057518490444498971, -1.500000000000000000 ) ) ;
#20265 = VERTEX_POINT ( 'NONE', #30182 ) ;
#20264 = DIRECTION ( 'NONE',  ( 0.1437473352844943209, 0.000000000000000000, -0.9896144216807913896 ) ) ;
#20266 = DIRECTION ( 'NONE',  ( 0.000000000000000000, 0.000000000000000000, -1.000000000000000000 ) ) ;
#20267 = CARTESIAN_POINT ( 'NONE',  ( 23.17250000273119070, 2.378061970571979433, -1.291182301015470602 ) ) ;
#20268 = DIRECTION ( 'NONE',  ( 0.000000000000000000, 0.000000000000000000, 1.000000000000000000 ) ) ;
#20269 = EDGE_CURVE ( 'NONE', #2610, #25225, #17607, .T. ) ;
#20270 = FACE_OUTER_BOUND ( 'NONE', #6226, .T. ) ;
#20271 = CARTESIAN_POINT ( 'NONE',  ( 6.037141752603385036, 8.462586328878536790, -0.4483113388088767470 ) ) ;
#20272 = CARTESIAN_POINT ( 'NONE',  ( 0.08034253656914176756, -9.429377841196146193, -5.242601083769383941 ) ) ;
#20273 = ORIENTED_EDGE ( 'NONE', *, *, #19652, .F. ) ;
#20274 = CARTESIAN_POINT ( 'NONE',  ( 46.69789307159569347, 25.15383447853596621, 4.629213727441585213 ) ) ;
#20275 = CARTESIAN_POINT ( 'NONE',  ( 56.97280603064898941, -277.2763395528616002, 0.4463807625373084065 ) ) ;
#20276 = CARTESIAN_POINT ( 'NONE',  ( -7.337550801365593678, 1.828967928396027398, -3.368539882008727115 ) ) ;
#20277 = ORIENTED_EDGE ( 'NONE', *, *, #25084, .T. ) ;
#20278 = VECTOR ( 'NONE', #7100, 1000.000000000000000 ) ;
#20279 = CARTESIAN_POINT ( 'NONE',  ( 25.67806763263881109, 1.420656155051234659, 2.597633682295764412 ) ) ;
#20280 = PLANE ( 'NONE',  #25308 ) ;
#20281 = FACE_OUTER_BOUND ( 'NONE', #32416, .T. ) ;
#20282 = VERTEX_POINT ( 'NONE', #17445 ) ;
#20283 = CARTESIAN_POINT ( 'NONE',  ( 0.000000000000000000, 20.00000000000000000, 6.818740222761507042 ) ) ;
#20284 = ORIENTED_EDGE ( 'NONE', *, *, #22905, .F. ) ;
#20285 = CARTESIAN_POINT ( 'NONE',  ( -40.49578753310456136, -13.12325744026704832, 5.486698823786521295 ) ) ;
#20286 = EDGE_LOOP ( 'NONE', ( #6242, #20960, #17915 ) ) ;
#20287 = CARTESIAN_POINT ( 'NONE',  ( -2.785986023666444211, -0.02407431902794407788, 1.185596063489961383 ) ) ;
#20289 = ORIENTED_EDGE ( 'NONE', *, *, #2436, .F. ) ;
#20288 = DIRECTION ( 'NONE',  ( 0.000000000000000000, 0.000000000000000000, -1.000000000000000000 ) ) ;
#20290 = ORIENTED_EDGE ( 'NONE', *, *, #30760, .T. ) ;
#20291 = CARTESIAN_POINT ( 'NONE',  ( 25.75999999999999801, -2.208672634433321348E-15, 0.000000000000000000 ) ) ;
#20292 = EDGE_CURVE ( 'NONE', #15269, #15578, #5242, .T. ) ;
#20294 = ORIENTED_EDGE ( 'NONE', *, *, #17352, .F. ) ;
#20293 = CIRCLE ( 'NONE', #30440, 5.010000000000000675 ) ;
#20295 = DIRECTION ( 'NONE',  ( 1.000000000000000000, 0.000000000000000000, 0.000000000000000000 ) ) ;
#20297 = ORIENTED_EDGE ( 'NONE', *, *, #21315, .F. ) ;
#20296 = CARTESIAN_POINT ( 'NONE',  ( 0.3277201397524639459, -5.271209332775584677, 1.500000000000000000 ) ) ;
#20298 = VECTOR ( 'NONE', #4746, 1000.000000000000000 ) ;
#20299 = CARTESIAN_POINT ( 'NONE',  ( 3.830085165118329002E-16, 4.467071865485494619, -1.625881193364653088 ) ) ;
#20300 = LINE ( 'NONE', #29558, #7541 ) ;
#20301 = DIRECTION ( 'NONE',  ( 1.000000000000000000, 0.000000000000000000, 0.000000000000000000 ) ) ;
#20302 = CYLINDRICAL_SURFACE ( 'NONE', #3925, 8.749000000000002331 ) ;
#20303 = TOROIDAL_SURFACE ( 'NONE', #24546, 10.51776515689528502, 0.5000000000000000000 ) ;
#20304 = CARTESIAN_POINT ( 'NONE',  ( -50.81000000000000227, -10.96999999999998643, 9.000000000000000000 ) ) ;
#20305 = CYLINDRICAL_SURFACE ( 'NONE', #27326, 6.000000000000001776 ) ;
#20306 = CARTESIAN_POINT ( 'NONE',  ( 24.36752972617692592, -17.44836528598961678, 1.442218785864448405 ) ) ;
#20307 = EDGE_CURVE ( 'NONE', #28679, #7524, #15482, .T. ) ;
#20308 = EDGE_CURVE ( 'NONE', #19305, #9887, #21360, .T. ) ;
#20309 = CARTESIAN_POINT ( 'NONE',  ( -4.176822952881705575, -3.225712836238914250, 0.9788672205877712029 ) ) ;
#20310 = FACE_OUTER_BOUND ( 'NONE', #19631, .T. ) ;
#20311 = DIRECTION ( 'NONE',  ( 0.000000000000000000, -0.4067366430757887730, -0.9135454576426058626 ) ) ;
#20312 = CARTESIAN_POINT ( 'NONE',  ( 109.4831014662949258, 20.77917954950597590, 0.4463807625372899768 ) ) ;
#20313 = EDGE_CURVE ( 'NONE', #17452, #4124, #8256, .T. ) ;
#20314 = VECTOR ( 'NONE', #30220, 999.9999999999998863 ) ;
#20315 = CARTESIAN_POINT ( 'NONE',  ( 3.499999999999999556, -1.471047635026823786, -6.892461014225975013 ) ) ;
#20316 = CARTESIAN_POINT ( 'NONE',  ( -2.950050802731187360, 0.3135853898029611342, -2.983565686104819648 ) ) ;
#20317 = ORIENTED_EDGE ( 'NONE', *, *, #3830, .F. ) ;
#20318 = CARTESIAN_POINT ( 'NONE',  ( -4.387550801365594388, -3.521866450007987037, -0.3701630799359323931 ) ) ;
#20319 = TOROIDAL_SURFACE ( 'NONE', #19234, 6.500000000000002665, 0.5000000000000000000 ) ;
#20320 = AXIS2_PLACEMENT_3D ( 'NONE', #21884, #6999, #16529 ) ;
#20321 = CARTESIAN_POINT ( 'NONE',  ( -3.672954038633582391E-13, 4.709950686175357504, 9.884132761439534676 ) ) ;
#20322 = CARTESIAN_POINT ( 'NONE',  ( 19.75018141867016297, -21.43174828998459702, -1.668660430087435254 ) ) ;
#20323 = ORIENTED_EDGE ( 'NONE', *, *, #20985, .F. ) ;
#20324 = CARTESIAN_POINT ( 'NONE',  ( 5.489321708267612898, -5.138670926724855370, -6.285661071314523340 ) ) ;
#20325 = AXIS2_PLACEMENT_3D ( 'NONE', #27988, #15096, #25313 ) ;
#20326 = ORIENTED_EDGE ( 'NONE', *, *, #17464, .F. ) ;
#20327 = DIRECTION ( 'NONE',  ( -1.000000000000000000, 0.000000000000000000, 0.000000000000000000 ) ) ;
#20328 = CALENDAR_DATE ( 2026, 6, 10 ) ;
#20330 = VERTEX_POINT ( 'NONE', #21126 ) ;
#20329 = CARTESIAN_POINT ( 'NONE',  ( 14.13431920379513862, -20.70626837987542856, -1.499999999999999556 ) ) ;
#20331 = ORIENTED_EDGE ( 'NONE', *, *, #16235, .F. ) ;
#20332 = CARTESIAN_POINT ( 'NONE',  ( -53.59739919106122841, 4.827917019894381490, 2.635056041638651703 ) ) ;
#20333 = ORIENTED_EDGE ( 'NONE', *, *, #3519, .F. ) ;
#20334 = DIRECTION ( 'NONE',  ( 0.000000000000000000, 0.000000000000000000, 1.000000000000000000 ) ) ;
#20336 = ORIENTED_EDGE ( 'NONE', *, *, #6249, .T. ) ;
#20335 = LINE ( 'NONE', #17642, #32590 ) ;
#20337 = CARTESIAN_POINT ( 'NONE',  ( 48.09670199522223299, -9.430894477034980738, 1.010822989962089746 ) ) ;
#20339 = DIRECTION ( 'NONE',  ( 1.000000000000000000, -0.000000000000000000, -0.000000000000000000 ) ) ;
#20338 = PERSON ( 'NAUO-PER1', 'UNSPECIFIED', 'UNSPECIFIED', ('UNSPECIFIED'), ('UNSPECIFIED'), ('UNSPECIFIED') ) ;
#20340 = CARTESIAN_POINT ( 'NONE',  ( 22.91474828513863216, -21.90304137343319724, -1.273718548422748231 ) ) ;
#20341 = FACE_OUTER_BOUND ( 'NONE', #20226, .T. ) ;
#20342 = CIRCLE ( 'NONE', #19256, 0.4500000000000016764 ) ;
#20343 = ADVANCED_FACE ( 'NONE', ( #28785 ), #29372, .T. ) ;
#20344 = ORIENTED_EDGE ( 'NONE', *, *, #18095, .F. ) ;
#20345 = AXIS2_PLACEMENT_3D ( 'NONE', #18035, #30599, #32777 ) ;
#20346 = B_SPLINE_CURVE_WITH_KNOTS ( 'NONE', 3,
 ( #14211, #4043, #32460, #6206, #26601, #3704 ),
 .UNSPECIFIED., .F., .F.,
 ( 4, 2, 4 ),
 ( 2.626357090645241657E-13, 0.0003954463998646022939, 0.0007908927994665688630 ),
 .UNSPECIFIED. ) ;
#20347 = DIRECTION ( 'NONE',  ( -0.000000000000000000, 0.000000000000000000, 1.000000000000000000 ) ) ;
#20348 = CARTESIAN_POINT ( 'NONE',  ( 23.68064580653238949, -7.171681651382474598, 4.522129901861162260 ) ) ;
#20349 = CARTESIAN_POINT ( 'NONE',  ( 11.04311965146451158, 15.00000000000000178, 1.508259000770581615 ) ) ;
#20350 = CARTESIAN_POINT ( 'NONE',  ( 29.38825086720286350, -3.456623792451285482, -2.713652344655540727 ) ) ;
#20351 = CIRCLE ( 'NONE', #588, 5.009999999999999787 ) ;
#20352 = CARTESIAN_POINT ( 'NONE',  ( 24.70609432061683464, -17.48198453993439117, 1.498641547862707979 ) ) ;
#20353 = DIRECTION ( 'NONE',  ( 0.000000000000000000, 0.000000000000000000, 1.000000000000000000 ) ) ;
#20354 = DIRECTION ( 'NONE',  ( 1.000000000000000000, -0.000000000000000000, -0.000000000000000000 ) ) ;
#20355 = CARTESIAN_POINT ( 'NONE',  ( 23.18045508973627378, -21.93188832360367257, 1.140730425197365561 ) ) ;
#20356 = ORIENTED_EDGE ( 'NONE', *, *, #14084, .T. ) ;
#20357 = CARTESIAN_POINT ( 'NONE',  ( -7.412550801365592967, -3.368539882008727115, -1.828967928396028064 ) ) ;
#20358 = ORIENTED_EDGE ( 'NONE', *, *, #18173, .T. ) ;
#20359 = CARTESIAN_POINT ( 'NONE',  ( -4.604531657079157014, -1.883076972206379818, -2.325406398514292761 ) ) ;
#20360 = CARTESIAN_POINT ( 'NONE',  ( 22.86000000136559507, 1.570731468192929858, 2.892927487894329186 ) ) ;
#20361 = CIRCLE ( 'NONE', #10202, 5.000000000000000888 ) ;
#20362 = DIRECTION ( 'NONE',  ( 0.000000000000000000, 0.7071067811865507924, 0.7071067811865441310 ) ) ;
#20363 = CARTESIAN_POINT ( 'NONE',  ( 0.2024771939337984550, -5.520608663253200099, 1.770108805539934327 ) ) ;
#20364 = CARTESIAN_POINT ( 'NONE',  ( 108.3924980168111745, 20.36374375480692578, 1.424458110042542192 ) ) ;
#20365 = ORIENTED_EDGE ( 'NONE', *, *, #17508, .F. ) ;
#20366 = DIRECTION ( 'NONE',  ( -0.1908089953765452762, 0.000000000000000000, -0.9816271834476639757 ) ) ;
#20367 = VECTOR ( 'NONE', #3100, 1000.000000000000114 ) ;
#20368 = AXIS2_PLACEMENT_3D ( 'NONE', #14816, #28047, #20533 ) ;
#20369 = VECTOR ( 'NONE', #23152, 1000.000000000000000 ) ;
#20370 = CARTESIAN_POINT ( 'NONE',  ( 102.6609843814833027, -1.982062027707615082, -4.522129901861162260 ) ) ;
#20371 = ORIENTED_EDGE ( 'NONE', *, *, #41, .T. ) ;
#20372 = CARTESIAN_POINT ( 'NONE',  ( 5.885541615502093649, 1.821712961073348014, 8.193643496140859739 ) ) ;
#20373 = SHAPE_DEFINITION_REPRESENTATION ( #22298, #8974 ) ;
#20374 = CARTESIAN_POINT ( 'NONE',  ( 69.06873112120143787, -6.081964788647525211, 4.043901188644938749 ) ) ;
#20375 = AXIS2_PLACEMENT_3D ( 'NONE', #1069, #3746, #29005 ) ;
#20376 = VECTOR ( 'NONE', #28429, 1000.000000000000227 ) ;
#20377 = LINE ( 'NONE', #7482, #15498 ) ;
#20379 = CARTESIAN_POINT ( 'NONE',  ( 10.55147673363119054, 4.116875700062082366, 2.376879293651078751 ) ) ;
#20378 = CARTESIAN_POINT ( 'NONE',  ( 10.00000000000000000, 2.376879293651063652, 4.116875700062091248 ) ) ;
#20380 = EDGE_CURVE ( 'NONE', #32842, #25696, #8402, .T. ) ;
#20381 = EDGE_LOOP ( 'NONE', ( #16095, #12037, #29789, #2647 ) ) ;
#20382 = DIRECTION ( 'NONE',  ( -0.000000000000000000, -0.000000000000000000, 1.000000000000000000 ) ) ;
#20383 = CARTESIAN_POINT ( 'NONE',  ( 22.98500000136559507, -0.9349337715887248157, 3.156283516753367824 ) ) ;
#20384 = CARTESIAN_POINT ( 'NONE',  ( 18.48753670594055976, -16.70790065660999346, -1.499999999999860334 ) ) ;
#20385 = EDGE_CURVE ( 'NONE', #6820, #31424, #18942, .T. ) ;
#20387 = VERTEX_POINT ( 'NONE', #26468 ) ;
#20386 = CARTESIAN_POINT ( 'NONE',  ( 107.6876975323875740, 19.28758966828627663, 4.774517761658953141 ) ) ;
#20388 = CARTESIAN_POINT ( 'NONE',  ( -6.712550801365593678, -3.675193018007246071, 1.088641768524163167 ) ) ;
#20389 = CARTESIAN_POINT ( 'NONE',  ( 107.9391918483597550, 17.83955614279767588, -3.592051012467005755 ) ) ;
#20390 = AXIS2_PLACEMENT_3D ( 'NONE', #12232, #21776, #26973 ) ;
#20391 = CARTESIAN_POINT ( 'NONE',  ( -53.96125734831202436, 5.502033201759978454, 1.127224778417299067 ) ) ;
#20393 = EDGE_CURVE ( 'NONE', #8056, #32762, #18275, .T. ) ;
#20392 = FACE_OUTER_BOUND ( 'NONE', #11026, .T. ) ;
#20394 = ORIENTED_EDGE ( 'NONE', *, *, #8993, .T. ) ;
#20396 = ORIENTED_EDGE ( 'NONE', *, *, #12628, .F. ) ;
#20395 = CARTESIAN_POINT ( 'NONE',  ( 24.05790257984262226, -17.31116499701224853, 1.379149890412948221 ) ) ;
#20397 = VECTOR ( 'NONE', #27695, 1000.000000000000114 ) ;
#20398 = CIRCLE ( 'NONE', #24639, 8.750000000000000000 ) ;
#20399 = CARTESIAN_POINT ( 'NONE',  ( 23.67724090058426611, -17.25947716274855281, -1.422757073343587919 ) ) ;
#20400 = CARTESIAN_POINT ( 'NONE',  ( -60.52311629951223892, -10.96999999999998820, 8.628141679950115162 ) ) ;
#20401 = CIRCLE ( 'NONE', #30552, 4.000000000000001776 ) ;
#20402 = EDGE_CURVE ( 'NONE', #6314, #24805, #21874, .T. ) ;
#20403 = CARTESIAN_POINT ( 'NONE',  ( 21.92250000136559507, 0.3178988483021036315, 3.024605502323848949 ) ) ;
#20404 = AXIS2_PLACEMENT_3D ( 'NONE', #31688, #3595, #21637 ) ;
#20405 = CARTESIAN_POINT ( 'NONE',  ( -29.99064796452623582, 9.298459344133517490, 1.499999999996624700 ) ) ;
#20406 = CARTESIAN_POINT ( 'NONE',  ( 7.453146289620847575, -19.12801665242071181, -1.500000000000000444 ) ) ;
#20407 = VECTOR ( 'NONE', #4518, 999.9999999999998863 ) ;
#20408 = CARTESIAN_POINT ( 'NONE',  ( -23.54713438637982748, 8.429255322705477838, 8.219131494323725917 ) ) ;
#20409 = DIRECTION ( 'NONE',  ( 1.000000000000000000, -0.000000000000000000, 0.000000000000000000 ) ) ;
#20410 = CARTESIAN_POINT ( 'NONE',  ( 107.8806061109513763, -16.35011981546645998, 2.521000801048293383 ) ) ;
#20411 = ORIENTED_EDGE ( 'NONE', *, *, #30633, .F. ) ;
#20412 = FACE_OUTER_BOUND ( 'NONE', #21734, .T. ) ;
#20413 = ADVANCED_FACE ( 'NONE', ( #18449 ), #895, .T. ) ;
#20414 = AXIS2_PLACEMENT_3D ( 'NONE', #22408, #19930, #7213 ) ;
#20416 = CIRCLE ( 'NONE', #17725, 5.010000000000000675 ) ;
#20415 = CALENDAR_DATE ( 2026, 6, 10 ) ;
#20417 = CARTESIAN_POINT ( 'NONE',  ( 25.86240141410254978, 23.76612641949149562, 0.4463807625372899768 ) ) ;
#20418 = CIRCLE ( 'NONE', #10866, 8.500000000000000000 ) ;
#20419 = VERTEX_POINT ( 'NONE', #18596 ) ;
#20420 = CARTESIAN_POINT ( 'NONE',  ( 108.1273904054188080, 18.88751996810619715, -5.041740218227376502 ) ) ;
#20421 = VECTOR ( 'NONE', #12152, 1000.000000000000114 ) ;
#20422 = VERTEX_POINT ( 'NONE', #15775 ) ;
#20423 = CARTESIAN_POINT ( 'NONE',  ( -23.08960572693444036, 4.011204475888708210, 2.145824749606468185 ) ) ;
#20425 = ORIENTED_EDGE ( 'NONE', *, *, #12115, .F. ) ;
#20424 = CARTESIAN_POINT ( 'NONE',  ( 69.01370136936026256, -4.979762270910514488, -4.008637876656666599 ) ) ;
#20426 = ORIENTED_EDGE ( 'NONE', *, *, #15050, .T. ) ;
#20427 = VECTOR ( 'NONE', #20366, 999.9999999999998863 ) ;
#20428 = CARTESIAN_POINT ( 'NONE',  ( 6.655951778521610684, -18.71196003547629516, -1.500000000000000000 ) ) ;
#20429 = CARTESIAN_POINT ( 'NONE',  ( -7.212550801365594566, 1.828967928396027398, -3.368539882008727115 ) ) ;
#20430 = CARTESIAN_POINT ( 'NONE',  ( 7.064632918400242545, -8.437262856154175594, 2.318425219014201843 ) ) ;
#20431 = AXIS2_PLACEMENT_3D ( 'NONE', #6367, #1216, #23928 ) ;
#20432 = CARTESIAN_POINT ( 'NONE',  ( 85.49734435724778336, -7.913007294147514692, -0.07017451552783579571 ) ) ;
#20434 = ORIENTED_EDGE ( 'NONE', *, *, #9493, .F. ) ;
#20433 = LINE ( 'NONE', #30650, #17095 ) ;
#20435 = DIRECTION ( 'NONE',  ( 0.000000000000000000, 0.000000000000000000, -1.000000000000000000 ) ) ;
#20436 = CARTESIAN_POINT ( 'NONE',  ( 25.73747082620503690, 18.89898602765365609, 1.050000000000000044 ) ) ;
#20437 = CARTESIAN_POINT ( 'NONE',  ( -3.353579435673377240, -11.46043295930974004, 1.499999999999999112 ) ) ;
#20438 = EDGE_CURVE ( 'NONE', #7241, #18979, #12265, .T. ) ;
#20439 = DIRECTION ( 'NONE',  ( 0.000000000000000000, 1.000000000000000000, 0.000000000000000000 ) ) ;
#20441 = ORIENTED_EDGE ( 'NONE', *, *, #24827, .T. ) ;
#20440 = CARTESIAN_POINT ( 'NONE',  ( 108.0614315348869781, -18.95396093674897386, -4.509855988468532750 ) ) ;
#20442 = EDGE_CURVE ( 'NONE', #17869, #5840, #25977, .T. ) ;
#20443 = FACE_OUTER_BOUND ( 'NONE', #6199, .T. ) ;
#20444 = VECTOR ( 'NONE', #1580, 1000.000000000000114 ) ;
#20445 = VECTOR ( 'NONE', #18089, 1000.000000000000000 ) ;
#20446 = CARTESIAN_POINT ( 'NONE',  ( -25.77866645709989513, 18.05832575017197428, 1.782687067521398605 ) ) ;
#20447 = CARTESIAN_POINT ( 'NONE',  ( 23.79750000273118715, -2.594547506269383685, -0.7685399846772043020 ) ) ;
#20448 = EDGE_CURVE ( 'NONE', #697, #25155, #21462, .T. ) ;
#20449 = AXIS2_PLACEMENT_3D ( 'NONE', #3030, #2680, #15861 ) ;
#20450 = FACE_OUTER_BOUND ( 'NONE', #3143, .T. ) ;
#20451 = VECTOR ( 'NONE', #16050, 1000.000000000000000 ) ;
#20452 = CARTESIAN_POINT ( 'NONE',  ( 5.377543748152548986, 8.014274990069656823, -8.669741416787380218E-17 ) ) ;
#20453 = CARTESIAN_POINT ( 'NONE',  ( 0.1574692315735313208, -9.238013023060274165, -5.243558859478258505 ) ) ;
#20454 = ORIENTED_EDGE ( 'NONE', *, *, #27117, .T. ) ;
#20455 = CARTESIAN_POINT ( 'NONE',  ( 7.249760686538667009, 7.892520144992453801, -1.391664247347147443 ) ) ;
#20456 = AXIS2_PLACEMENT_3D ( 'NONE', #28793, #20791, #22513 ) ;
#20457 = CIRCLE ( 'NONE', #18850, 2.999999999999999556 ) ;
#20458 = CARTESIAN_POINT ( 'NONE',  ( -50.60000000000000142, -0.5000000000000000000, -1.500000000000000000 ) ) ;
#20459 = CARTESIAN_POINT ( 'NONE',  ( -5.837550801365592790, -1.088641768524163611, -3.675193018007245627 ) ) ;
#20460 = ORIENTED_EDGE ( 'NONE', *, *, #8432, .T. ) ;
#20461 = VECTOR ( 'NONE', #32139, 1000.000000000000000 ) ;
#20462 = EDGE_CURVE ( 'NONE', #20953, #7325, #2939, .T. ) ;
#20463 = CC_DESIGN_DATE_AND_TIME_ASSIGNMENT ( #5772, #31507, ( #21588 ) ) ;
#20464 = CARTESIAN_POINT ( 'NONE',  ( 3.063284526839887167, -8.461683424509331530, 2.223716399045538861 ) ) ;
#20465 = DIRECTION ( 'NONE',  ( -1.000000000000000000, 8.574039729943022041E-17, -0.000000000000000000 ) ) ;
#20466 = CARTESIAN_POINT ( 'NONE',  ( 2.889143798718251333, 0.000000000000000000, -0.9788672205888330202 ) ) ;
#20467 = CARTESIAN_POINT ( 'NONE',  ( 29.18953645666585217, -9.308308156628569918, -0.07017451552783579571 ) ) ;
#20468 = ORIENTED_EDGE ( 'NONE', *, *, #10979, .F. ) ;
#20469 = VECTOR ( 'NONE', #22516, 1000.000000000000000 ) ;
#20470 = CARTESIAN_POINT ( 'NONE',  ( -40.73291413977247544, -13.73842845495894593, 5.444121653534940819 ) ) ;
#20471 = ORIENTED_EDGE ( 'NONE', *, *, #11850, .T. ) ;
#20472 = CARTESIAN_POINT ( 'NONE',  ( 0.000000000000000000, 5.222868219166995729, -9.680994141368712391 ) ) ;
#20473 = PRODUCT_DEFINITION_SHAPE ( 'NONE', 'NONE',  #33102 ) ;
#20474 = TOROIDAL_SURFACE ( 'NONE', #18861, 298.6457063863958865, 5.000000000000000888 ) ;
#20476 = EDGE_LOOP ( 'NONE', ( #6298, #7738, #16859, #9021, #9419, #28210 ) ) ;
#20475 = DIRECTION ( 'NONE',  ( -1.000000000000000000, 8.574039729943022041E-17, 6.162975822039154730E-33 ) ) ;
#20477 = ORIENTED_EDGE ( 'NONE', *, *, #19321, .T. ) ;
#20478 = CARTESIAN_POINT ( 'NONE',  ( 2.671540748214986660, 0.5000000000000006661, -1.500000000000000000 ) ) ;
#20479 = VECTOR ( 'NONE', #8347, 1000.000000000000114 ) ;
#20480 = CIRCLE ( 'NONE', #11390, 10.01776515689528502 ) ;
#20481 = CIRCLE ( 'NONE', #10321, 10.99999999999999822 ) ;
#20482 = ORIENTED_EDGE ( 'NONE', *, *, #24487, .T. ) ;
#20483 = CARTESIAN_POINT ( 'NONE',  ( 5.885541806331895387, -7.076443837533989090, 4.514241479885522601 ) ) ;
#20485 = EDGE_LOOP ( 'NONE', ( #14760, #543, #13152, #4907 ) ) ;
#20484 = CARTESIAN_POINT ( 'NONE',  ( 0.3277201397524639459, -5.271209332775584677, -1.500000000000000000 ) ) ;
#20486 = CARTESIAN_POINT ( 'NONE',  ( -5.650050800000001594, -1.549418761218565255, 2.853674364686380471 ) ) ;
#20487 = CARTESIAN_POINT ( 'NONE',  ( 2.274274201627632053, 10.82112760146237029, 1.975651141464422000 ) ) ;
#20488 = EDGE_CURVE ( 'NONE', #8885, #31265, #5137, .T. ) ;
#20489 = DIRECTION ( 'NONE',  ( 0.000000000000000000, -0.08715574274766962892, 0.9961946980917446570 ) ) ;
#20490 = CARTESIAN_POINT ( 'NONE',  ( 0.000000000000000000, 0.000000000000000000, 6.000000000000000000 ) ) ;
#20491 = CARTESIAN_POINT ( 'NONE',  ( 7.064632816082964339, 8.721381771256204729, 0.7071067811865412445 ) ) ;
#20492 = CARTESIAN_POINT ( 'NONE',  ( 0.9078783126652600899, -4.283561563640669867, 1.499999999999999778 ) ) ;
#20493 = CARTESIAN_POINT ( 'NONE',  ( 1.624999999999999778, 7.593217523260583413, 7.958834565716794707 ) ) ;
#20494 = CARTESIAN_POINT ( 'NONE',  ( 10.00000000000000000, -2.718385644597145046, -4.208382051008221936 ) ) ;
#20495 = CARTESIAN_POINT ( 'NONE',  ( 68.79832465278998654, -7.861404707920828905, -0.07017451552783579571 ) ) ;
#20496 = AXIS2_PLACEMENT_3D ( 'NONE', #23342, #446, #10628 ) ;
#20497 = CARTESIAN_POINT ( 'NONE',  ( -5.749676575031998027, 8.479088208361000873E-16, 6.923700951379999857 ) ) ;
#20498 = CARTESIAN_POINT ( 'NONE',  ( 54.64624227588102201, -3.635739347938792054, -0.02339150518254430253 ) ) ;
#20499 = VECTOR ( 'NONE', #14498, 1000.000000000000000 ) ;
#20500 = CARTESIAN_POINT ( 'NONE',  ( 10.55147673363118876, -4.116875700062067267, -2.376879293651108060 ) ) ;
#20501 = CARTESIAN_POINT ( 'NONE',  ( -3.700050802731187805, 1.549418761218566143, -2.853674364686379583 ) ) ;
#20502 = ORIENTED_EDGE ( 'NONE', *, *, #19267, .F. ) ;
#20503 = TOROIDAL_SURFACE ( 'NONE', #8739, 5.500000000000000000, 0.5000000000000000000 ) ;
#20504 = CARTESIAN_POINT ( 'NONE',  ( -5.537550801365594744, 3.368539882008727115, 1.828967928396026954 ) ) ;
#20505 = ADVANCED_FACE ( 'NONE', ( #6066 ), #5592, .T. ) ;
#20506 = CARTESIAN_POINT ( 'NONE',  ( 10.00000000000000000, 5.003758587302148619, -0.2499999999999991951 ) ) ;
#20507 = CARTESIAN_POINT ( 'NONE',  ( 6.749760686538667009, 6.735557395310442023E-16, -5.500000000000000000 ) ) ;
#20508 = APPROVAL_PERSON_ORGANIZATION ( #21830, #6550, #29545 ) ;
#20509 = EDGE_LOOP ( 'NONE', ( #14160, #2940, #9060, #28097 ) ) ;
#20510 = CARTESIAN_POINT ( 'NONE',  ( 102.5305753040692878, -0.1042037546421146210, -0.07017451552781628354 ) ) ;
#20511 = ORIENTED_EDGE ( 'NONE', *, *, #24743, .T. ) ;
#20512 = CARTESIAN_POINT ( 'NONE',  ( 69.09268213438589612, -2.232183665269756645, -1.010822989962086416 ) ) ;
#20513 = CALENDAR_DATE ( 2026, 6, 10 ) ;
#20515 = VERTEX_POINT ( 'NONE', #28486 ) ;
#20514 = CARTESIAN_POINT ( 'NONE',  ( 74.30107678963170770, -22.79527490385382649, -1.499999999999999556 ) ) ;
#20516 = ORIENTED_EDGE ( 'NONE', *, *, #14443, .F. ) ;
#20517 = CARTESIAN_POINT ( 'NONE',  ( -2.160548182721718113, -12.59940861538154167, 1.743857535748950971 ) ) ;
#20518 = EDGE_CURVE ( 'NONE', #5453, #15485, #22957, .T. ) ;
#20519 = ORIENTED_EDGE ( 'NONE', *, *, #21047, .F. ) ;
#20520 = DIRECTION ( 'NONE',  ( 0.000000000000000000, 0.000000000000000000, 1.000000000000000000 ) ) ;
#20521 = AXIS2_PLACEMENT_3D ( 'NONE', #6306, #1328, #8972 ) ;
#20523 = ORIENTED_EDGE ( 'NONE', *, *, #27316, .T. ) ;
#20522 = CARTESIAN_POINT ( 'NONE',  ( -54.10469650629801919, 5.263418255572274163, 1.500000000000000000 ) ) ;
#20524 = AXIS2_PLACEMENT_3D ( 'NONE', #10474, #30888, #5638 ) ;
#20525 = CARTESIAN_POINT ( 'NONE',  ( 102.9361373302715918, -5.944196040818414239, 2.713652344655544724 ) ) ;
#20526 = CARTESIAN_POINT ( 'NONE',  ( 3.529825581556955655E-16, 4.116875700062116117, -2.376879293651021019 ) ) ;
#20527 = ADVANCED_FACE ( 'NONE', ( #735 ), #13715, .F. ) ;
#20528 = CARTESIAN_POINT ( 'NONE',  ( 21.78705206151444074, -21.77640818797000932, -1.495779539311291817 ) ) ;
#20529 = CARTESIAN_POINT ( 'NONE',  ( 3.249999999999999556, -6.772677083992426184, 5.538577986808876474 ) ) ;
#20530 = ORIENTED_EDGE ( 'NONE', *, *, #26506, .F. ) ;
#20531 = DIRECTION ( 'NONE',  ( -0.000000000000000000, 0.000000000000000000, 1.000000000000000000 ) ) ;
#20532 = CARTESIAN_POINT ( 'NONE',  ( 7.249760686538667009, -8.014274990069656823, 8.669741416787380218E-17 ) ) ;
#20533 = DIRECTION ( 'NONE',  ( 0.000000000000000000, 0.9659258262890678681, 0.2588190451025219052 ) ) ;
#20534 = DIRECTION ( 'NONE',  ( 4.917867153433032926E-17, 0.5735764363510501562, -0.8191520442889889120 ) ) ;
#20535 = ORGANIZATION ( 'NAUO-ORG6', 'UNSPECIFIED', 'UNSPECIFIED' ) ;
#20536 = CARTESIAN_POINT ( 'NONE',  ( -7.998722633285748174, -2.371517779863575370, 1.837526800715260533 ) ) ;
#20537 = CARTESIAN_POINT ( 'NONE',  ( 108.1300413742128228, -19.95926608421481063, -1.392287898180229133 ) ) ;
#20538 = CARTESIAN_POINT ( 'NONE',  ( 24.00111451137534146, -6.623356326098185375E-16, -2.499999999999998224 ) ) ;
#20539 = DIRECTION ( 'NONE',  ( 0.000000000000000000, -0.000000000000000000, -1.000000000000000000 ) ) ;
#20540 = ORIENTED_EDGE ( 'NONE', *, *, #8723, .T. ) ;
#20541 = CARTESIAN_POINT ( 'NONE',  ( -7.662550801365593856, -0.3701630799359326152, 3.521866450007987037 ) ) ;
#20542 = VERTEX_POINT ( 'NONE', #30052 ) ;
#20543 = CARTESIAN_POINT ( 'NONE',  ( -3.054531657079158080, -2.846291840500172921, -1.545410377633947618 ) ) ;
#20544 =( BOUNDED_CURVE ( )  B_SPLINE_CURVE ( 3, ( #31924, #11842, #29396, #27211 ),
 .UNSPECIFIED., .F., .F. ) 
 B_SPLINE_CURVE_WITH_KNOTS ( ( 4, 4 ),
 ( 0.1919862177193129571, 1.570796326794901887 ),
 .UNSPECIFIED. ) 
 CURVE ( )  GEOMETRIC_REPRESENTATION_ITEM ( )  RATIONAL_B_SPLINE_CURVE ( ( 1.000000000000000000, 0.8477497222584654546, 0.8477497222584654546, 1.000000000000000000 ) ) 
 REPRESENTATION_ITEM ( '' )  );
#20545 = AXIS2_PLACEMENT_3D ( 'NONE', #16959, #1285, #8791 ) ;
#20546 = CARTESIAN_POINT ( 'NONE',  ( 108.0970801781586772, 18.71874066288092564, 5.127126610281505847 ) ) ;
#20547 = CARTESIAN_POINT ( 'NONE',  ( 3.285049811803533171, 7.727496690442961710E-33, -1.174877964933951802 ) ) ;
#20548 = CARTESIAN_POINT ( 'NONE',  ( 9.851448552576139051, -11.91728849018574721, 1.000000000000000000 ) ) ;
#20549 = ORIENTED_EDGE ( 'NONE', *, *, #23193, .T. ) ;
#20550 = DIRECTION ( 'NONE',  ( -1.000000000000000000, 0.000000000000000000, -0.000000000000000000 ) ) ;
#20552 = ORIENTED_EDGE ( 'NONE', *, *, #1402, .T. ) ;
#20551 = B_SPLINE_CURVE_WITH_KNOTS ( 'NONE', 3,
 ( #30962, #8044, #27620, #2212 ),
 .UNSPECIFIED., .F., .F.,
 ( 4, 4 ),
 ( 0.01682050255738576708, 0.01682075285862154324 ),
 .UNSPECIFIED. ) ;
#20553 = CARTESIAN_POINT ( 'NONE',  ( 3.063284526845908129, -0.4999240074859571670, -8.734705317652709411 ) ) ;
#20554 = CALENDAR_DATE ( 2026, 6, 10 ) ;
#20555 = CARTESIAN_POINT ( 'NONE',  ( 18.76206016059314763, -5.836912598754047998, 4.053847714184954931 ) ) ;
#20556 = ADVANCED_FACE ( 'NONE', ( #30221 ), #23060, .T. ) ;
#20557 = EDGE_CURVE ( 'NONE', #28620, #32499, #7900, .T. ) ;
#20558 = DIRECTION ( 'NONE',  ( 0.000000000000000000, 0.000000000000000000, 1.000000000000000000 ) ) ;
#20560 = CARTESIAN_POINT ( 'NONE',  ( 6.880159329304569304, 7.110803091624058325, 5.066480354148957588 ) ) ;
#20559 = DIRECTION ( 'NONE',  ( 0.000000000000000000, -0.8660254037844433705, 0.4999999999999920064 ) ) ;
#20561 = ORIENTED_EDGE ( 'NONE', *, *, #21077, .F. ) ;
#20562 = DIRECTION ( 'NONE',  ( -1.000000000000000000, 8.574039729943017111E-17, -0.000000000000000000 ) ) ;
#20563 = LINE ( 'NONE', #10161, #19287 ) ;
#20564 = CARTESIAN_POINT ( 'NONE',  ( 24.29750000136559507, -2.363507492473152283, -1.913930629741525280 ) ) ;
#20565 = DIRECTION ( 'NONE',  ( 0.000000000000000000, 0.2079116908177532363, 0.9781476007338069101 ) ) ;
#20567 = ORIENTED_EDGE ( 'NONE', *, *, #12809, .F. ) ;
#20566 = CARTESIAN_POINT ( 'NONE',  ( 12.65465643788354200, -15.70291107026620914, 1.500000000000000444 ) ) ;
#20568 = AXIS2_PLACEMENT_3D ( 'NONE', #11736, #18959, #11577 ) ;
#20569 = CARTESIAN_POINT ( 'NONE',  ( -6.062550801365593323, -0.3701630799359326152, 3.521866450007987037 ) ) ;
#20570 = CARTESIAN_POINT ( 'NONE',  ( 1.624999999999999778, -10.90201369670499965, 1.464956435139505908 ) ) ;
#20571 = CARTESIAN_POINT ( 'NONE',  ( 24.35832023931450507, -17.33818253687174860, -1.317734466820339900 ) ) ;
#20572 = LINE ( 'NONE', #22387, #25145 ) ;
#20573 = EDGE_LOOP ( 'NONE', ( #17240, #15548, #4854, #25575 ) ) ;
#20574 = ORIENTED_EDGE ( 'NONE', *, *, #16464, .T. ) ;
#20575 = CARTESIAN_POINT ( 'NONE',  ( 7.249760686538667009, -6.139290821770289064, 5.151476664237455871 ) ) ;
#20576 = DIRECTION ( 'NONE',  ( -0.2951703194034052125, 0.3797261271633437518, 0.8767454310646960458 ) ) ;
#20577 = EDGE_CURVE ( 'NONE', #2638, #21128, #13136, .T. ) ;
#20578 = CARTESIAN_POINT ( 'NONE',  ( 10.00000000000000000, -1.745506336992504507E-14, 4.753758587302147731 ) ) ;
#20579 = CARTESIAN_POINT ( 'NONE',  ( 28.70307564580985371, -5.239617037324004301, 3.390608483623311908 ) ) ;
#20580 = DIRECTION ( 'NONE',  ( 0.000000000000000000, 0.2923717047227409882, -0.9563047559630342143 ) ) ;
#20581 = CARTESIAN_POINT ( 'NONE',  ( 10.00000000000000000, 3.055657119358800244, 3.641590349731939735 ) ) ;
#20582 = CARTESIAN_POINT ( 'NONE',  ( -23.35000000000000142, -10.96966150227469505, 4.500000000000000888 ) ) ;
#20583 = CARTESIAN_POINT ( 'NONE',  ( 18.61776180080997989, -7.449878658335503445, 1.169950778988562146 ) ) ;
#20584 = ORIENTED_EDGE ( 'NONE', *, *, #3636, .F. ) ;
#20585 = CARTESIAN_POINT ( 'NONE',  ( 2.592584925145450470, 7.731606906650982047, -6.844296717726155777 ) ) ;
#20586 = ADVANCED_FACE ( 'NONE', ( #22693 ), #2620, .T. ) ;
#20587 = PERSON_AND_ORGANIZATION ( #6766, #25292 ) ;
#20588 = CARTESIAN_POINT ( 'NONE',  ( 23.90742340929273624, -3.204431202270332513, 2.713652344655542503 ) ) ;
#20589 = ORIENTED_EDGE ( 'NONE', *, *, #15371, .F. ) ;
#20590 = ADVANCED_FACE ( 'NONE', ( #2296 ), #7443, .T. ) ;
#20591 = FACE_OUTER_BOUND ( 'NONE', #4586, .T. ) ;
#20592 = EDGE_LOOP ( 'NONE', ( #12699, #25470, #11630, #12376 ) ) ;
#20593 = CARTESIAN_POINT ( 'NONE',  ( -21.75451829708082840, 4.263352738049903223, 2.138819418443957066 ) ) ;
#20595 = EDGE_LOOP ( 'NONE', ( #15608, #30938, #7009 ) ) ;
#20594 = CARTESIAN_POINT ( 'NONE',  ( 84.97362918700360979, -4.190265677326723726, -4.150065216340092178 ) ) ;
#20596 = EDGE_CURVE ( 'NONE', #9165, #14302, #5133, .T. ) ;
#20597 = ORIENTED_EDGE ( 'NONE', *, *, #29639, .T. ) ;
#20598 = DIRECTION ( 'NONE',  ( -0.000000000000000000, 0.000000000000000000, 1.000000000000000000 ) ) ;
#20599 = CARTESIAN_POINT ( 'NONE',  ( -7.912550801365592967, 3.675193018007246959, -1.088641768524161391 ) ) ;
#20600 = DIRECTION ( 'NONE',  ( 0.000000000000000000, 0.000000000000000000, -1.000000000000000000 ) ) ;
#20601 = DIRECTION ( 'NONE',  ( 0.000000000000000000, 0.8191520442889936859, -0.5735764363510434949 ) ) ;
#20603 = ORIENTED_EDGE ( 'NONE', *, *, #29017, .T. ) ;
#20602 = CARTESIAN_POINT ( 'NONE',  ( 0.000000000000000000, -4.724769925181202979, 4.089810527897742354 ) ) ;
#20604 = DIRECTION ( 'NONE',  ( -1.000000000000000000, 0.000000000000000000, -0.000000000000000000 ) ) ;
#20605 = FACE_OUTER_BOUND ( 'NONE', #11890, .T. ) ;
#20606 = EDGE_CURVE ( 'NONE', #5744, #32789, #13851, .T. ) ;
#20607 = CARTESIAN_POINT ( 'NONE',  ( 0.7297941506389588051, -15.54810501259861688, 1.500000000000000666 ) ) ;
#20609 = CARTESIAN_POINT ( 'NONE',  ( 25.61000000136559507, 3.156283516753366047, 0.9349337715887203748 ) ) ;
#20608 = APPLICATION_CONTEXT ( 'configuration controlled 3d designs of mechanical parts and assemblies' ) ;
#20610 = CARTESIAN_POINT ( 'NONE',  ( 107.3476768466457401, -15.88628154573096651, 1.500000000000000000 ) ) ;
#20612 = ORIENTED_EDGE ( 'NONE', *, *, #11623, .T. ) ;
#20611 = CARTESIAN_POINT ( 'NONE',  ( 108.0609297225750396, -18.94673496429123105, -4.529582879229646863 ) ) ;
#20613 = CARTESIAN_POINT ( 'NONE',  ( 25.75999999999999801, -5.000000000000005329, 6.123233995736770227E-16 ) ) ;
#20614 = DIRECTION ( 'NONE',  ( 0.000000000000000000, 1.000000000000000000, -1.224646799147353207E-16 ) ) ;
#20615 = CARTESIAN_POINT ( 'NONE',  ( 21.11000000136559152, -3.156283516753370044, -0.9349337715887220401 ) ) ;
#20616 = EDGE_CURVE ( 'NONE', #21332, #10245, #9601, .T. ) ;
#20617 = LINE ( 'NONE', #15756, #31629 ) ;
#20618 = CARTESIAN_POINT ( 'NONE',  ( 6.524594682510452159, 8.636529731786344755, -0.6222547417166852668 ) ) ;
#20619 = CARTESIAN_POINT ( 'NONE',  ( 2.382865613620175349, 0.000000000000000000, 1.508259000770581615 ) ) ;
#20620 = EDGE_LOOP ( 'NONE', ( #7846, #1215, #25427, #17390 ) ) ;
#20621 = DIRECTION ( 'NONE',  ( 0.000000000000000000, 0.9945218953682734009, 0.1045284632676534292 ) ) ;
#20622 = EDGE_CURVE ( 'NONE', #9701, #15924, #27220, .T. ) ;
#20623 = LINE ( 'NONE', #15761, #17754 ) ;
#20624 = CARTESIAN_POINT ( 'NONE',  ( 107.5183782604217129, -18.35318718675820904, -5.137737709513164219 ) ) ;
#20625 = ORIENTED_EDGE ( 'NONE', *, *, #28094, .F. ) ;
#20626 = CYLINDRICAL_SURFACE ( 'NONE', #29472, 8.500000000000000000 ) ;
#20627 = LINE ( 'NONE', #7396, #5565 ) ;
#20628 = EDGE_CURVE ( 'NONE', #25309, #18474, #21976, .T. ) ;
#20629 = CARTESIAN_POINT ( 'NONE',  ( 0.1962428234089072521, -6.885380501030516243, -1.500000000000000444 ) ) ;
#20630 = DIRECTION ( 'NONE',  ( 0.03488359650710501358, -0.9989355049964838695, -0.03018263660036204360 ) ) ;
#20631 = EDGE_CURVE ( 'NONE', #12982, #15020, #20335, .T. ) ;
#20632 = ORIENTED_EDGE ( 'NONE', *, *, #15967, .T. ) ;
#20633 = CARTESIAN_POINT ( 'NONE',  ( -40.76707995218932723, -13.06422702898852783, 5.564001359196309338 ) ) ;
#20634 = ORIENTED_EDGE ( 'NONE', *, *, #15787, .T. ) ;
#20635 = CARTESIAN_POINT ( 'NONE',  ( 3.063284526839890276, 0.4999240074895630048, -8.734705317681616066 ) ) ;
#20637 = ORIENTED_EDGE ( 'NONE', *, *, #29892, .F. ) ;
#20636 = CARTESIAN_POINT ( 'NONE',  ( -54.06000000000000227, -10.96999999999998643, 9.000000000000000000 ) ) ;
#20638 = VERTEX_POINT ( 'NONE', #2794 ) ;
#20639 = DIRECTION ( 'NONE',  ( -1.000000000000000000, 0.000000000000000000, 0.000000000000000000 ) ) ;
#20640 = EDGE_CURVE ( 'NONE', #28881, #6649, #11734, .T. ) ;
#20641 = ORIENTED_EDGE ( 'NONE', *, *, #5236, .F. ) ;
#20642 = DIRECTION ( 'NONE',  ( 0.9947025833170223263, 0.1027947991993880261, 0.000000000000000000 ) ) ;
#20644 = ORIENTED_EDGE ( 'NONE', *, *, #6221, .F. ) ;
#20643 = DIRECTION ( 'NONE',  ( -1.000000000000000000, -0.000000000000000000, 0.000000000000000000 ) ) ;
#20645 = ORIENTED_EDGE ( 'NONE', *, *, #21448, .T. ) ;
#20646 = CARTESIAN_POINT ( 'NONE',  ( 18.41217767841934716, -16.82117819851176677, -1.753330701571969907 ) ) ;
#20647 = CARTESIAN_POINT ( 'NONE',  ( 7.249760686538667009, 0.000000000000000000, 0.000000000000000000 ) ) ;
#20648 = DIRECTION ( 'NONE',  ( -0.000000000000000000, -0.000000000000000000, -1.000000000000000000 ) ) ;
#20649 = DIRECTION ( 'NONE',  ( 0.000000000000000000, 0.000000000000000000, 1.000000000000000000 ) ) ;
#20650 = DIRECTION ( 'NONE',  ( -1.000000000000000000, -0.000000000000000000, -0.000000000000000000 ) ) ;
#20651 = EDGE_CURVE ( 'NONE', #18222, #3046, #114, .T. ) ;
#20652 = CARTESIAN_POINT ( 'NONE',  ( 107.9227312540154458, 20.59779369625414347, 1.977410089419335826 ) ) ;
#20653 = CARTESIAN_POINT ( 'NONE',  ( 0.5630063594414467243, -7.169269592067868402, 1.500000000000000222 ) ) ;
#20654 = CARTESIAN_POINT ( 'NONE',  ( 10.00000000000000000, -0.8254815157535575487, 4.681538312723514395 ) ) ;
#20655 = CARTESIAN_POINT ( 'NONE',  ( 107.4500446874326940, -17.36019328965951303, -4.522129901861167589 ) ) ;
#20656 = LINE ( 'NONE', #15121, #1581 ) ;
#20657 = ADVANCED_FACE ( 'NONE', ( #10116 ), #30884, .F. ) ;
#20658 = CYLINDRICAL_SURFACE ( 'NONE', #20970, 2.999999999999998224 ) ;
#20659 = CARTESIAN_POINT ( 'NONE',  ( 23.84714171513300229, -3.444070612154822353, 0.07017451549163798707 ) ) ;
#20660 = DIRECTION ( 'NONE',  ( 0.000000000000000000, -0.4226182617406868403, -0.9063077870366558209 ) ) ;
#20661 = CARTESIAN_POINT ( 'NONE',  ( 10.00000000000000000, -1.775199859220255486E-14, 4.753758587302147731 ) ) ;
#20662 = EDGE_LOOP ( 'NONE', ( #11992, #30983, #28483, #3327 ) ) ;
#20663 = CARTESIAN_POINT ( 'NONE',  ( -7.287550801365593856, 2.752080473201636845, -2.228590825266444142 ) ) ;
#20664 = B_SPLINE_CURVE_WITH_KNOTS ( 'NONE', 3,
 ( #31037, #20829, #20683, #15467, #5289, #8299, #30886, #13451, #7636, #17838, #26177, #21008, #3283, #3129, #23492, #2983, #23339, #28685, #26023, #25675 ),
 .UNSPECIFIED., .F., .F.,
 ( 4, 2, 2, 2, 2, 2, 2, 2, 2, 4 ),
 ( -5.999999999908826955E-08, 0.003223665706961764427, 0.006447391413923528498, 0.009671117120885284330, 0.01128297997436616788, 0.01289484282784704797, 0.01611856853480881507, 0.01934229424177057524, 0.02256601994873234235, 0.02578974565569410252 ),
 .UNSPECIFIED. ) ;
#20665 = CARTESIAN_POINT ( 'NONE',  ( -41.39035047991316674, -16.40843718609402302, 2.028141679950118625 ) ) ;
#20666 = EDGE_CURVE ( 'NONE', #30035, #16750, #19873, .T. ) ;
#20667 = DIRECTION ( 'NONE',  ( 1.000000000000000000, 0.000000000000000000, -0.000000000000000000 ) ) ;
#20668 = VERTEX_POINT ( 'NONE', #598 ) ;
#20669 = CARTESIAN_POINT ( 'NONE',  ( 56.97280603064898941, -277.2763395528616002, 0.4463807625372899768 ) ) ;
#20670 =( LENGTH_UNIT ( ) NAMED_UNIT ( * ) SI_UNIT ( .MILLI., .METRE. ) );
#20671 = EDGE_CURVE ( 'NONE', #21342, #16032, #6116, .T. ) ;
#20672 = ORIENTED_EDGE ( 'NONE', *, *, #12537, .F. ) ;
#20673 = DIRECTION ( 'NONE',  ( 8.574039729943018344E-17, 1.000000000000000000, 0.000000000000000000 ) ) ;
#20674 = APPROVAL_ROLE ( '' ) ;
#20676 = VERTEX_POINT ( 'NONE', #18637 ) ;
#20675 = CARTESIAN_POINT ( 'NONE',  ( -1.218076164763124636, -14.00532792343563848, -1.499999999999999556 ) ) ;
#20677 = EDGE_LOOP ( 'NONE', ( #29470, #18326, #13511, #14514 ) ) ;
#20678 = CARTESIAN_POINT ( 'NONE',  ( -3.406057470504892493, -10.41438730896155462, 1.743528078589993147 ) ) ;
#20679 = ORIENTED_EDGE ( 'NONE', *, *, #447, .F. ) ;
#20680 = DIRECTION ( 'NONE',  ( -1.000000000000000000, -0.000000000000000000, -0.000000000000000000 ) ) ;
#20682 = ORIENTED_EDGE ( 'NONE', *, *, #4252, .T. ) ;
#20681 = CARTESIAN_POINT ( 'NONE',  ( 3.499999999999999556, 0.000000000000000000, 0.000000000000000000 ) ) ;
#20683 = CARTESIAN_POINT ( 'NONE',  ( 24.14778831125731884, 18.13365127247671538, 1.049999999999999822 ) ) ;
#20684 = LINE ( 'NONE', #13285, #22983 ) ;
#20685 = DIRECTION ( 'NONE',  ( 0.000000000000000000, 0.000000000000000000, 1.000000000000000000 ) ) ;
#20686 = CARTESIAN_POINT ( 'NONE',  ( 0.5640491644773603097, 9.257234168466334623, -2.305464659958512907 ) ) ;
#20687 = EDGE_CURVE ( 'NONE', #4862, #14011, #26650, .T. ) ;
#20688 = EDGE_LOOP ( 'NONE', ( #28342, #16708, #31578, #14797 ) ) ;
#20689 = CC_DESIGN_PERSON_AND_ORGANIZATION_ASSIGNMENT ( #14454, #24669, ( #3447 ) ) ;
#20690 = CARTESIAN_POINT ( 'NONE',  ( 5.885541838704149598, -6.185046950422357526, 5.674471607902420445 ) ) ;
#20691 = CARTESIAN_POINT ( 'NONE',  ( 41.44567272411835290, -7.615257740949710197, 4.522129901861162260 ) ) ;
#20692 = CARTESIAN_POINT ( 'NONE',  ( 47.94950013216721629, -7.827917879355752007, -2.184956529945580872 ) ) ;
#20693 = DIRECTION ( 'NONE',  ( -1.000000000000000000, -0.000000000000000000, -0.000000000000000000 ) ) ;
#20694 = CARTESIAN_POINT ( 'NONE',  ( 24.53773319407783760, -17.45675205880590752, 1.481708193828056963 ) ) ;
#20695 = DIRECTION ( 'NONE',  ( 0.000000000000000000, 0.000000000000000000, -1.000000000000000000 ) ) ;
#20696 = CARTESIAN_POINT ( 'NONE',  ( 24.04749999999999943, 2.594547506269380133, 0.7685399846772031918 ) ) ;
#20697 = CARTESIAN_POINT ( 'NONE',  ( 7.064423669210277978, -7.135485519863427051, -5.064320921489765759 ) ) ;
#20698 = ORIENTED_EDGE ( 'NONE', *, *, #4347, .F. ) ;
#20699 = CARTESIAN_POINT ( 'NONE',  ( -6.562550801365594211, -2.228590825266444586, -2.752080473201636401 ) ) ;
#20700 = ORIENTED_EDGE ( 'NONE', *, *, #25981, .F. ) ;
#20701 = ADVANCED_FACE ( 'NONE', ( #13770 ), #31703, .F. ) ;
#20702 = CARTESIAN_POINT ( 'NONE',  ( -4.454531657079158435, 1.545410377633947174, -2.846291840500173365 ) ) ;
#20703 = EDGE_CURVE ( 'NONE', #3275, #32538, #18986, .T. ) ;
#20704 = CARTESIAN_POINT ( 'NONE',  ( 107.6330232455594142, 18.97482909515709082, 5.056747795904239062 ) ) ;
#20705 = CARTESIAN_POINT ( 'NONE',  ( 1.624846380744160435, -1.458043416193428143, 1.758813134411630230 ) ) ;
#20706 = CARTESIAN_POINT ( 'NONE',  ( 25.61042644977005622, -17.59778802277103082, 1.500000000000000000 ) ) ;
#20707 = ORIENTED_EDGE ( 'NONE', *, *, #23525, .T. ) ;
#20708 = CARTESIAN_POINT ( 'NONE',  ( -1.082681991931091492, 0.000000000000000000, 4.629213727441584325 ) ) ;
#20709 = B_SPLINE_CURVE_WITH_KNOTS ( 'NONE', 3,
 ( #8876, #3403, #24265, #11219, #19084, #5730, #3559, #3224, #1030, #3883 ),
 .UNSPECIFIED., .F., .F.,
 ( 4, 2, 2, 2, 4 ),
 ( 3.032460776717885298E-07, 0.0005479053915603964179, 0.001095507537043121033, 0.001643109682525845322, 0.002190711828008569829 ),
 .UNSPECIFIED. ) ;
#20710 = ORIENTED_EDGE ( 'NONE', *, *, #31204, .F. ) ;
#20711 = CARTESIAN_POINT ( 'NONE',  ( 107.9618353151786181, 20.81780380167319677, -1.491740999229417941 ) ) ;
#20712 = APPROVAL_DATE_TIME ( #28067, #9842 ) ;
#20713 = CARTESIAN_POINT ( 'NONE',  ( 54.97358454004179151, -6.375051295539742924, 4.150065907150774613 ) ) ;
#20714 = FACE_OUTER_BOUND ( 'NONE', #22827, .T. ) ;
#20716 = DIRECTION ( 'NONE',  ( 0.000000000000000000, 0.000000000000000000, 1.000000000000000000 ) ) ;
#20715 = LINE ( 'NONE', #25901, #22514 ) ;
#20717 = ORIENTED_EDGE ( 'NONE', *, *, #2823, .F. ) ;
#20718 = CARTESIAN_POINT ( 'NONE',  ( -8.000050800000002127, -2.895451290119166021, -0.7990719894741236118 ) ) ;
#20719 = CARTESIAN_POINT ( 'NONE',  ( 3.063284526839887167, 0.4999240074894433228, 8.734705317681628500 ) ) ;
#20720 = CARTESIAN_POINT ( 'NONE',  ( 21.67250000136559507, 3.024605502323846729, -0.3178988483021056854 ) ) ;
#20721 = CARTESIAN_POINT ( 'NONE',  ( 7.077711312404307767E-17, 0.8254815157535250192, 4.681538312723519724 ) ) ;
#20723 = ORIENTED_EDGE ( 'NONE', *, *, #17824, .F. ) ;
#20722 = CARTESIAN_POINT ( 'NONE',  ( 108.3696618535068126, 20.23658298680886247, -1.378742097822665436 ) ) ;
#20724 = CARTESIAN_POINT ( 'NONE',  ( -6.312550801365593323, 3.675193018007247403, -1.088641768524161391 ) ) ;
#20725 = CARTESIAN_POINT ( 'NONE',  ( 0.000000000000000000, 0.000000000000000000, 0.000000000000000000 ) ) ;
#20726 = CARTESIAN_POINT ( 'NONE',  ( 29.22961111230330999, -6.951722887053946032, -3.390608046110267004 ) ) ;
#20727 = EDGE_LOOP ( 'NONE', ( #21868, #24898, #30867, #16820, #7025, #31734, #12088, #22191 ) ) ;
#20728 = ORIENTED_EDGE ( 'NONE', *, *, #20254, .T. ) ;
#20729 =( BOUNDED_SURFACE ( )  B_SPLINE_SURFACE ( 3, 2, ( 
 ( #1023, #9015, #23912 ),
 ( #713, #28626, #21589 ),
 ( #16240, #8711, #26453 ),
 ( #15899, #26108, #13374 ),
 ( #10903, #8384, #28769 ),
 ( #3552, #16045, #13711 ),
 ( #26277, #11206, #3393 ),
 ( #23764, #877, #6201 ),
 ( #27589, #9364, #4690 ),
 ( #14711, #30127, #29616 ),
 ( #17227, #19916, #26935 ),
 ( #11697, #4037, #9513 ),
 ( #7018, #17395, #16731 ),
 ( #7201, #25060, #27433 ),
 ( #4538, #9689, #19421 ),
 ( #12049, #24910, #14860 ),
 ( #12363, #22582, #2176 ),
 ( #6698, #16886, #21896 ) ),
 .UNSPECIFIED., .F., .F., .F. ) 
 B_SPLINE_SURFACE_WITH_KNOTS ( ( 4, 2, 2, 2, 2, 2, 2, 2, 4 ),
 ( 3, 3 ),
 ( 3.141592653589793116, 3.534291735288517255, 3.926990816987241395, 4.319689898685965090, 4.712388980384689674, 5.105088062083414258, 5.497787143782137953, 5.890486225480861648, 6.283185307179586232 ),
 ( 0.000000000000000000, 1.000000000000000000 ),
 .UNSPECIFIED. ) 
 GEOMETRIC_REPRESENTATION_ITEM ( )  RATIONAL_B_SPLINE_SURFACE ( (
 ( 1.000000000000000000, 0.5948227867513392608, 1.000000000000000000),
 ( 1.000000000000000000, 0.5947841457464595472, 1.000000000000000000),
 ( 1.000000000000000000, 0.5992555908982051260, 1.000000000000000000),
 ( 1.000000000000000000, 0.6156781713480670160, 1.000000000000000000),
 ( 1.000000000000000000, 0.6276164863437538877, 1.000000000000000000),
 ( 1.000000000000000000, 0.6558905360706541732, 1.000000000000000000),
 ( 1.000000000000000000, 0.6721825289739642439, 1.000000000000000000),
 ( 1.000000000000000000, 0.7057963334894752361, 1.000000000000000000),
 ( 1.000000000000000000, 0.7231030986475205369, 1.000000000000000000),
 ( 1.000000000000000000, 0.7560862040296049136, 1.000000000000000000),
 ( 1.000000000000000000, 0.7717639430041645099, 1.000000000000000000),
 ( 1.000000000000000000, 0.7996867613994225188, 1.000000000000000000),
 ( 1.000000000000000000, 0.8119378018739443759, 1.000000000000000000),
 ( 1.000000000000000000, 0.8319131657171122685, 1.000000000000000000),
 ( 1.000000000000000000, 0.8396427561410071405, 1.000000000000000000),
 ( 1.000000000000000000, 0.8500048284159551493, 1.000000000000000000),
 ( 1.000000000000000000, 0.8526458704374092479, 1.000000000000000000),
 ( 1.000000000000000000, 0.8526401643540935105, 1.000000000000000000) ) ) 
 REPRESENTATION_ITEM ( '' )  SURFACE ( )  );
#20730 = DIRECTION ( 'NONE',  ( 1.000000000000000000, -8.574039729943018344E-17, -0.000000000000000000 ) ) ;
#20731 = CYLINDRICAL_SURFACE ( 'NONE', #6382, 8.500000000000000000 ) ;
#20732 = ADVANCED_FACE ( 'NONE', ( #31220 ), #19079, .F. ) ;
#20733 = CARTESIAN_POINT ( 'NONE',  ( 22.11000000136559507, -2.892927487894331406, 1.570731468192932523 ) ) ;
#20734 = EDGE_CURVE ( 'NONE', #4370, #21301, #2687, .T. ) ;
#20735 = CARTESIAN_POINT ( 'NONE',  ( 0.5640491644773562019, 2.305464659958607943, 9.257234168466320412 ) ) ;
#20736 = CARTESIAN_POINT ( 'NONE',  ( 2.387277105415073208, -10.57576230868571976, 2.081082275505834023 ) ) ;
#20737 = ADVANCED_FACE ( 'NONE', ( #2083 ), #7098, .F. ) ;
#20738 = CARTESIAN_POINT ( 'NONE',  ( -47.55999999999999517, -10.96999999999998643, 9.000000000000000000 ) ) ;
#20739 = CARTESIAN_POINT ( 'NONE',  ( -23.35000000000000142, -10.96966150227469505, 4.000000000000000000 ) ) ;
#20740 = ORIENTED_EDGE ( 'NONE', *, *, #31868, .T. ) ;
#20741 = DIRECTION ( 'NONE',  ( -0.1908089953765494118, -0.000000000000000000, -0.9816271834476630875 ) ) ;
#20742 = DIRECTION ( 'NONE',  ( -0.9975973382524639943, -0.06927878976713693071, 0.000000000000000000 ) ) ;
#20743 = ORIENTED_EDGE ( 'NONE', *, *, #9397, .F. ) ;
#20744 = CARTESIAN_POINT ( 'NONE',  ( 0.000000000000000000, 0.000000000000000000, 0.000000000000000000 ) ) ;
#20745 = ORIENTED_EDGE ( 'NONE', *, *, #13212, .T. ) ;
#20746 = CARTESIAN_POINT ( 'NONE',  ( -4.962942409646514008, 3.284080845023683730E-15, 3.000000000000000000 ) ) ;
#20748 = VERTEX_POINT ( 'NONE', #19799 ) ;
#20747 = CARTESIAN_POINT ( 'NONE',  ( 69.02444692758074041, -5.195103839413598656, -4.215290682810015177 ) ) ;
#20749 = ORIENTED_EDGE ( 'NONE', *, *, #7450, .T. ) ;
#20750 = CARTESIAN_POINT ( 'NONE',  ( -3.370691070153704949, -1.614088942876946264, 1.500000000000000000 ) ) ;
#20751 = CARTESIAN_POINT ( 'NONE',  ( -6.012550801365594388, -1.828967928396026732, 3.368539882008728004 ) ) ;
#20752 = CARTESIAN_POINT ( 'NONE',  ( 7.249760686538667009, 6.139290821770257089, 5.151476664237498504 ) ) ;
#20753 = CARTESIAN_POINT ( 'NONE',  ( 23.58793147791972444, -8.793627369988310960, -1.915219082070897638 ) ) ;
#20755 = ORIENTED_EDGE ( 'NONE', *, *, #9153, .T. ) ;
#20754 = DIRECTION ( 'NONE',  ( 0.9816271834476637537, 0.000000000000000000, -0.1908089953765453872 ) ) ;
#20756 = CARTESIAN_POINT ( 'NONE',  ( 107.6439010983367410, -20.16588486397409596, 2.098868881559764255 ) ) ;
#20757 = CARTESIAN_POINT ( 'NONE',  ( 24.08142948293325247, 18.58944880476600048, 1.500000000000000000 ) ) ;
#20758 = CARTESIAN_POINT ( 'NONE',  ( -3.446172085536864049, -10.31568092537763270, 1.743523032603425671 ) ) ;
#20759 = CARTESIAN_POINT ( 'NONE',  ( 0.6791199890552934715, -7.071625480714427425, 5.814932665552373869 ) ) ;
#20760 = DIRECTION ( 'NONE',  ( 0.000000000000000000, 0.5735764363510441610, 0.8191520442889931308 ) ) ;
#20762 = ORIENTED_EDGE ( 'NONE', *, *, #14811, .T. ) ;
#20761 = DIRECTION ( 'NONE',  ( 1.000000000000000000, 0.000000000000000000, 0.000000000000000000 ) ) ;
#20763 = LINE ( 'NONE', #25448, #22105 ) ;
#20764 = EDGE_CURVE ( 'NONE', #20748, #21430, #11766, .T. ) ;
#20765 = B_SPLINE_CURVE_WITH_KNOTS ( 'NONE', 3,
 ( #16598, #31500, #26638, #1067, #3593, #6586, #23956, #23809, #31685, #8585 ),
 .UNSPECIFIED., .F., .F.,
 ( 4, 2, 2, 2, 4 ),
 ( 0.000000000000000000, 0.002028609684475585380, 0.003042914526713378070, 0.003550066947832274632, 0.004057219368951170760 ),
 .UNSPECIFIED. ) ;
#20766 = CARTESIAN_POINT ( 'NONE',  ( -1.959487840848934744E-16, -2.285372942704986254, 4.458382051008185520 ) ) ;
#20767 = CARTESIAN_POINT ( 'NONE',  ( 22.36000000136559152, 0.9349337715887185984, -3.156283516753368268 ) ) ;
#20768 = DIRECTION ( 'NONE',  ( -1.000000000000000000, 0.000000000000000000, -0.000000000000000000 ) ) ;
#20769 = DIRECTION ( 'NONE',  ( 0.9896144216807900573, 0.000000000000000000, 0.1437473352845041463 ) ) ;
#20770 = CARTESIAN_POINT ( 'NONE',  ( 101.8016823592330127, -4.042758964360499974, 3.993434276137187489 ) ) ;
#20771 = EDGE_LOOP ( 'NONE', ( #7090, #10099, #27164, #14550 ) ) ;
#20772 = FACE_OUTER_BOUND ( 'NONE', #15726, .T. ) ;
#20773 = DIRECTION ( 'NONE',  ( 1.000000000000000000, -2.473959037481237219E-13, 0.000000000000000000 ) ) ;
#20774 = ORIENTED_EDGE ( 'NONE', *, *, #23360, .F. ) ;
#20775 = DIRECTION ( 'NONE',  ( 0.9816271834476639757, 0.000000000000000000, -0.1908089953765449709 ) ) ;
#20776 = CARTESIAN_POINT ( 'NONE',  ( 10.57125986779756843, 4.971152295393309828, -0.6226916219171529931 ) ) ;
#20777 = DIRECTION ( 'NONE',  ( -0.000000000000000000, -0.000000000000000000, -1.000000000000000000 ) ) ;
#20779 = CARTESIAN_POINT ( 'NONE',  ( 107.4505400438408742, -17.36716520511782136, 4.540783781969483179 ) ) ;
#20778 = CARTESIAN_POINT ( 'NONE',  ( 41.45135008765516460, -9.497951668093163491, -0.07017451552783579571 ) ) ;
#20780 = ORIENTED_EDGE ( 'NONE', *, *, #28224, .T. ) ;
#20781 = CARTESIAN_POINT ( 'NONE',  ( -41.30241497097880909, -14.93473732866679882, 5.402788590779837641 ) ) ;
#20782 = ORIENTED_EDGE ( 'NONE', *, *, #5258, .T. ) ;
#20783 = DIRECTION ( 'NONE',  ( -1.000000000000000000, 0.000000000000000000, 0.000000000000000000 ) ) ;
#20785 = ORIENTED_EDGE ( 'NONE', *, *, #2575, .F. ) ;
#20784 = DIRECTION ( 'NONE',  ( 1.000000000000000000, -0.000000000000000000, -0.000000000000000000 ) ) ;
#20786 = ORIENTED_EDGE ( 'NONE', *, *, #31075, .T. ) ;
#20787 = CARTESIAN_POINT ( 'NONE',  ( 5.885541806331895387, -4.514241479885499508, -7.076443837534005077 ) ) ;
#20788 = CARTESIAN_POINT ( 'NONE',  ( 2.654002685506794634, 0.4696231843230830316, -1.499999999999999778 ) ) ;
#20790 = EDGE_LOOP ( 'NONE', ( #20056, #15195, #19437, #30662 ) ) ;
#20789 = CARTESIAN_POINT ( 'NONE',  ( 2.671540748214986660, 0.5000000000000006661, 1.500000000000000000 ) ) ;
#20791 = DIRECTION ( 'NONE',  ( 2.473959037481237219E-13, 1.000000000000000000, -0.000000000000000000 ) ) ;
#20792 = CARTESIAN_POINT ( 'NONE',  ( 3.679561191470742454, -12.16212054601122539, -1.758156634178598798 ) ) ;
#20793 = EDGE_CURVE ( 'NONE', #25934, #12596, #27497, .T. ) ;
#20794 = CARTESIAN_POINT ( 'NONE',  ( 18.72498703414868260, -6.251315747377667265, 3.393491514081778071 ) ) ;
#20795 = CARTESIAN_POINT ( 'NONE',  ( 8.007433738499996068, 15.00000000000000000, -5.396302277755718357 ) ) ;
#20796 = CARTESIAN_POINT ( 'NONE',  ( 3.499999999999999556, 6.100541242131516384, -3.528937025535512362 ) ) ;
#20797 = CARTESIAN_POINT ( 'NONE',  ( 0.000000000000000000, -2.861184399891040009, 6.440778198864103743 ) ) ;
#20798 = DIRECTION ( 'NONE',  ( 1.000000000000000000, 0.000000000000000000, 0.000000000000000000 ) ) ;
#20799 = DIRECTION ( 'NONE',  ( 0.000000000000000000, 8.673617379884035472E-16, -1.000000000000000000 ) ) ;
#20800 = DIRECTION ( 'NONE',  ( 1.000000000000000000, 0.000000000000000000, 0.000000000000000000 ) ) ;
#20801 = ADVANCED_FACE ( 'NONE', ( #9765 ), #30189, .T. ) ;
#20802 = EDGE_CURVE ( 'NONE', #30629, #8686, #26823, .T. ) ;
#20803 = CARTESIAN_POINT ( 'NONE',  ( 107.4500520109482409, -17.36019278854280401, -4.522129900387231949 ) ) ;
#20804 = DIRECTION ( 'NONE',  ( 0.000000000000000000, -0.3090169943749551673, 0.9510565162951511997 ) ) ;
#20805 = CIRCLE ( 'NONE', #26657, 8.500000000000000000 ) ;
#20806 = ORIENTED_EDGE ( 'NONE', *, *, #4705, .F. ) ;
#20807 = CARTESIAN_POINT ( 'NONE',  ( 34.99999999999999289, 0.5000000000000000000, 2.482234843104954791 ) ) ;
#20808 = ADVANCED_FACE ( 'NONE', ( #1430 ), #32195, .F. ) ;
#20809 = DIRECTION ( 'NONE',  ( 0.000000000000000000, 0.000000000000000000, 1.000000000000000000 ) ) ;
#20810 = ORIENTED_EDGE ( 'NONE', *, *, #3322, .F. ) ;
#20811 = DIRECTION ( 'NONE',  ( 0.4999999999999977796, 0.8660254037844398178, 0.000000000000000000 ) ) ;
#20812 = VERTEX_POINT ( 'NONE', #1762 ) ;
#20813 = FACE_OUTER_BOUND ( 'NONE', #1841, .T. ) ;
#20814 = ADVANCED_FACE ( 'NONE', ( #24461 ), #1578, .T. ) ;
#20815 = AXIS2_PLACEMENT_3D ( 'NONE', #2365, #10021, #30277 ) ;
#20816 = VECTOR ( 'NONE', #17048, 1000.000000000000227 ) ;
#20817 = ORIENTED_EDGE ( 'NONE', *, *, #32827, .F. ) ;
#20818 = CARTESIAN_POINT ( 'NONE',  ( -38.14293509397970183, 21.94000000000000128, 1.050000000000000044 ) ) ;
#20819 = ITEM_DEFINED_TRANSFORMATION ( 'NONE', 'NONE', #32754,  #2865 ) ;
#20821 = ORIENTED_EDGE ( 'NONE', *, *, #13035, .F. ) ;
#20820 = CARTESIAN_POINT ( 'NONE',  ( 0.7632845268398871230, 5.538577986808899567, 6.772677083992407532 ) ) ;
#20822 = EDGE_LOOP ( 'NONE', ( #15, #22176, #585, #16754 ) ) ;
#20823 = CARTESIAN_POINT ( 'NONE',  ( 12.44989959798868817, 18.00000000000000355, 13.00000000000004441 ) ) ;
#20824 = VERTEX_POINT ( 'NONE', #27146 ) ;
#20825 = AXIS2_PLACEMENT_3D ( 'NONE', #9582, #20301, #10265 ) ;
#20826 = CARTESIAN_POINT ( 'NONE',  ( 56.97280603064898941, -277.2763395528616002, -4.612695725900422872 ) ) ;
#20828 = ORIENTED_EDGE ( 'NONE', *, *, #22697, .T. ) ;
#20827 = CARTESIAN_POINT ( 'NONE',  ( 0.3076689118644526655, -9.439351442248995028, -4.089891983583746615 ) ) ;
#20829 = CARTESIAN_POINT ( 'NONE',  ( 25.10961529206432274, 18.61629793905443364, 1.050000000000000044 ) ) ;
#20830 = LINE ( 'NONE', #25676, #28261 ) ;
#20831 = CARTESIAN_POINT ( 'NONE',  ( 17.41559371906258136, 18.02474698348859405, 1.500000000000000000 ) ) ;
#20832 = LINE ( 'NONE', #21012, #8166 ) ;
#20833 = ORIENTED_EDGE ( 'NONE', *, *, #10592, .T. ) ;
#20834 = AXIS2_PLACEMENT_3D ( 'NONE', #445, #25868, #13141 ) ;
#20835 = CARTESIAN_POINT ( 'NONE',  ( -4.050050800000001061, -1.549418761218565255, 2.853674364686380471 ) ) ;
#20836 = CARTESIAN_POINT ( 'NONE',  ( -0.3880080537174158128, -2.647099810594272462, -4.522129901861164925 ) ) ;
#20837 = DIRECTION ( 'NONE',  ( 0.000000000000000000, 0.000000000000000000, -1.000000000000000000 ) ) ;
#20838 = CARTESIAN_POINT ( 'NONE',  ( 3.499999999999999556, -1.179494851233859887, -6.136676046192499179 ) ) ;
#20839 = EDGE_CURVE ( 'NONE', #31833, #17869, #25637, .T. ) ;
#20840 = EDGE_CURVE ( 'NONE', #12952, #2157, #9630, .T. ) ;
#20841 = VECTOR ( 'NONE', #20035, 1000.000000000000000 ) ;
#20842 = CARTESIAN_POINT ( 'NONE',  ( 24.41770876813069791, -17.42528320598814062, 1.442338022868773439 ) ) ;
#20843 = CARTESIAN_POINT ( 'NONE',  ( -7.050050802731187893, -1.887961173149512062, -2.331437884370912261 ) ) ;
#20844 = DIRECTION ( 'NONE',  ( -1.000000000000000000, -0.000000000000000000, -0.000000000000000000 ) ) ;
#20845 = CARTESIAN_POINT ( 'NONE',  ( 5.175170698068133568, 0.5000000000000000000, 5.403836275575642389 ) ) ;
#20846 = AXIS2_PLACEMENT_3D ( 'NONE', #17782, #20139, #22799 ) ;
#20847 = CARTESIAN_POINT ( 'NONE',  ( -3.112550801365593145, 3.675193018007247403, -1.088641768524161391 ) ) ;
#20848 = ORIENTED_EDGE ( 'NONE', *, *, #19701, .F. ) ;
#20849 = CARTESIAN_POINT ( 'NONE',  ( -4.854531657079157903, -1.545410377633946286, 2.846291840500174697 ) ) ;
#20850 = CIRCLE ( 'NONE', #19770, 6.000000000000000000 ) ;
#20851 = CARTESIAN_POINT ( 'NONE',  ( 12.27700767694853390, 19.86581740147262209, -5.396302277755719246 ) ) ;
#20852 = CARTESIAN_POINT ( 'NONE',  ( -5.150050800000000706, 3.113457007523260156, -0.9222479816126439855 ) ) ;
#20853 = CARTESIAN_POINT ( 'NONE',  ( 16.87487612390540903, -15.54663979847974176, 1.500000000000000000 ) ) ;
#20854 = ORIENTED_EDGE ( 'NONE', *, *, #7087, .F. ) ;
#20855 = DIRECTION ( 'NONE',  ( 0.9896144216807899463, -0.000000000000000000, 0.1437473352845038410 ) ) ;
#20856 = EDGE_CURVE ( 'NONE', #14011, #19637, #5098, .T. ) ;
#20857 = ORIENTED_EDGE ( 'NONE', *, *, #10999, .T. ) ;
#20858 = CARTESIAN_POINT ( 'NONE',  ( 2.632061376486628301, -0.4999999999999986122, 1.500000000000000000 ) ) ;
#20859 = SHAPE_DEFINITION_REPRESENTATION ( #9468, #30799 ) ;
#20860 = CIRCLE ( 'NONE', #17646, 0.4999999999999996114 ) ;
#20861 = AXIS2_PLACEMENT_3D ( 'NONE', #14020, #29593, #1167 ) ;
#20862 = CARTESIAN_POINT ( 'NONE',  ( 18.76007193770565351, -5.859136940314201070, 4.023790192988138337 ) ) ;
#20863 = VECTOR ( 'NONE', #31447, 1000.000000000000000 ) ;
#20864 = CARTESIAN_POINT ( 'NONE',  ( 10.00000000000000000, 3.641590349731929077, 3.055657119358814011 ) ) ;
#20865 = AXIS2_PLACEMENT_3D ( 'NONE', #28924, #15740, #31608 ) ;
#20867 = FACE_OUTER_BOUND ( 'NONE', #3993, .T. ) ;
#20866 = CYLINDRICAL_SURFACE ( 'NONE', #18852, 5.010000000000000675 ) ;
#20868 = ORIENTED_EDGE ( 'NONE', *, *, #9373, .T. ) ;
#20869 = CARTESIAN_POINT ( 'NONE',  ( 18.76371685223992003, -5.818394111047758166, 4.091315477141354684 ) ) ;
#20870 = FACE_OUTER_BOUND ( 'NONE', #15905, .T. ) ;
#20871 = EDGE_CURVE ( 'NONE', #23049, #18045, #28324, .T. ) ;
#20872 = CARTESIAN_POINT ( 'NONE',  ( 21.23500000136559507, -3.156283516753370044, -0.9349337715887220401 ) ) ;
#20874 = ORIENTED_EDGE ( 'NONE', *, *, #23022, .F. ) ;
#20873 = CARTESIAN_POINT ( 'NONE',  ( 23.75111450864416440, -1.283275288181523244E-15, -2.499999999999998668 ) ) ;
#20875 = CARTESIAN_POINT ( 'NONE',  ( -7.362550801365593145, -2.228590825266444586, -2.752080473201636401 ) ) ;
#20876 = B_SPLINE_CURVE_WITH_KNOTS ( 'NONE', 3,
 ( #20635, #2938, #30841, #8255, #3084, #400, #12744, #27990 ),
 .UNSPECIFIED., .F., .F.,
 ( 4, 2, 2, 4 ),
 ( 2.024520226828864513E-07, 0.001261135997420233463, 0.001891602770119006583, 0.002522069542817780355 ),
 .UNSPECIFIED. ) ;
#20877 = DIRECTION ( 'NONE',  ( -0.000000000000000000, 0.9961946980917458783, -0.08715574274765452989 ) ) ;
#20878 = CARTESIAN_POINT ( 'NONE',  ( 102.4756904796925596, -4.748902435557111446, -2.787782622584134451 ) ) ;
#20879 = VERTEX_POINT ( 'NONE', #18108 ) ;
#20880 = EDGE_LOOP ( 'NONE', ( #16868, #8519, #18686, #15413, #3627, #18841, #15358, #6255 ) ) ;
#20881 = DIRECTION ( 'NONE',  ( 1.000000000000000000, -0.000000000000000000, 0.000000000000000000 ) ) ;
#20882 = CARTESIAN_POINT ( 'NONE',  ( 4.749760686538667009, -6.139290821770219786, -5.151476664237539360 ) ) ;
#20883 = CIRCLE ( 'NONE', #14987, 5.587650971692158741 ) ;
#20884 = DIRECTION ( 'NONE',  ( 8.574039729943018344E-17, 1.000000000000000000, 0.000000000000000000 ) ) ;
#20885 = CIRCLE ( 'NONE', #13388, 2.999999999999999112 ) ;
#20886 = CIRCLE ( 'NONE', #29957, 0.4999999999999996114 ) ;
#20887 = CARTESIAN_POINT ( 'NONE',  ( 17.37538333147394098, -21.16291065652744763, -1.500000000000001554 ) ) ;
#20888 = DIRECTION ( 'NONE',  ( 0.000000000000000000, 1.000000000000000000, 0.000000000000000000 ) ) ;
#20889 = VECTOR ( 'NONE', #30375, 1000.000000000000000 ) ;
#20890 = DIRECTION ( 'NONE',  ( 0.000000000000000000, -0.8090169943749403458, -0.5877852522924831291 ) ) ;
#20891 = CARTESIAN_POINT ( 'NONE',  ( 0.7632845268398871230, 0.000000000000000000, 0.000000000000000000 ) ) ;
#20892 = VERTEX_POINT ( 'NONE', #25324 ) ;
#20893 = LINE ( 'NONE', #23885, #18823 ) ;
#20894 = AXIS2_PLACEMENT_3D ( 'NONE', #8439, #6256, #781 ) ;
#20895 = ORIENTED_EDGE ( 'NONE', *, *, #3904, .F. ) ;
#20896 = MECHANICAL_CONTEXT ( 'NONE', #25714, 'mechanical' ) ;
#20897 = LINE ( 'NONE', #10194, #10720 ) ;
#20898 = VERTEX_POINT ( 'NONE', #262 ) ;
#20899 = FACE_OUTER_BOUND ( 'NONE', #28875, .T. ) ;
#20900 = ORIENTED_EDGE ( 'NONE', *, *, #23365, .F. ) ;
#20901 = CARTESIAN_POINT ( 'NONE',  ( -20.49373157874864759, 4.792442962972690346, 2.124178786190599855 ) ) ;
#20903 = ORIENTED_EDGE ( 'NONE', *, *, #33046, .T. ) ;
#20902 = CARTESIAN_POINT ( 'NONE',  ( 28.69165144960210867, -5.691079856418894245, -4.093303788746957217 ) ) ;
#20904 = AXIS2_PLACEMENT_3D ( 'NONE', #6277, #14134, #31384 ) ;
#20905 = ORIENTED_EDGE ( 'NONE', *, *, #947, .F. ) ;
#20906 = EDGE_CURVE ( 'NONE', #28296, #13484, #11237, .T. ) ;
#20907 = DIRECTION ( 'NONE',  ( 0.000000000000000000, 0.000000000000000000, 1.000000000000000000 ) ) ;
#20908 = CARTESIAN_POINT ( 'NONE',  ( -5.812550801365592434, -3.368539882008727115, -1.828967928396027842 ) ) ;
#20909 = ADVANCED_FACE ( 'NONE', ( #4752 ), #3602, .T. ) ;
#20910 = VECTOR ( 'NONE', #9136, 1000.000000000000000 ) ;
#20911 = CARTESIAN_POINT ( 'NONE',  ( 11.67286638378806352, -13.57952815233281640, 1.499999999999999778 ) ) ;
#20912 = CONICAL_SURFACE ( 'NONE', #25173, 297.9081695149525899, 0.4915790642873721361 ) ;
#20913 = CARTESIAN_POINT ( 'NONE',  ( 7.077711312404307767E-17, 0.8254815157535250192, 4.681538312723519724 ) ) ;
#20914 =( BOUNDED_CURVE ( )  B_SPLINE_CURVE ( 2, ( #29306, #16597, #24300, #11589, #4584 ),
 .UNSPECIFIED., .F., .F. ) 
 B_SPLINE_CURVE_WITH_KNOTS ( ( 3, 2, 3 ),
 ( 0.05000000059124252300, 0.07499999999999999722, 0.09661161918950035565 ),
 .UNSPECIFIED. ) 
 CURVE ( )  GEOMETRIC_REPRESENTATION_ITEM ( )  RATIONAL_B_SPLINE_CURVE ( ( 1.000000000000000000, 0.9238795325112867385, 1.000000000000000000, 0.9341965377642874602, 0.9821626249036858880 ) ) 
 REPRESENTATION_ITEM ( '' )  );
#20916 = ORIENTED_EDGE ( 'NONE', *, *, #32794, .F. ) ;
#20915 = CARTESIAN_POINT ( 'NONE',  ( 0.000000000000000000, -7.673322273190700926, -3.656518192455154637 ) ) ;
#20917 = FACE_OUTER_BOUND ( 'NONE', #16909, .T. ) ;
#20918 = CARTESIAN_POINT ( 'NONE',  ( 2.274274201625327230, 0.000000000000000000, 0.000000000000000000 ) ) ;
#20919 = EDGE_CURVE ( 'NONE', #1029, #6686, #16851, .T. ) ;
#20920 = CARTESIAN_POINT ( 'NONE',  ( -3.686313051336277180, -9.650521517436112973, 1.743567022824936696 ) ) ;
#20921 = CARTESIAN_POINT ( 'NONE',  ( 0.3045633657615048895, -7.698316278340158192, 6.808202580038414276 ) ) ;
#20922 = CARTESIAN_POINT ( 'NONE',  ( -2.506063600758156262, 0.4999999999999998890, -1.500000000000000000 ) ) ;
#20924 = ORIENTED_EDGE ( 'NONE', *, *, #2182, .T. ) ;
#20923 = CARTESIAN_POINT ( 'NONE',  ( 23.29109779593935414, -17.41442569313434063, 1.664431119656365254 ) ) ;
#20925 = CARTESIAN_POINT ( 'NONE',  ( 2.274274201625327230, 0.000000000000000000, 0.000000000000000000 ) ) ;
#20926 = CIRCLE ( 'NONE', #17713, 299.3348442831094189 ) ;
#20927 = CIRCLE ( 'NONE', #18247, 2.999999999999999112 ) ;
#20928 = DIRECTION ( 'NONE',  ( -1.000000000000000000, 0.000000000000000000, -0.000000000000000000 ) ) ;
#20929 = CARTESIAN_POINT ( 'NONE',  ( 24.67250000273118360, -2.378061970571983430, 1.291182301015471712 ) ) ;
#20930 = CARTESIAN_POINT ( 'NONE',  ( -8.000050800000000351, 0.05271045196100602320, -2.999989457909464363 ) ) ;
#20931 = CARTESIAN_POINT ( 'NONE',  ( 2.592584690696363214, -4.120115534657249334, -9.468199582994131447 ) ) ;
#20932 = CARTESIAN_POINT ( 'NONE',  ( 9.282537329959909655, 0.2172754300399125094, 1.041239158277188048 ) ) ;
#20933 = CARTESIAN_POINT ( 'NONE',  ( 107.9852701348502819, -17.85725572279256212, 4.475774678959534292 ) ) ;
#20934 = AXIS2_PLACEMENT_3D ( 'NONE', #30027, #14941, #32215 ) ;
#20935 = CARTESIAN_POINT ( 'NONE',  ( -7.906300802048391141, 0.3418742348694470690, -3.252716068056403564 ) ) ;
#20936 = ORIENTED_EDGE ( 'NONE', *, *, #2080, .F. ) ;
#20937 = AXIS2_PLACEMENT_3D ( 'NONE', #14671, #4147, #1638 ) ;
#20938 = AXIS2_PLACEMENT_3D ( 'NONE', #21251, #32415, #29733 ) ;
#20939 = CIRCLE ( 'NONE', #1704, 300.9381170038701612 ) ;
#20940 = CARTESIAN_POINT ( 'NONE',  ( 2.942065251340673093, -8.983930386558810710, 2.300561732648069402 ) ) ;
#20941 = CARTESIAN_POINT ( 'NONE',  ( -3.043440560540900286, -0.3795130046622989806, -1.490258760090589218 ) ) ;
#20942 = CARTESIAN_POINT ( 'NONE',  ( -29.24402871571405882, -25.43932300454937945, 11.00000000000000000 ) ) ;
#20945 = CARTESIAN_POINT ( 'NONE',  ( 107.4510466397278350, -17.37451394313761099, 4.559260914617079052 ) ) ;
#20944 = DIRECTION ( 'NONE',  ( 0.000000000000000000, -0.000000000000000000, -1.000000000000000000 ) ) ;
#20943 = CIRCLE ( 'NONE', #8640, 10.99999999999999822 ) ;
#20946 = ORIENTED_EDGE ( 'NONE', *, *, #24672, .T. ) ;
#20947 = AXIS2_PLACEMENT_3D ( 'NONE', #12248, #21959, #27489 ) ;
#20948 = CARTESIAN_POINT ( 'NONE',  ( 15.84732276226623604, 14.44600775457921493, 1.050000000000000044 ) ) ;
#20949 = VERTEX_POINT ( 'NONE', #30697 ) ;
#20950 = CARTESIAN_POINT ( 'NONE',  ( 7.249760686538667009, 6.226446564517917892, 6.147671362329242051 ) ) ;
#20952 = VERTEX_POINT ( 'NONE', #7770 ) ;
#20951 = DIRECTION ( 'NONE',  ( 0.000000000000000000, 0.9510565162951544194, -0.3090169943749446202 ) ) ;
#20953 = VERTEX_POINT ( 'NONE', #20789 ) ;
#20954 = EDGE_CURVE ( 'NONE', #32424, #11793, #10155, .T. ) ;
#20955 = CARTESIAN_POINT ( 'NONE',  ( 18.86054332783663767, -4.736068442360261699, 3.993434336035624366 ) ) ;
#20956 = EDGE_CURVE ( 'NONE', #1130, #24612, #4925, .T. ) ;
#20957 = EDGE_CURVE ( 'NONE', #22238, #32480, #2106, .T. ) ;
#20958 = DIRECTION ( 'NONE',  ( 0.000000000000000000, 0.000000000000000000, -1.000000000000000000 ) ) ;
#20960 = ORIENTED_EDGE ( 'NONE', *, *, #24287, .T. ) ;
#20959 = CARTESIAN_POINT ( 'NONE',  ( 5.612718761614565288, -3.934162523501283815, 7.212912035758797913 ) ) ;
#20961 = AXIS2_PLACEMENT_3D ( 'NONE', #4643, #27383, #4496 ) ;
#20962 = ORIENTED_EDGE ( 'NONE', *, *, #21383, .T. ) ;
#20963 = CARTESIAN_POINT ( 'NONE',  ( 0.09007350345950326798, -14.90606730690115000, -1.745535732425882225 ) ) ;
#20964 = AXIS2_PLACEMENT_3D ( 'NONE', #19280, #23952, #1063 ) ;
#20965 = LINE ( 'NONE', #17964, #11809 ) ;
#20966 = TOROIDAL_SURFACE ( 'NONE', #22035, 5.500000000000001776, 0.5000000000000000000 ) ;
#20967 = CARTESIAN_POINT ( 'NONE',  ( 2.921917104085894298E-16, 3.407865132560230492, -3.672404558090004212 ) ) ;
#20968 = CARTESIAN_POINT ( 'NONE',  ( -2.484167557306937280, -0.3164610288023908535, 3.010925563584172515 ) ) ;
#20969 = CARTESIAN_POINT ( 'NONE',  ( 2.795120570939532367, 3.714272345039596246, 9.022485053488384921 ) ) ;
#20970 = AXIS2_PLACEMENT_3D ( 'NONE', #30199, #22671, #25649 ) ;
#20971 = VECTOR ( 'NONE', #26798, 1000.000000000000000 ) ;
#20972 = CARTESIAN_POINT ( 'NONE',  ( -15.12340757463330654, -27.93932300454937590, -1.000000000000000000 ) ) ;
#20973 = CARTESIAN_POINT ( 'NONE',  ( 2.318314390550209048, -10.58246510144062924, 1.499999999999999778 ) ) ;
#20974 = LINE ( 'NONE', #7928, #7716 ) ;
#20975 = AXIS2_PLACEMENT_3D ( 'NONE', #22547, #14831, #15335 ) ;
#20976 = LINE ( 'NONE', #28805, #16088 ) ;
#20977 = DIRECTION ( 'NONE',  ( -1.000000000000000000, 0.000000000000000000, 0.000000000000000000 ) ) ;
#20978 = ORIENTED_EDGE ( 'NONE', *, *, #1543, .T. ) ;
#20979 = CARTESIAN_POINT ( 'NONE',  ( 2.274274201625327230, 0.000000000000000000, 0.000000000000000000 ) ) ;
#20980 = CARTESIAN_POINT ( 'NONE',  ( 41.43369393131070666, -3.642920876109168926, 2.713652344655542503 ) ) ;
#20981 = CARTESIAN_POINT ( 'NONE',  ( 0.000000000000000000, 0.000000000000000000, 0.000000000000000000 ) ) ;
#20982 = ORIENTED_EDGE ( 'NONE', *, *, #31592, .F. ) ;
#20983 = CARTESIAN_POINT ( 'NONE',  ( 24.67250000136559507, 3.024605502323846729, -0.3178988483021056854 ) ) ;
#20984 = CIRCLE ( 'NONE', #5530, 2.999999999999999556 ) ;
#20985 = EDGE_CURVE ( 'NONE', #7402, #12740, #582, .T. ) ;
#20986 = VECTOR ( 'NONE', #31801, 999.9999999999998863 ) ;
#20987 = DIRECTION ( 'NONE',  ( -1.000000000000000000, -0.000000000000000000, 0.000000000000000000 ) ) ;
#20988 = CARTESIAN_POINT ( 'NONE',  ( 1.624999999999999778, -10.90201369670497833, -1.464956435139658231 ) ) ;
#20990 = VERTEX_POINT ( 'NONE', #30994 ) ;
#20989 = VECTOR ( 'NONE', #3868, 1000.000000000000114 ) ;
#20991 = CARTESIAN_POINT ( 'NONE',  ( 3.499999999999999556, 0.000000000000000000, 0.000000000000000000 ) ) ;
#20992 = VECTOR ( 'NONE', #8533, 1000.000000000000227 ) ;
#20993 = AXIS2_PLACEMENT_3D ( 'NONE', #27926, #7705, #28240 ) ;
#20994 = ADVANCED_FACE ( 'NONE', ( #28648 ), #5743, .T. ) ;
#20995 = ORIENTED_EDGE ( 'NONE', *, *, #17035, .F. ) ;
#20996 = CARTESIAN_POINT ( 'NONE',  ( 107.6300413742128228, -19.95926608421483195, 0.000000000000000000 ) ) ;
#20997 = DATE_AND_TIME ( #28336, #3475 ) ;
#20999 = VERTEX_POINT ( 'NONE', #18947 ) ;
#20998 = CARTESIAN_POINT ( 'NONE',  ( 18.62789956201168096, -21.71817389964364153, -0.9788672205760856615 ) ) ;
#21000 = ORIENTED_EDGE ( 'NONE', *, *, #8888, .F. ) ;
#21001 = CARTESIAN_POINT ( 'NONE',  ( 24.79750000136559507, 0.3178988483021036315, 3.024605502323848949 ) ) ;
#21002 = AXIS2_PLACEMENT_3D ( 'NONE', #8808, #26534, #4123 ) ;
#21003 = EDGE_CURVE ( 'NONE', #18598, #17832, #26475, .T. ) ;
#21004 = ORIENTED_EDGE ( 'NONE', *, *, #30430, .T. ) ;
#21005 = CARTESIAN_POINT ( 'NONE',  ( -1.757992424077718940, -0.3150232093026757996, 2.997245624844496081 ) ) ;
#21007 = ORIENTED_EDGE ( 'NONE', *, *, #16539, .F. ) ;
#21006 = CARTESIAN_POINT ( 'NONE',  ( 41.34400607036777586, -3.938209558064118987, -0.8105618912876280113 ) ) ;
#21008 = CARTESIAN_POINT ( 'NONE',  ( 15.48186204063833138, 10.33650625749590546, 1.049999999999999600 ) ) ;
#21009 = DIRECTION ( 'NONE',  ( 0.000000000000000000, 0.000000000000000000, 1.000000000000000000 ) ) ;
#21010 = EDGE_CURVE ( 'NONE', #4970, #21159, #24843, .T. ) ;
#21011 = CARTESIAN_POINT ( 'NONE',  ( -61.56966150227469114, -10.96966150227468972, 1.500000000000000000 ) ) ;
#21012 = CARTESIAN_POINT ( 'NONE',  ( -4.075891499408641642E-16, -4.753758587302147731, 0.000000000000000000 ) ) ;
#21013 = ORIENTED_EDGE ( 'NONE', *, *, #10178, .T. ) ;
#21014 = CIRCLE ( 'NONE', #1803, 2.099999999999997868 ) ;
#21015 = AXIS2_PLACEMENT_3D ( 'NONE', #26386, #21035, #11136 ) ;
#21016 = DIRECTION ( 'NONE',  ( 1.000000000000000000, 0.000000000000000000, 0.000000000000000000 ) ) ;
#21017 = CARTESIAN_POINT ( 'NONE',  ( 3.499999999999999556, 7.008469740302810891, -0.7425307242147067832 ) ) ;
#21018 = EDGE_CURVE ( 'NONE', #9606, #12581, #22831, .T. ) ;
#21019 = CARTESIAN_POINT ( 'NONE',  ( 85.11758351742656714, -6.522238754303181452, -1.873788413186571189 ) ) ;
#21020 = CARTESIAN_POINT ( 'NONE',  ( -6.956376981307135665, 0.1572233378491243172, -2.999999999999999556 ) ) ;
#21021 = AXIS2_PLACEMENT_3D ( 'NONE', #6893, #17085, #8761 ) ;
#21022 = AXIS2_PLACEMENT_3D ( 'NONE', #20739, #10863, #26075 ) ;
#21023 = CIRCLE ( 'NONE', #6592, 5.010000000000000675 ) ;
#21024 = B_SPLINE_CURVE_WITH_KNOTS ( 'NONE', 3,
 ( #29569, #19033, #16845, #14312, #24362, #9134, #3998, #6807 ),
 .UNSPECIFIED., .F., .F.,
 ( 4, 2, 2, 4 ),
 ( 5.099451029791657500E-07, 0.001229189590460676770, 0.001843529413139525413, 0.002457869235818374055 ),
 .UNSPECIFIED. ) ;
#21025 = CARTESIAN_POINT ( 'NONE',  ( -8.000050799999998574, -0.9398417724546661578, 2.990403141914843133 ) ) ;
#21026 = CYLINDRICAL_SURFACE ( 'NONE', #30013, 0.5000000000000000000 ) ;
#21027 = CARTESIAN_POINT ( 'NONE',  ( 22.92250000273118715, -1.291182301015472600, -2.378061970571982098 ) ) ;
#21028 = CYLINDRICAL_SURFACE ( 'NONE', #18259, 3.750000000000000444 ) ;
#21029 = LOCAL_TIME ( 16, 7, 10.00000000000000000, #853 ) ;
#21030 = CARTESIAN_POINT ( 'NONE',  ( -3.712550801365592790, 1.088641768524161613, 3.675193018007247403 ) ) ;
#21031 = ORIENTED_EDGE ( 'NONE', *, *, #32458, .F. ) ;
#21032 = CARTESIAN_POINT ( 'NONE',  ( -4.904531657079156837, -0.3127741368606806738, 2.975847129947406522 ) ) ;
#21033 = EDGE_CURVE ( 'NONE', #5334, #18559, #6074, .T. ) ;
#21034 = FACE_OUTER_BOUND ( 'NONE', #19554, .T. ) ;
#21035 = DIRECTION ( 'NONE',  ( 0.000000000000000000, -0.000000000000000000, -1.000000000000000000 ) ) ;
#21036 = CARTESIAN_POINT ( 'NONE',  ( 9.360049168480738757, -11.53021799169789752, 1.500000000000214939 ) ) ;
#21037 = ORIENTED_EDGE ( 'NONE', *, *, #15460, .F. ) ;
#21038 = CARTESIAN_POINT ( 'NONE',  ( 3.499999999999999556, -4.147285340411747789, -5.698247474649445365 ) ) ;
#21039 = CIRCLE ( 'NONE', #29578, 7.318435636271054534 ) ;
#21040 = VECTOR ( 'NONE', #15847, 1000.000000000000000 ) ;
#21041 = ORIENTED_EDGE ( 'NONE', *, *, #27391, .T. ) ;
#21042 = CARTESIAN_POINT ( 'NONE',  ( 0.9355032790606521154, -3.271333551678202056, 1.499999999999860778 ) ) ;
#21043 = PERSON_AND_ORGANIZATION_ROLE ( 'creator' ) ;
#21044 = EDGE_CURVE ( 'NONE', #24398, #3200, #420, .T. ) ;
#21045 = CARTESIAN_POINT ( 'NONE',  ( 18.76498559208903671, -5.804212145908565823, 4.093303788723032355 ) ) ;
#21046 = AXIS2_PLACEMENT_3D ( 'NONE', #5272, #2453, #15447 ) ;
#21047 = EDGE_CURVE ( 'NONE', #9004, #21250, #19261, .T. ) ;
#21048 = CARTESIAN_POINT ( 'NONE',  ( 2.482257818914018088, 0.000000000000000000, -1.712210361609936005 ) ) ;
#21049 = CARTESIAN_POINT ( 'NONE',  ( 7.249760686538667009, 8.437262856154195134, -2.318425219014145444 ) ) ;
#21050 = AXIS2_PLACEMENT_3D ( 'NONE', #3676, #3041, #3187 ) ;
#21051 = ORIENTED_EDGE ( 'NONE', *, *, #17322, .T. ) ;
#21052 = LOCAL_TIME ( 16, 7, 10.00000000000000000, #15840 ) ;
#21053 = EDGE_CURVE ( 'NONE', #5412, #11370, #32060, .T. ) ;
#21054 = DIRECTION ( 'NONE',  ( -1.000000000000000000, 0.000000000000000000, 0.000000000000000000 ) ) ;
#21055 = DIRECTION ( 'NONE',  ( -1.000000000000000000, 0.000000000000000000, 0.000000000000000000 ) ) ;
#21056 = CARTESIAN_POINT ( 'NONE',  ( 9.350000000000004974, -2.117582368135751233E-18, 1.049909311857671668 ) ) ;
#21057 = B_SPLINE_CURVE_WITH_KNOTS ( 'NONE', 3,
 ( #6465, #32562, #31904, #32254, #9632, #24507, #32409, #29567, #14815, #29880 ),
 .UNSPECIFIED., .F., .F.,
 ( 4, 2, 2, 2, 4 ),
 ( 1.968338519013029732E-07, 0.0005467926395225683033, 0.001093388445193234533, 0.001639984250863900980, 0.002186580056534567426 ),
 .UNSPECIFIED. ) ;
#21059 = ORIENTED_EDGE ( 'NONE', *, *, #31104, .T. ) ;
#21058 = CARTESIAN_POINT ( 'NONE',  ( 3.249999999999999556, -9.241976615262146311, -1.699438267350472209 ) ) ;
#21060 = CARTESIAN_POINT ( 'NONE',  ( -2.712550801365593234, -3.675193018007246071, 1.088641768524163167 ) ) ;
#21061 = CARTESIAN_POINT ( 'NONE',  ( 0.9801757370192284435, 20.00000000000000000, -6.747923662139671208 ) ) ;
#21062 = CARTESIAN_POINT ( 'NONE',  ( 54.98781319022972980, -6.881869368919742769, -3.390608480956866178 ) ) ;
#21063 = ORIENTED_EDGE ( 'NONE', *, *, #16663, .F. ) ;
#21064 = VERTEX_POINT ( 'NONE', #5888 ) ;
#21065 = EDGE_CURVE ( 'NONE', #4203, #29021, #3421, .T. ) ;
#21066 = VECTOR ( 'NONE', #19143, 1000.000000000000000 ) ;
#21067 = CARTESIAN_POINT ( 'NONE',  ( 56.97280603064898941, -277.2763395528616002, 4.621439243524390506 ) ) ;
#21068 = CARTESIAN_POINT ( 'NONE',  ( 7.249760686538667009, 0.7071067811865129338, 8.721381771256208282 ) ) ;
#21069 = CARTESIAN_POINT ( 'NONE',  ( 69.18703749905368738, -4.112663945019823686, 4.522129901861162260 ) ) ;
#21070 = CARTESIAN_POINT ( 'NONE',  ( 0.000000000000000000, 8.357095590591338663, 1.552080310331533486 ) ) ;
#21071 = PLANE ( 'NONE',  #9232 ) ;
#21072 = LOCAL_TIME ( 16, 7, 10.00000000000000000, #30213 ) ;
#21073 = DIRECTION ( 'NONE',  ( 1.000000000000000000, 0.000000000000000000, 0.000000000000000000 ) ) ;
#21074 = CARTESIAN_POINT ( 'NONE',  ( 85.13967574987862008, -6.881122605237359302, 0.8105612905563517323 ) ) ;
#21075 = VERTEX_POINT ( 'NONE', #8557 ) ;
#21076 = DIRECTION ( 'NONE',  ( 0.000000000000000000, 0.000000000000000000, -1.000000000000000000 ) ) ;
#21077 = EDGE_CURVE ( 'NONE', #26082, #18185, #18769, .T. ) ;
#21078 = EDGE_LOOP ( 'NONE', ( #31725, #6825, #29317, #14384 ) ) ;
#21079 = CALENDAR_DATE ( 2026, 6, 10 ) ;
#21080 = ADVANCED_FACE ( 'NONE', ( #26960 ), #31972, .F. ) ;
#21081 = CARTESIAN_POINT ( 'NONE',  ( 23.84310522038115465, -4.329614468541457484, 4.522129901861162260 ) ) ;
#21082 = ORIENTED_EDGE ( 'NONE', *, *, #5362, .T. ) ;
#21083 = CIRCLE ( 'NONE', #6137, 2.524999999999999911 ) ;
#21084 = CARTESIAN_POINT ( 'NONE',  ( 24.35832023931602208, -17.33818253687209676, 1.317734466820223549 ) ) ;
#21085 = EDGE_LOOP ( 'NONE', ( #21693, #32966, #13735, #1416 ) ) ;
#21086 = DIRECTION ( 'NONE',  ( 0.000000000000000000, 0.000000000000000000, -1.000000000000000000 ) ) ;
#21088 = EDGE_LOOP ( 'NONE', ( #30169, #10122, #21786, #2867 ) ) ;
#21087 = CARTESIAN_POINT ( 'NONE',  ( 84.97632234719172573, -4.234187385253560088, -4.185347070103271783 ) ) ;
#21089 = ORIENTED_EDGE ( 'NONE', *, *, #22893, .F. ) ;
#21090 = CARTESIAN_POINT ( 'NONE',  ( 3.541509388326463004, -13.88765124358303993, -4.522129901861164925 ) ) ;
#21091 = CARTESIAN_POINT ( 'NONE',  ( -3.112550801365593145, 3.675193018007246959, -1.088641768524161391 ) ) ;
#21092 = CARTESIAN_POINT ( 'NONE',  ( 9.613697478362638549, -12.36077863760316475, 1.500000000000000222 ) ) ;
#21093 = CARTESIAN_POINT ( 'NONE',  ( 2.303429269646776412, -1.057870905165122055, -1.499999999999999112 ) ) ;
#21095 = ORIENTED_EDGE ( 'NONE', *, *, #11244, .T. ) ;
#21094 = CARTESIAN_POINT ( 'NONE',  ( 6.880159540721329847, 7.943102264535301771, -3.624895993596787491 ) ) ;
#21096 = CARTESIAN_POINT ( 'NONE',  ( -6.187550801365593323, -0.3701630799359326152, 3.521866450007987037 ) ) ;
#21097 = CARTESIAN_POINT ( 'NONE',  ( 17.59176001116349752, 13.74650376811828423, 1.500000000000000222 ) ) ;
#21098 = DIRECTION ( 'NONE',  ( 1.000000000000000000, 0.000000000000000000, -4.336808689942013792E-15 ) ) ;
#21099 = CARTESIAN_POINT ( 'NONE',  ( -33.81874022276151948, 19.50000000000000000, -1.818740222761502601 ) ) ;
#21100 = LINE ( 'NONE', #522, #25105 ) ;
#21102 = ORIENTED_EDGE ( 'NONE', *, *, #30826, .T. ) ;
#21101 = CARTESIAN_POINT ( 'NONE',  ( -23.54713438637982748, 8.275374457817619600, 8.600000000000004974 ) ) ;
#21103 = CARTESIAN_POINT ( 'NONE',  ( 3.063284526839887167, 0.000000000000000000, 0.000000000000000000 ) ) ;
#21104 = EDGE_CURVE ( 'NONE', #23564, #18851, #8560, .T. ) ;
#21105 = PRODUCT_DEFINITION ( 'UNKNOWN', '', #5017, #457 ) ;
#21106 = CARTESIAN_POINT ( 'NONE',  ( 9.101556641444268791, 4.770368330595423290E-16, 3.895301350492843540 ) ) ;
#21107 = CARTESIAN_POINT ( 'NONE',  ( 24.17250000273118360, 2.378061970571979433, -1.291182301015470824 ) ) ;
#21108 = DIRECTION ( 'NONE',  ( -7.472768010110897478E-18, -0.08715574274765533480, -0.9961946980917457672 ) ) ;
#21109 = CARTESIAN_POINT ( 'NONE',  ( 78.98737618897432355, 23.37029618663415320, 5.412820279296879811 ) ) ;
#21110 = LINE ( 'NONE', #12896, #32747 ) ;
#21111 = DIRECTION ( 'NONE',  ( 0.000000000000000000, 0.000000000000000000, 1.000000000000000000 ) ) ;
#21112 = CARTESIAN_POINT ( 'NONE',  ( -16.20597128428593336, -10.96966150227469328, -11.50000000000000000 ) ) ;
#21113 = ORIENTED_EDGE ( 'NONE', *, *, #14248, .F. ) ;
#21114 = EDGE_CURVE ( 'NONE', #16163, #8185, #13889, .T. ) ;
#21115 = B_SPLINE_CURVE_WITH_KNOTS ( 'NONE', 3,
 ( #4955, #2608, #12131, #30363, #12773, #22982, #25348, #30721 ),
 .UNSPECIFIED., .F., .F.,
 ( 4, 2, 2, 4 ),
 ( 2.737843117452289853E-07, 0.001261207499628671418, 0.001891674357287133779, 0.002522141214945596357 ),
 .UNSPECIFIED. ) ;
#21116 = CARTESIAN_POINT ( 'NONE',  ( 0.000000000000000000, 0.000000000000000000, 0.000000000000000000 ) ) ;
#21117 = EDGE_CURVE ( 'NONE', #5623, #25934, #27632, .T. ) ;
#21118 = CARTESIAN_POINT ( 'NONE',  ( -3.167307446159718598, 1.905824131322175763E-18, -1.051955142024793677 ) ) ;
#21119 = DIRECTION ( 'NONE',  ( 8.574039729943018344E-17, 1.000000000000000000, 0.000000000000000000 ) ) ;
#21121 = CARTESIAN_POINT ( 'NONE',  ( 107.9815407526517390, -17.80355354688649072, 4.374676372033779792 ) ) ;
#21120 = LINE ( 'NONE', #29272, #30557 ) ;
#21122 = VERTEX_POINT ( 'NONE', #29642 ) ;
#21123 = CARTESIAN_POINT ( 'NONE',  ( 0.000000000000000000, 6.807171995660674213, -6.478011392632816445 ) ) ;
#21124 = ORIENTED_EDGE ( 'NONE', *, *, #32526, .T. ) ;
#21125 = PLANE ( 'NONE',  #8130 ) ;
#21127 = VERTEX_POINT ( 'NONE', #27459 ) ;
#21126 = CARTESIAN_POINT ( 'NONE',  ( 2.274274201625327230, 9.915734732513220351, 4.762163868918306342 ) ) ;
#21128 = VERTEX_POINT ( 'NONE', #16569 ) ;
#21129 = CARTESIAN_POINT ( 'NONE',  ( 48.06508596181272708, -7.548662730768715079, -4.522129901861164036 ) ) ;
#21130 = CARTESIAN_POINT ( 'NONE',  ( 5.377543748152548098, -6.940565734314625423, 4.007137495034787555 ) ) ;
#21132 = ORIENTED_EDGE ( 'NONE', *, *, #19096, .F. ) ;
#21131 = CARTESIAN_POINT ( 'NONE',  ( 18.88575891862270240, -4.454208744578314949, 3.539106266409321133 ) ) ;
#21133 = ORIENTED_EDGE ( 'NONE', *, *, #17497, .F. ) ;
#21134 = DIRECTION ( 'NONE',  ( 1.000000000000000000, -8.574039729943018344E-17, -0.000000000000000000 ) ) ;
#21135 = CARTESIAN_POINT ( 'NONE',  ( 22.49117028854483635, -21.89694127986737371, -1.202706146049568048 ) ) ;
#21136 = CARTESIAN_POINT ( 'NONE',  ( 20.55552624091252056, -16.63177717300871095, -1.500000000000000666 ) ) ;
#21137 = CARTESIAN_POINT ( 'NONE',  ( 107.9807375830284002, -17.79198810411418918, -4.344786411726714981 ) ) ;
#21138 = LINE ( 'NONE', #7595, #7141 ) ;
#21139 = CARTESIAN_POINT ( 'NONE',  ( -6.912942406915326465, 7.727249047114547632E-16, -2.999999999999999556 ) ) ;
#21140 = CARTESIAN_POINT ( 'NONE',  ( 1.750000000000000222, -8.497168642645963388, -0.2193742428685781509 ) ) ;
#21141 = CARTESIAN_POINT ( 'NONE',  ( 69.08947486655651460, -6.491576118626577241, 3.390608973714449359 ) ) ;
#21142 = CARTESIAN_POINT ( 'NONE',  ( -0.9232102171129841217, 0.000000000000000000, 4.522129901861158707 ) ) ;
#21143 = CARTESIAN_POINT ( 'NONE',  ( 6.356382477965132338, 5.080803740829814785, -6.947086032709882453 ) ) ;
#21144 = ORIENTED_EDGE ( 'NONE', *, *, #6176, .T. ) ;
#21145 = CARTESIAN_POINT ( 'NONE',  ( 109.4480141202987369, 20.58379936219382245, 1.732900863439792660 ) ) ;
#21146 =( BOUNDED_CURVE ( )  B_SPLINE_CURVE ( 2, ( #10636, #18011, #22708, #23013, #15479, #28050, #9980, #455, #20843, #23205, #133 ),
 .UNSPECIFIED., .F., .F. ) 
 B_SPLINE_CURVE_WITH_KNOTS ( ( 3, 2, 2, 2, 2, 3 ),
 ( 0.06038226199343772749, 0.06250000000000000000, 0.07812500000000000000, 0.09375000000000000000, 0.1093750000000000000, 0.1228822619934377414 ),
 .UNSPECIFIED. ) 
 CURVE ( )  GEOMETRIC_REPRESENTATION_ITEM ( )  RATIONAL_B_SPLINE_CURVE ( ( 0.9821626249036858880, 0.9896829947469992783, 1.000000000000000000, 0.9238795325112867385, 1.000000000000000000, 0.9238795325112867385, 1.000000000000000000, 0.9238795325112867385, 1.000000000000000000, 0.9341965377642873491, 0.9821626249036861100 ) ) 
 REPRESENTATION_ITEM ( '' )  );
#21147 = CARTESIAN_POINT ( 'NONE',  ( 107.2640681281281729, 16.88755960000358414, 2.548738122058122446 ) ) ;
#21148 = EDGE_CURVE ( 'NONE', #2834, #4033, #24565, .T. ) ;
#21149 = LINE ( 'NONE', #18618, #13497 ) ;
#21150 = ORIENTED_EDGE ( 'NONE', *, *, #15508, .T. ) ;
#21151 = CARTESIAN_POINT ( 'NONE',  ( 22.98500000136559507, -0.9349337715887248157, 3.156283516753367824 ) ) ;
#21152 = EDGE_CURVE ( 'NONE', #15187, #16550, #22409, .T. ) ;
#21153 = CARTESIAN_POINT ( 'NONE',  ( 25.51240124312818480, -1.336128462440899334, -2.459621423140391894 ) ) ;
#21154 = CARTESIAN_POINT ( 'NONE',  ( 20.72551590764745910, -21.66366526924183233, -1.459983613673072167 ) ) ;
#21155 = ORIENTED_EDGE ( 'NONE', *, *, #9644, .T. ) ;
#21156 = CARTESIAN_POINT ( 'NONE',  ( 6.038145268433178892, 6.771555838910925829, -5.096160642893582171 ) ) ;
#21157 = SHAPE_REPRESENTATION_RELATIONSHIP ( 'NONE' , 'NONE' ,  #30799, #30736 ) ;
#21158 = VERTEX_POINT ( 'NONE', #3897 ) ;
#21159 = VERTEX_POINT ( 'NONE', #6871 ) ;
#21160 = CARTESIAN_POINT ( 'NONE',  ( 25.41068576271571544, -17.53965252855327961, -1.057866664603150708 ) ) ;
#21161 = DATE_AND_TIME ( #2974, #1846 ) ;
#21163 = ORIENTED_EDGE ( 'NONE', *, *, #26603, .T. ) ;
#21162 = CARTESIAN_POINT ( 'NONE',  ( -3.659776827764270379, -1.633636780108817854, -0.9788672205760856615 ) ) ;
#21164 = EDGE_LOOP ( 'NONE', ( #14673, #14467, #6738 ) ) ;
#21165 = CARTESIAN_POINT ( 'NONE',  ( 25.04750000136559507, -3.024605502323851169, 0.3178988483021052969 ) ) ;
#21166 = ORIENTED_EDGE ( 'NONE', *, *, #5908, .T. ) ;
#21167 = CARTESIAN_POINT ( 'NONE',  ( -1.750050802731187405, -0.3135853898029607456, 2.983565686104819648 ) ) ;
#21169 = ORIENTED_EDGE ( 'NONE', *, *, #8616, .T. ) ;
#21168 = CARTESIAN_POINT ( 'NONE',  ( -2.286883085291277595, 1.186209272513202517, 3.262832825226773092 ) ) ;
#21170 = CARTESIAN_POINT ( 'NONE',  ( 0.000000000000000000, 0.000000000000000000, 0.000000000000000000 ) ) ;
#21171 = CARTESIAN_POINT ( 'NONE',  ( 5.887529311434773760, -0.3723788567093893609, 8.386653846779019261 ) ) ;
#21172 = CARTESIAN_POINT ( 'NONE',  ( -14.85000000000000142, -10.96966150227469328, 4.000000000000000000 ) ) ;
#21173 = CARTESIAN_POINT ( 'NONE',  ( 0.3076688774149766714, 10.04057401064417654, -2.239519426675632197 ) ) ;
#21174 = CARTESIAN_POINT ( 'NONE',  ( 0.000000000000000000, 6.745408891279611296, -5.171987904998036178 ) ) ;
#21175 = ORIENTED_EDGE ( 'NONE', *, *, #16698, .T. ) ;
#21176 = B_SPLINE_CURVE_WITH_KNOTS ( 'NONE', 3,
 ( #9653, #12514, #32763, #12168, #27707, #19879, #7831, #4658, #18024, #23027, #27887, #28064 ),
 .UNSPECIFIED., .F., .F.,
 ( 4, 2, 2, 2, 2, 4 ),
 ( 0.000000000000000000, 4.210616338135260222E-05, 8.421232676270520444E-05, 0.0001684246535254206817, 0.0003368493070508517717, 0.0006736986141017032182 ),
 .UNSPECIFIED. ) ;
#21177 = DIRECTION ( 'NONE',  ( -0.000000000000000000, -0.000000000000000000, -1.000000000000000000 ) ) ;
#21178 = CARTESIAN_POINT ( 'NONE',  ( 11.04311965146451335, 15.00000000000000355, -1.500000000000000000 ) ) ;
#21179 = CARTESIAN_POINT ( 'NONE',  ( 55.02116481234001810, -8.082960297851709441, -1.169950777210956083 ) ) ;
#21180 = DIRECTION ( 'NONE',  ( 0.000000000000000000, 0.8191520442889864695, 0.5735764363510537089 ) ) ;
#21181 = EDGE_CURVE ( 'NONE', #1933, #22549, #7690, .T. ) ;
#21182 = CARTESIAN_POINT ( 'NONE',  ( 6.038145077921538650, 7.799182446117193912, 3.316258947000888302 ) ) ;
#21183 = CARTESIAN_POINT ( 'NONE',  ( 22.23605616177110278, -21.82696876987042600, 1.456498850422674574 ) ) ;
#21184 = CARTESIAN_POINT ( 'NONE',  ( -50.60000000000000142, 0.000000000000000000, -1.000000000000000000 ) ) ;
#21185 = CARTESIAN_POINT ( 'NONE',  ( 7.249760686538667009, 7.906491560603716273, -3.748318449932209973 ) ) ;
#21186 = CARTESIAN_POINT ( 'NONE',  ( 102.3434546416268773, -2.854938759700320627, 3.993434327340286583 ) ) ;
#21187 = CARTESIAN_POINT ( 'NONE',  ( -4.412550801365593856, -1.828967928396026510, 3.368539882008728004 ) ) ;
#21188 = ORIENTED_EDGE ( 'NONE', *, *, #18081, .T. ) ;
#21189 = CARTESIAN_POINT ( 'NONE',  ( -5.650050800000000706, -1.549418761218565477, 2.853674364686380471 ) ) ;
#21190 = CARTESIAN_POINT ( 'NONE',  ( 10.90258948330155953, 17.51112508050605854, -4.612695725900421984 ) ) ;
#21191 = CYLINDRICAL_SURFACE ( 'NONE', #11387, 2.499999999999997780 ) ;
#21192 = CARTESIAN_POINT ( 'NONE',  ( 8.486535498532832733, -10.66169397763358795, 1.500000000000000000 ) ) ;
#21193 = ORIENTED_EDGE ( 'NONE', *, *, #28457, .T. ) ;
#21194 = CARTESIAN_POINT ( 'NONE',  ( 54.92448458019108415, -4.608697703005007362, -2.787782628541026320 ) ) ;
#21195 = EDGE_LOOP ( 'NONE', ( #4576, #1017, #338, #11904 ) ) ;
#21196 = CARTESIAN_POINT ( 'NONE',  ( 2.303449397150664435, -1.057836737633686353, 1.500000000000000000 ) ) ;
#21197 = APPROVAL_ROLE ( '' ) ;
#21198 = EDGE_CURVE ( 'NONE', #3400, #14263, #2204, .T. ) ;
#21199 = CARTESIAN_POINT ( 'NONE',  ( 102.3664313161174420, -3.178976151102068215, 4.275175836097663051 ) ) ;
#21200 = DIRECTION ( 'NONE',  ( -6.062761635205589313E-17, -0.7071067811865484609, 0.7071067811865465735 ) ) ;
#21201 = CARTESIAN_POINT ( 'NONE',  ( 7.577572045913208321, 15.00000000000002132, 4.629213727441584325 ) ) ;
#21202 = ORIENTED_EDGE ( 'NONE', *, *, #19584, .F. ) ;
#21203 = ADVANCED_FACE ( 'NONE', ( #9718 ), #25438, .T. ) ;
#21204 = CARTESIAN_POINT ( 'NONE',  ( -31.59999999999999787, -25.43932300454937945, 11.50000000000000000 ) ) ;
#21205 = DIRECTION ( 'NONE',  ( 0.000000000000000000, -0.5735764363510552633, 0.8191520442889853593 ) ) ;
#21206 = CARTESIAN_POINT ( 'NONE',  ( 8.862909208978496878, -0.2945138977690186510, 1.470869863057392424 ) ) ;
#21208 = ORIENTED_EDGE ( 'NONE', *, *, #14493, .F. ) ;
#21207 = DIRECTION ( 'NONE',  ( -1.000000000000000000, 0.000000000000000000, 0.000000000000000000 ) ) ;
#21209 = CARTESIAN_POINT ( 'NONE',  ( -4.112550801365593145, -1.088641768524163389, -3.675193018007246071 ) ) ;
#21210 = ADVANCED_FACE ( 'NONE', ( #26 ), #5058, .T. ) ;
#21211 = CARTESIAN_POINT ( 'NONE',  ( 3.499999999999999556, -8.497168642645966941, 0.2193742428684632428 ) ) ;
#21212 = DIRECTION ( 'NONE',  ( 1.000000000000000000, -8.574039729943018344E-17, -0.000000000000000000 ) ) ;
#21213 = EDGE_LOOP ( 'NONE', ( #27291, #29279, #408 ) ) ;
#21214 = EDGE_LOOP ( 'NONE', ( #4244, #3339, #13094, #26647 ) ) ;
#21215 = DIRECTION ( 'NONE',  ( 0.000000000000000000, 0.000000000000000000, -1.000000000000000000 ) ) ;
#21216 = DIRECTION ( 'NONE',  ( 1.000000000000000000, -8.574039729943018344E-17, -0.000000000000000000 ) ) ;
#21217 = ADVANCED_FACE ( 'NONE', ( #18070 ), #14884, .T. ) ;
#21218 = EDGE_CURVE ( 'NONE', #21729, #26855, #21778, .T. ) ;
#21219 = FACE_OUTER_BOUND ( 'NONE', #18276, .T. ) ;
#21220 = CARTESIAN_POINT ( 'NONE',  ( 0.5704036742843073826, -8.851103337321047704, 3.563415854978290387 ) ) ;
#21221 = CARTESIAN_POINT ( 'NONE',  ( -1.928625734671288505, 0.6478360620448558871, 3.177561564833204066 ) ) ;
#21222 = CARTESIAN_POINT ( 'NONE',  ( -3.137550801365593500, 3.368539882008727115, 1.828967928396027176 ) ) ;
#21223 = LINE ( 'NONE', #26423, #23623 ) ;
#21224 = CARTESIAN_POINT ( 'NONE',  ( 102.5330529704723546, -5.572982809272949645, 1.169950773226209106 ) ) ;
#21225 = EDGE_LOOP ( 'NONE', ( #28933, #28992, #9522, #27771 ) ) ;
#21226 = CARTESIAN_POINT ( 'NONE',  ( -33.81874022276151237, 19.50000000000000000, -1.818740222761502601 ) ) ;
#21227 = EDGE_CURVE ( 'NONE', #12922, #13681, #22918, .T. ) ;
#21228 = VERTEX_POINT ( 'NONE', #7376 ) ;
#21229 = PERSON_AND_ORGANIZATION ( #6766, #25292 ) ;
#21230 = CARTESIAN_POINT ( 'NONE',  ( 7.249760686538667009, 6.139290821770327256, -5.151476664237414127 ) ) ;
#21231 = EDGE_CURVE ( 'NONE', #29357, #10953, #31535, .T. ) ;
#21232 = FACE_OUTER_BOUND ( 'NONE', #15209, .T. ) ;
#21233 = VERTEX_POINT ( 'NONE', #20602 ) ;
#21234 = CARTESIAN_POINT ( 'NONE',  ( 25.75999999999999801, -2.208672634433321348E-15, 0.000000000000000000 ) ) ;
#21235 = ORIENTED_EDGE ( 'NONE', *, *, #4305, .F. ) ;
#21236 = EDGE_LOOP ( 'NONE', ( #25801, #20745, #20995, #6941 ) ) ;
#21237 = MANIFOLD_SOLID_BREP ( 'CirPattern1', #8665 ) ;
#21238 = DIRECTION ( 'NONE',  ( -1.000000000000000000, -0.000000000000000000, 0.000000000000000000 ) ) ;
#21239 = CARTESIAN_POINT ( 'NONE',  ( -5.662550801365592967, 0.3701630799359330593, -3.521866450007987037 ) ) ;
#21240 = CARTESIAN_POINT ( 'NONE',  ( 6.963573770753491488, -4.510305581628904825, 1.500000000000000444 ) ) ;
#21241 = CARTESIAN_POINT ( 'NONE',  ( 0.2683958477397258569, -5.146640226071303559, -1.768824076817805402 ) ) ;
#21243 = ORIENTED_EDGE ( 'NONE', *, *, #20049, .T. ) ;
#21242 = CARTESIAN_POINT ( 'NONE',  ( 14.29326447320846682, 9.302996554324566958, -1.500000000000000222 ) ) ;
#21244 = CARTESIAN_POINT ( 'NONE',  ( -7.487550801365594033, -2.228590825266444586, -2.752080473201636401 ) ) ;
#21245 = CARTESIAN_POINT ( 'NONE',  ( 9.923352537767708981, 1.153138503616545796, 1.499999999999881650 ) ) ;
#21246 = FACE_OUTER_BOUND ( 'NONE', #28263, .T. ) ;
#21247 = DIRECTION ( 'NONE',  ( -0.03487826274237759705, -0.9987827659587180662, -0.03487826274237711827 ) ) ;
#21248 = EDGE_CURVE ( 'NONE', #5341, #15697, #10210, .T. ) ;
#21250 = VERTEX_POINT ( 'NONE', #22423 ) ;
#21249 = CARTESIAN_POINT ( 'NONE',  ( 21.03177542174608661, -17.18603084754167298, 1.753176640694532162 ) ) ;
#21251 = CARTESIAN_POINT ( 'NONE',  ( 25.75999999999999801, -2.208672634433321348E-15, 0.000000000000000000 ) ) ;
#21252 = LINE ( 'NONE', #6523, #8803 ) ;
#21253 = EDGE_CURVE ( 'NONE', #19227, #2042, #20433, .T. ) ;
#21254 = EDGE_CURVE ( 'NONE', #7219, #12210, #17626, .T. ) ;
#21255 = CARTESIAN_POINT ( 'NONE',  ( 25.75999999999999801, -2.208672634433321348E-15, 0.000000000000000000 ) ) ;
#21256 = CARTESIAN_POINT ( 'NONE',  ( 101.8016823592329274, -4.042758964359259188, -3.993434276136486716 ) ) ;
#21257 = CARTESIAN_POINT ( 'NONE',  ( -2.962625823238647982, -0.001292792641206102827, -0.8472062597617540103 ) ) ;
#21258 = CARTESIAN_POINT ( 'NONE',  ( 3.499999999999999556, 4.137773741518377513, 5.705158055754806945 ) ) ;
#21259 = CARTESIAN_POINT ( 'NONE',  ( 109.1472041058640912, 18.90877050785832836, -4.999054092451833853 ) ) ;
#21260 = CARTESIAN_POINT ( 'NONE',  ( -5.587550801365593678, 3.521866450007987037, 0.3701630799359328372 ) ) ;
#21261 = ORIENTED_EDGE ( 'NONE', *, *, #28255, .F. ) ;
#21262 = CARTESIAN_POINT ( 'NONE',  ( 1.624999999999999778, 10.90201369670498721, -1.464956435139580515 ) ) ;
#21263 = CARTESIAN_POINT ( 'NONE',  ( 101.8016823592330127, -4.042758964360499974, 3.993434276137187489 ) ) ;
#21264 = CARTESIAN_POINT ( 'NONE',  ( 0.000000000000000000, -6.200809695932770538, -0.7745709230445805282 ) ) ;
#21266 = CARTESIAN_POINT ( 'NONE',  ( 107.9910885158944041, -17.94103896239631979, 4.566504411386732798 ) ) ;
#21265 = DIRECTION ( 'NONE',  ( 0.000000000000000000, 0.9659258262890693114, -0.2588190451025167427 ) ) ;
#21267 = ORIENTED_EDGE ( 'NONE', *, *, #15312, .T. ) ;
#21268 = EDGE_CURVE ( 'NONE', #16695, #12771, #1298, .T. ) ;
#21269 = CC_DESIGN_DATE_AND_TIME_ASSIGNMENT ( #4661, #14834, ( #31711 ) ) ;
#21270 = DIRECTION ( 'NONE',  ( 0.000000000000000000, 0.000000000000000000, 1.000000000000000000 ) ) ;
#21271 = ORIENTED_EDGE ( 'NONE', *, *, #14781, .F. ) ;
#21273 = VERTEX_POINT ( 'NONE', #25275 ) ;
#21272 = CARTESIAN_POINT ( 'NONE',  ( 108.3696618535068126, 20.23658298680886247, -1.378742097822665436 ) ) ;
#21274 = VERTEX_POINT ( 'NONE', #12564 ) ;
#21275 = LINE ( 'NONE', #8259, #9155 ) ;
#21276 = DIRECTION ( 'NONE',  ( -1.000000000000000000, 0.000000000000000000, 0.000000000000000000 ) ) ;
#21278 = ORIENTED_EDGE ( 'NONE', *, *, #3322, .T. ) ;
#21277 = CARTESIAN_POINT ( 'NONE',  ( 18.94426840742758245, -3.800190086666909828, 2.484897251481009040 ) ) ;
#21279 = CARTESIAN_POINT ( 'NONE',  ( 15.60185111446442541, 10.48692277156955299, -1.499999999999998446 ) ) ;
#21280 = CARTESIAN_POINT ( 'NONE',  ( 3.722807861074314939, -17.21380748779928993, -1.747812250015838176 ) ) ;
#21281 = DIRECTION ( 'NONE',  ( 0.000000000000000000, 0.3090169943749412895, 0.9510565162951555296 ) ) ;
#21282 = CARTESIAN_POINT ( 'NONE',  ( 9.331062908042635939, 15.00000000000000178, -4.612695725900422872 ) ) ;
#21283 = CARTESIAN_POINT ( 'NONE',  ( 107.4494260027903465, -17.35107267642216655, -4.497208115429102371 ) ) ;
#21284 = DIRECTION ( 'NONE',  ( -1.000000000000000000, 0.000000000000000000, 0.000000000000000000 ) ) ;
#21285 = EDGE_CURVE ( 'NONE', #6857, #7133, #10044, .T. ) ;
#21286 = B_SPLINE_CURVE_WITH_KNOTS ( 'NONE', 3,
 ( #14691, #17199, #4517, #32591, #30104, #7181, #14837, #12339, #23040, #7484 ),
 .UNSPECIFIED., .F., .F.,
 ( 4, 2, 2, 2, 4 ),
 ( 2.571685856657688708E-07, 0.0005478592107668815280, 0.001095461252948097194, 0.001643063295129312644, 0.002190665337310528961 ),
 .UNSPECIFIED. ) ;
#21287 = DIRECTION ( 'NONE',  ( -2.219124775574902609E-17, -0.2588190451025176309, -0.9659258262890692004 ) ) ;
#21288 = CARTESIAN_POINT ( 'NONE',  ( -41.77414131929176477, -16.18685544166627821, 1.500000000000000000 ) ) ;
#21289 = CARTESIAN_POINT ( 'NONE',  ( -2.912942406915326909, 4.884725290497410777E-15, -2.999999999999999556 ) ) ;
#21290 = CARTESIAN_POINT ( 'NONE',  ( 2.648464616715299424, 0.1990047044050357872, 1.630908343631527258 ) ) ;
#21291 = ORIENTED_EDGE ( 'NONE', *, *, #24028, .F. ) ;
#21292 = CARTESIAN_POINT ( 'NONE',  ( 7.249760686538667009, -3.647351267791519636, -7.953573330858250579 ) ) ;
#21293 = FACE_OUTER_BOUND ( 'NONE', #3660, .T. ) ;
#21294 = CARTESIAN_POINT ( 'NONE',  ( 2.661997753583468906, 10.09011512947409805, 0.9074203448822234508 ) ) ;
#21295 = EDGE_LOOP ( 'NONE', ( #20336, #7764, #17104, #7583, #15813, #32806, #30183, #9554, #14808, #18666, #12915, #8222, #2535, #13731, #5593, #13249, #12623, #857, #23998, #30948, #6555, #28998, #18411, #25750, #16678, #16284, #11265, #22179, #15274, #8344, #22909, #23398, #16882, #9558, #29070, #9579, #1088, #19159, #25067, #6394, #27456, #29637, #28650, #10203, #13755, #1218, #10670, #21942, #16850, #26425, #3714, #32406, #19936, #6845, #15078, #20567, #15267, #22680, #9267, #25610, #20574, #356, #24025, #27022, #1041, #4227, #6634, #15537, #28577, #31181, #7435, #22689, #17944, #9699, #1915, #18194, #746, #11718, #28950, #16294, #17593, #27234, #25722, #11159, #23184, #8688, #6897, #31426, #7803, #12644, #1927, #20171, #3219, #32507, #28203, #4324, #12631, #32149, #26413, #31778, #3279, #32506, #18356, #5203, #29989, #20277, #13192, #5123 ) ) ;
#21296 = CYLINDRICAL_SURFACE ( 'NONE', #13550, 3.000000000000000444 ) ;
#21297 = CARTESIAN_POINT ( 'NONE',  ( 20.69942760064582998, -21.74528614261393500, -1.396244390127318491 ) ) ;
#21298 = ORIENTED_EDGE ( 'NONE', *, *, #20518, .F. ) ;
#21299 = CARTESIAN_POINT ( 'NONE',  ( 10.97445643284022587, -14.84313750102852225, -1.499999999999999112 ) ) ;
#21300 = EDGE_CURVE ( 'NONE', #32970, #15150, #6086, .T. ) ;
#21301 = VERTEX_POINT ( 'NONE', #15885 ) ;
#21302 = ORIENTED_EDGE ( 'NONE', *, *, #20631, .T. ) ;
#21303 = CARTESIAN_POINT ( 'NONE',  ( 29.38825086720286350, -3.456623792451285482, -2.713652344655540727 ) ) ;
#21304 = PERSON_AND_ORGANIZATION_ROLE ( 'classification_officer' ) ;
#21306 = ORIENTED_EDGE ( 'NONE', *, *, #1872, .F. ) ;
#21305 = CARTESIAN_POINT ( 'NONE',  ( 6.691656545361666986, -18.99987508458807639, -0.9788672205760856615 ) ) ;
#21307 = ORIENTED_EDGE ( 'NONE', *, *, #13487, .F. ) ;
#21308 = DIRECTION ( 'NONE',  ( -1.000000000000000000, 0.000000000000000000, 0.000000000000000000 ) ) ;
#21309 = ORIENTED_EDGE ( 'NONE', *, *, #3631, .F. ) ;
#21310 = CARTESIAN_POINT ( 'NONE',  ( 0.000000000000000000, 0.000000000000000000, 0.000000000000000000 ) ) ;
#21312 = ORIENTED_EDGE ( 'NONE', *, *, #25146, .F. ) ;
#21311 = CARTESIAN_POINT ( 'NONE',  ( 41.34428855215451648, -4.040999237037778968, -1.169951068919291348 ) ) ;
#21313 = LINE ( 'NONE', #14120, #19359 ) ;
#21314 = FACE_OUTER_BOUND ( 'NONE', #9036, .T. ) ;
#21315 = EDGE_CURVE ( 'NONE', #4711, #15980, #11193, .T. ) ;
#21316 = CYLINDRICAL_SURFACE ( 'NONE', #16227, 5.010000000000000675 ) ;
#21317 = CARTESIAN_POINT ( 'NONE',  ( 5.612974441954673210, 5.126870824538761973, 6.420536856479951204 ) ) ;
#21318 = EDGE_CURVE ( 'NONE', #11856, #7812, #9069, .T. ) ;
#21319 = CARTESIAN_POINT ( 'NONE',  ( 108.0290699101298202, -18.48796159080449542, 4.329927758675821359 ) ) ;
#21320 =( BOUNDED_CURVE ( )  B_SPLINE_CURVE ( 3, ( #21851, #11339, #27043, #4146 ),
 .UNSPECIFIED., .F., .F. ) 
 B_SPLINE_CURVE_WITH_KNOTS ( ( 4, 4 ),
 ( 4.520402762664171625, 4.712388980383413362 ),
 .UNSPECIFIED. ) 
 CURVE ( )  GEOMETRIC_REPRESENTATION_ITEM ( )  RATIONAL_B_SPLINE_CURVE ( ( 1.000000000000000000, 0.9969307989114568613, 0.9969307989114568613, 1.000000000000000000 ) ) 
 REPRESENTATION_ITEM ( '' )  );
#21321 = EDGE_CURVE ( 'NONE', #25915, #17424, #5382, .T. ) ;
#21322 = DIRECTION ( 'NONE',  ( -1.000000000000000000, 0.000000000000000000, 0.000000000000000000 ) ) ;
#21323 = CYLINDRICAL_SURFACE ( 'NONE', #25681, 5.010000000000000675 ) ;
#21324 = CARTESIAN_POINT ( 'NONE',  ( 17.41559371906256004, 18.02474698348863669, 1.508259000770581615 ) ) ;
#21325 = DIRECTION ( 'NONE',  ( 0.000000000000000000, 0.5735764363510496011, -0.8191520442889893561 ) ) ;
#21326 = DIRECTION ( 'NONE',  ( 0.000000000000000000, -0.000000000000000000, -1.000000000000000000 ) ) ;
#21327 = DIRECTION ( 'NONE',  ( 1.000000000000000000, -0.000000000000000000, 0.000000000000000000 ) ) ;
#21328 = DIRECTION ( 'NONE',  ( 3.623545766764302137E-17, 0.4226182617407097108, -0.9063077870366451627 ) ) ;
#21329 = CARTESIAN_POINT ( 'NONE',  ( 21.34414429286333714, -21.72097900651761648, 1.443623072031003485 ) ) ;
#21330 = DIRECTION ( 'NONE',  ( 0.000000000000000000, 1.000000000000000000, 0.000000000000000000 ) ) ;
#21331 = CARTESIAN_POINT ( 'NONE',  ( -2.862550801365593145, -0.3701630799359326152, 3.521866450007987037 ) ) ;
#21332 = VERTEX_POINT ( 'NONE', #16375 ) ;
#21333 = CARTESIAN_POINT ( 'NONE',  ( -7.050050800000000173, -2.853674364686378695, -1.549418761218566809 ) ) ;
#21334 = CIRCLE ( 'NONE', #32565, 2.099999999999997868 ) ;
#21335 = AXIS2_PLACEMENT_3D ( 'NONE', #17679, #4196, #27094 ) ;
#21336 = CARTESIAN_POINT ( 'NONE',  ( 7.249760686538667009, -4.007137495034861274, 6.940565734314584567 ) ) ;
#21337 = CARTESIAN_POINT ( 'NONE',  ( 3.499999999999999556, -5.979767908488830663, -1.814490771706242622 ) ) ;
#21338 = CARTESIAN_POINT ( 'NONE',  ( -41.04966659693692321, -14.04895890769333811, 5.700525207345996215 ) ) ;
#21339 = ORIENTED_EDGE ( 'NONE', *, *, #6899, .T. ) ;
#21340 = DIRECTION ( 'NONE',  ( 1.000000000000000000, -0.000000000000000000, -0.000000000000000000 ) ) ;
#21341 = CIRCLE ( 'NONE', #12782, 11.00000000000000000 ) ;
#21342 = VERTEX_POINT ( 'NONE', #13207 ) ;
#21343 = CARTESIAN_POINT ( 'NONE',  ( 0.2685008736531913076, -5.146116540876891854, 1.768822251658703326 ) ) ;
#21344 = APPROVAL_STATUS ( 'not_yet_approved' ) ;
#21345 = CARTESIAN_POINT ( 'NONE',  ( 28.67878734107726046, -6.190522357109429663, 4.312042181584448741 ) ) ;
#21346 = EDGE_CURVE ( 'NONE', #28496, #31361, #3779, .T. ) ;
#21347 = LINE ( 'NONE', #3498, #16565 ) ;
#21348 = CARTESIAN_POINT ( 'NONE',  ( 23.85741365831132654, -17.28578219493638812, -1.405688364266028056 ) ) ;
#21349 = CARTESIAN_POINT ( 'NONE',  ( 8.901201215455847304, 15.00000000000002132, 5.412820279296879811 ) ) ;
#21350 = ORIENTED_EDGE ( 'NONE', *, *, #27945, .F. ) ;
#21351 = EDGE_CURVE ( 'NONE', #27551, #5304, #32012, .T. ) ;
#21352 = DIRECTION ( 'NONE',  ( 0.000000000000000000, 0.000000000000000000, -1.000000000000000000 ) ) ;
#21353 = CARTESIAN_POINT ( 'NONE',  ( 0.1574692247319865734, 10.55579611470142609, -1.187839595765044942 ) ) ;
#21354 = DIRECTION ( 'NONE',  ( 1.000000000000000000, -0.000000000000000000, -0.000000000000000000 ) ) ;
#21355 = EDGE_CURVE ( 'NONE', #72, #22098, #31019, .T. ) ;
#21356 = VECTOR ( 'NONE', #23310, 1000.000000000000114 ) ;
#21358 = ORIENTED_EDGE ( 'NONE', *, *, #1221, .T. ) ;
#21357 = CARTESIAN_POINT ( 'NONE',  ( 108.1382412073544685, 18.94794151480644118, -4.129322685383101543 ) ) ;
#21359 = CARTESIAN_POINT ( 'NONE',  ( -4.162550801365592967, -2.228590825266444586, -2.752080473201636401 ) ) ;
#21360 = CIRCLE ( 'NONE', #24015, 2.499999999999996891 ) ;
#21361 = CARTESIAN_POINT ( 'NONE',  ( 108.3358872576213230, 20.04851271009933456, 1.796441256565045386 ) ) ;
#21362 = CARTESIAN_POINT ( 'NONE',  ( 55.00858942667153428, -7.632540988256709902, -2.184956776153270219 ) ) ;
#21363 = ORIENTED_EDGE ( 'NONE', *, *, #16125, .T. ) ;
#21364 = ORIENTED_EDGE ( 'NONE', *, *, #5326, .F. ) ;
#21365 = CIRCLE ( 'NONE', #20825, 4.000000000000001776 ) ;
#21366 = CARTESIAN_POINT ( 'NONE',  ( 108.0374854960985687, -18.60914393521796839, 4.376826314212413749 ) ) ;
#21367 = CARTESIAN_POINT ( 'NONE',  ( -23.54713438637982748, 3.520075575296777171, 1.500000000000000000 ) ) ;
#21368 = CARTESIAN_POINT ( 'NONE',  ( 108.1300413742128228, -19.95926608421463300, 1.392287898181946426 ) ) ;
#21369 = CARTESIAN_POINT ( 'NONE',  ( 13.54302414779168373, -18.70685303420125223, 5.485967528433935314 ) ) ;
#21370 = CARTESIAN_POINT ( 'NONE',  ( 24.73877499206001218, -17.41122639143721784, 1.266735320468793224 ) ) ;
#21371 = EDGE_LOOP ( 'NONE', ( #5059, #19011, #7693, #6597 ) ) ;
#21372 = CARTESIAN_POINT ( 'NONE',  ( -8.404531657079157725, 2.325406398514293205, -1.883076972206379374 ) ) ;
#21373 = DIRECTION ( 'NONE',  ( -1.000000000000000000, -0.000000000000000000, -0.000000000000000000 ) ) ;
#21374 = CARTESIAN_POINT ( 'NONE',  ( -4.287550801365592967, -2.228590825266444586, -2.752080473201636401 ) ) ;
#21375 = AXIS2_PLACEMENT_3D ( 'NONE', #8165, #28716, #18371 ) ;
#21376 = CARTESIAN_POINT ( 'NONE',  ( 0.000000000000000000, -0.5000000000000000000, -1.500000000000000000 ) ) ;
#21377 = CARTESIAN_POINT ( 'NONE',  ( 18.62691943105422254, -7.347514731317398073, 1.529339877370982981 ) ) ;
#21378 = ORIENTED_EDGE ( 'NONE', *, *, #22165, .T. ) ;
#21379 = CARTESIAN_POINT ( 'NONE',  ( 7.064423637759000840, -2.318425219013664496, 8.437262856155488322 ) ) ;
#21380 = AXIS2_PLACEMENT_3D ( 'NONE', #21101, #6036, #13367 ) ;
#21381 = AXIS2_PLACEMENT_3D ( 'NONE', #13699, #28611, #696 ) ;
#21383 = EDGE_CURVE ( 'NONE', #20134, #29829, #2181, .T. ) ;
#21382 = ORIENTED_EDGE ( 'NONE', *, *, #24520, .T. ) ;
#21384 = CALENDAR_DATE ( 2026, 6, 10 ) ;
#21385 = CARTESIAN_POINT ( 'NONE',  ( 54.97720174176811980, -6.505747997631214474, 3.994702633076089082 ) ) ;
#21386 = AXIS2_PLACEMENT_3D ( 'NONE', #11811, #27533, #22018 ) ;
#21387 = CIRCLE ( 'NONE', #13349, 6.248999999999999666 ) ;
#21388 = ADVANCED_FACE ( 'NONE', ( #10543 ), #8696, .T. ) ;
#21389 = CARTESIAN_POINT ( 'NONE',  ( 9.369450431866805928, -11.55901544634946987, -0.9999999999999997780 ) ) ;
#21390 = VERTEX_POINT ( 'NONE', #5847 ) ;
#21391 = CARTESIAN_POINT ( 'NONE',  ( 0.6791197464446975252, -9.138998021039022035, 0.5477823182330348040 ) ) ;
#21392 = ORIENTED_EDGE ( 'NONE', *, *, #28457, .F. ) ;
#21393 = VERTEX_POINT ( 'NONE', #13065 ) ;
#21394 = EDGE_CURVE ( 'NONE', #10544, #29208, #27775, .T. ) ;
#21395 = CARTESIAN_POINT ( 'NONE',  ( 0.1610798642962581184, -10.72944008624797974, -4.522129901861164925 ) ) ;
#21396 = CARTESIAN_POINT ( 'NONE',  ( -4.112550801365593145, -1.088641768524163611, -3.675193018007245627 ) ) ;
#21397 = CARTESIAN_POINT ( 'NONE',  ( 10.51239158225386383, -12.94889321834415341, 1.500000000000000000 ) ) ;
#21398 = CARTESIAN_POINT ( 'NONE',  ( 0.2475851010963652510, -6.181414723257675270, -1.499999999999999556 ) ) ;
#21400 = VERTEX_POINT ( 'NONE', #20915 ) ;
#21399 = CARTESIAN_POINT ( 'NONE',  ( 0.3749742512057836485, -5.190538276685865426, 8.659825570211395984 ) ) ;
#21401 = CARTESIAN_POINT ( 'NONE',  ( -6.237550801365593145, 1.088641768524161613, 3.675193018007247403 ) ) ;
#21402 = CARTESIAN_POINT ( 'NONE',  ( 17.22494247561739300, 13.33946157486217032, 1.500000000000000000 ) ) ;
#21403 = CIRCLE ( 'NONE', #15527, 5.100000000000000533 ) ;
#21404 = EDGE_CURVE ( 'NONE', #24410, #2361, #19644, .T. ) ;
#21405 = CARTESIAN_POINT ( 'NONE',  ( 56.97280603064898941, -277.2763395528616002, 5.471072653610983494 ) ) ;
#21406 = CARTESIAN_POINT ( 'NONE',  ( 21.04750000136559507, -3.024605502323851169, 0.3178988483021052969 ) ) ;
#21407 = AXIS2_PLACEMENT_3D ( 'NONE', #20251, #23093, #25768 ) ;
#21409 = VERTEX_POINT ( 'NONE', #11533 ) ;
#21408 = CARTESIAN_POINT ( 'NONE',  ( 3.499999999999999556, 0.000000000000000000, 0.000000000000000000 ) ) ;
#21410 = AXIS2_PLACEMENT_3D ( 'NONE', #31263, #21696, #18533 ) ;
#21411 = DIRECTION ( 'NONE',  ( -1.000000000000000000, -0.000000000000000000, -0.000000000000000000 ) ) ;
#21412 = CARTESIAN_POINT ( 'NONE',  ( 20.98500000273118715, -0.2613211581691358698, -2.486304738420681559 ) ) ;
#21413 = CARTESIAN_POINT ( 'NONE',  ( 5.887529755120530339, -1.089605374054316789, -8.323904922804405970 ) ) ;
#21414 = EDGE_CURVE ( 'NONE', #24368, #12536, #10461, .T. ) ;
#21415 = LINE ( 'NONE', #8385, #10232 ) ;
#21416 = DIRECTION ( 'NONE',  ( -0.000000000000000000, 0.3746065934159164001, -0.9271838545667856479 ) ) ;
#21417 = CARTESIAN_POINT ( 'NONE',  ( 3.063284526846069777, -2.223716399039799452, 8.461683424479977234 ) ) ;
#21418 = CARTESIAN_POINT ( 'NONE',  ( 25.98690466878746008, 22.56136012750956965, 0.4463807625373348298 ) ) ;
#21419 = CARTESIAN_POINT ( 'NONE',  ( -4.537550801365592967, -1.828967928396026510, 3.368539882008728004 ) ) ;
#21420 = ORIENTED_EDGE ( 'NONE', *, *, #26052, .F. ) ;
#21421 = DIRECTION ( 'NONE',  ( 0.000000000000000000, -1.734723475976807094E-15, -1.000000000000000000 ) ) ;
#21422 = AXIS2_PLACEMENT_3D ( 'NONE', #28161, #18121, #27823 ) ;
#21423 = CARTESIAN_POINT ( 'NONE',  ( 2.592584690691854821, 9.468199583002103736, -4.120115534666250134 ) ) ;
#21425 = LINE ( 'NONE', #24081, #19832 ) ;
#21424 = DIRECTION ( 'NONE',  ( -1.000000000000000000, 8.574039729943017111E-17, -0.000000000000000000 ) ) ;
#21426 = ORIENTED_EDGE ( 'NONE', *, *, #16016, .F. ) ;
#21427 = VECTOR ( 'NONE', #32338, 1000.000000000000000 ) ;
#21428 = CARTESIAN_POINT ( 'NONE',  ( 25.43628654896178887, -17.54453578616395504, 1.000000000000000000 ) ) ;
#21429 = CIRCLE ( 'NONE', #32664, 4.000000000000001776 ) ;
#21430 = VERTEX_POINT ( 'NONE', #9003 ) ;
#21431 = FACE_OUTER_BOUND ( 'NONE', #6569, .T. ) ;
#21433 = VERTEX_POINT ( 'NONE', #24734 ) ;
#21432 = CARTESIAN_POINT ( 'NONE',  ( 24.37017644008354722, -17.36705458137034697, 1.347230727348949442 ) ) ;
#21434 = ORIENTED_EDGE ( 'NONE', *, *, #14056, .T. ) ;
#21435 = DIRECTION ( 'NONE',  ( -1.000000000000000000, 8.574039729943018344E-17, -0.000000000000000000 ) ) ;
#21436 = EDGE_CURVE ( 'NONE', #10245, #22148, #26193, .T. ) ;
#21437 = VECTOR ( 'NONE', #4751, 1000.000000000000000 ) ;
#21438 = EDGE_CURVE ( 'NONE', #19582, #25459, #1630, .T. ) ;
#21439 = VECTOR ( 'NONE', #32848, 1000.000000000000227 ) ;
#21441 = AXIS2_PLACEMENT_3D ( 'NONE', #3606, #26818, #23663 ) ;
#21440 = CARTESIAN_POINT ( 'NONE',  ( -6.150050802731187538, 0.3135853898029611342, -2.983565686104819648 ) ) ;
#21443 = VERTEX_POINT ( 'NONE', #27070 ) ;
#21442 = CARTESIAN_POINT ( 'NONE',  ( 107.8490370924046857, 17.33753888827191147, 2.533541893723956662 ) ) ;
#21444 = DIRECTION ( 'NONE',  ( 8.281886410780507329E-17, 0.9659258262890679791, 0.2588190451025216277 ) ) ;
#21445 = DIRECTION ( 'NONE',  ( 0.000000000000000000, 1.000000000000000000, 0.000000000000000000 ) ) ;
#21446 = CARTESIAN_POINT ( 'NONE',  ( 108.0920678934618593, -19.39511687885960356, -2.469487401138616534 ) ) ;
#21447 = CARTESIAN_POINT ( 'NONE',  ( 7.362531901230324749, -8.542914936813222226, -1.499999999999856559 ) ) ;
#21448 = EDGE_CURVE ( 'NONE', #30055, #27447, #26737, .T. ) ;
#21449 = CARTESIAN_POINT ( 'NONE',  ( 107.9488496542534648, -17.33280986247086375, -4.539927485673689311 ) ) ;
#21450 = CARTESIAN_POINT ( 'NONE',  ( -50.81000000000000227, -10.96999999999998643, 5.700000000000000178 ) ) ;
#21451 = CARTESIAN_POINT ( 'NONE',  ( 2.437082427505626203, 4.432669656489596655, -9.703015696712895988 ) ) ;
#21452 = FACE_OUTER_BOUND ( 'NONE', #1262, .T. ) ;
#21453 = CIRCLE ( 'NONE', #15584, 6.500000000000002665 ) ;
#21455 = EDGE_CURVE ( 'NONE', #22729, #28583, #28301, .T. ) ;
#21454 = VECTOR ( 'NONE', #11130, 1000.000000000000000 ) ;
#21456 = CARTESIAN_POINT ( 'NONE',  ( 6.356382228872879736, 8.265862592379924934, 2.398350474621971706 ) ) ;
#21457 = FACE_OUTER_BOUND ( 'NONE', #20573, .T. ) ;
#21458 = CC_DESIGN_DATE_AND_TIME_ASSIGNMENT ( #32356, #29315, ( #32825 ) ) ;
#21459 = ORIENTED_EDGE ( 'NONE', *, *, #11179, .T. ) ;
#21460 = LINE ( 'NONE', #31677, #4958 ) ;
#21461 = CIRCLE ( 'NONE', #19339, 10.00000000000000355 ) ;
#21462 = B_SPLINE_CURVE_WITH_KNOTS ( 'NONE', 3,
 ( #13729, #21432, #30987, #31649 ),
 .UNSPECIFIED., .F., .F.,
 ( 4, 4 ),
 ( -7.558714329344716932E-06, 0.0001212692847099137061 ),
 .UNSPECIFIED. ) ;
#21463 = AXIS2_PLACEMENT_3D ( 'NONE', #13581, #23787, #21276 ) ;
#21464 = CARTESIAN_POINT ( 'NONE',  ( 25.00111451137534146, -4.139597703811366476E-17, -2.499999999999998668 ) ) ;
#21465 = CYLINDRICAL_SURFACE ( 'NONE', #18344, 3.000000000000000444 ) ;
#21466 = VERTEX_POINT ( 'NONE', #24390 ) ;
#21467 = AXIS2_PLACEMENT_3D ( 'NONE', #894, #11071, #19251 ) ;
#21468 = VECTOR ( 'NONE', #14511, 1000.000000000000000 ) ;
#21469 = CARTESIAN_POINT ( 'NONE',  ( 25.40183372063117417, -2.672122287336369251, 0.04926763101708898224 ) ) ;
#21470 = CARTESIAN_POINT ( 'NONE',  ( 78.98737618897432355, 23.37029618663415320, -5.396302277755718357 ) ) ;
#21471 = ORIENTED_EDGE ( 'NONE', *, *, #31969, .T. ) ;
#21472 = DIRECTION ( 'NONE',  ( 0.000000000000000000, 0.08715574274765461316, 0.9961946980917457672 ) ) ;
#21473 = DIRECTION ( 'NONE',  ( 0.000000000000000000, 0.000000000000000000, 1.000000000000000000 ) ) ;
#21474 = EDGE_LOOP ( 'NONE', ( #4160, #8295, #27886, #4682, #18071, #2574, #3563, #14990, #19607, #18635, #5180, #20632 ) ) ;
#21475 = VECTOR ( 'NONE', #31958, 1000.000000000000114 ) ;
#21476 = ORIENTED_EDGE ( 'NONE', *, *, #31969, .F. ) ;
#21477 = CARTESIAN_POINT ( 'NONE',  ( 25.49907528997228923, -17.55969604403593110, -1.109946655923441883 ) ) ;
#21478 = APPROVAL_DATE_TIME ( #29671, #28809 ) ;
#21479 = AXIS2_PLACEMENT_3D ( 'NONE', #12950, #10279, #20660 ) ;
#21481 = EDGE_LOOP ( 'NONE', ( #10612, #5458, #27862, #15299, #20023, #7972, #13126, #620, #23126, #23884, #3371, #7627, #22558, #16410, #4865, #29609, #6748, #10236, #20936, #19694, #16914 ) ) ;
#21480 = DIRECTION ( 'NONE',  ( -1.000000000000000000, -0.000000000000000000, 0.000000000000000000 ) ) ;
#21482 = EDGE_LOOP ( 'NONE', ( #10664, #4773, #28168, #30143 ) ) ;
#21483 = CARTESIAN_POINT ( 'NONE',  ( 25.75999999999999446, 1.024942698525265428, 2.863353032229740691 ) ) ;
#21484 = EDGE_CURVE ( 'NONE', #24130, #16234, #4819, .T. ) ;
#21485 = CIRCLE ( 'NONE', #17204, 0.9999999999999991118 ) ;
#21486 = AXIS2_PLACEMENT_3D ( 'NONE', #10598, #20977, #20804 ) ;
#21487 = CIRCLE ( 'NONE', #32692, 8.500000000000000000 ) ;
#21488 = ORIENTED_EDGE ( 'NONE', *, *, #12649, .F. ) ;
#21489 = CARTESIAN_POINT ( 'NONE',  ( -0.5616989984783457013, -12.44624546261724163, 4.522129901861158707 ) ) ;
#21490 = DIRECTION ( 'NONE',  ( -0.8660254037844397068, 0.4999999999999981681, 0.000000000000000000 ) ) ;
#21492 = ORIENTED_EDGE ( 'NONE', *, *, #9439, .F. ) ;
#21491 = CARTESIAN_POINT ( 'NONE',  ( 4.749760686538667009, 5.151476664237477188, 6.139290821770273077 ) ) ;
#21493 = VECTOR ( 'NONE', #22200, 1000.000000000000114 ) ;
#21494 = CARTESIAN_POINT ( 'NONE',  ( 21.99290772595112387, -0.1310194482076041944, -2.499999999999998224 ) ) ;
#21495 = DIRECTION ( 'NONE',  ( -0.9896144216807899463, 0.000000000000000000, -0.1437473352845038410 ) ) ;
#21496 = LINE ( 'NONE', #21973, #27752 ) ;
#21497 = CARTESIAN_POINT ( 'NONE',  ( 5.865515302491369098, 15.00000000000000000, 1.500000000000000000 ) ) ;
#21499 = CARTESIAN_POINT ( 'NONE',  ( 108.0293210873539067, -18.49157848034651153, 4.320045722282116252 ) ) ;
#21498 = CIRCLE ( 'NONE', #1213, 4.000000000000001776 ) ;
#21500 = CARTESIAN_POINT ( 'NONE',  ( 0.1610798642962581184, -10.72944008624893542, -4.522129901861164925 ) ) ;
#21501 = DIRECTION ( 'NONE',  ( 0.000000000000000000, -1.000000000000000000, 0.000000000000000000 ) ) ;
#21502 = EDGE_CURVE ( 'NONE', #30146, #2248, #2152, .T. ) ;
#21503 = DIRECTION ( 'NONE',  ( -1.000000000000000000, -0.000000000000000000, -0.000000000000000000 ) ) ;
#21504 = CC_DESIGN_DATE_AND_TIME_ASSIGNMENT ( #5196, #10030, ( #1899 ) ) ;
#21505 = VECTOR ( 'NONE', #15737, 999.9999999999998863 ) ;
#21506 = DIRECTION ( 'NONE',  ( 0.000000000000000000, 0.03489949670250103164, -0.9993908270190957621 ) ) ;
#21507 = CARTESIAN_POINT ( 'NONE',  ( 107.3477315916820913, -15.88627780335592732, -1.500000000000000000 ) ) ;
#21508 = DIRECTION ( 'NONE',  ( 1.000000000000000000, -0.000000000000000000, -0.000000000000000000 ) ) ;
#21509 = VECTOR ( 'NONE', #20090, 1000.000000000000000 ) ;
#21510 = AXIS2_PLACEMENT_3D ( 'NONE', #22208, #9642, #4002 ) ;
#21511 = CARTESIAN_POINT ( 'NONE',  ( 2.425585535373192325, 9.314797388894900720, 5.239665997526921970 ) ) ;
#21512 = CARTESIAN_POINT ( 'NONE',  ( -2.112550801365593145, 1.088641768524161613, 3.675193018007247403 ) ) ;
#21513 = VERTEX_POINT ( 'NONE', #32441 ) ;
#21514 = AXIS2_PLACEMENT_3D ( 'NONE', #17431, #14901, #4896 ) ;
#21515 = CARTESIAN_POINT ( 'NONE',  ( -5.450050799999999640, -2.853674364686378695, -1.549418761218566809 ) ) ;
#21516 = LINE ( 'NONE', #31061, #25281 ) ;
#21517 = CARTESIAN_POINT ( 'NONE',  ( -4.912942406915327354, -5.022711880624455567E-15, 2.999999999999999556 ) ) ;
#21518 = CARTESIAN_POINT ( 'NONE',  ( 8.060276137098854932, -2.738905750061799704, 1.000000000000000000 ) ) ;
#21519 =( GEOMETRIC_REPRESENTATION_CONTEXT ( 3 ) GLOBAL_UNCERTAINTY_ASSIGNED_CONTEXT ( ( #27549 ) ) GLOBAL_UNIT_ASSIGNED_CONTEXT ( ( #10458, #28174, #13606 ) ) REPRESENTATION_CONTEXT ( 'NONE', 'WORKASPACE' ) );
#21520 = ORIENTED_EDGE ( 'NONE', *, *, #31411, .T. ) ;
#21521 = CARTESIAN_POINT ( 'NONE',  ( 10.28480887676876243, -12.81065604946471304, -1.500000000000000666 ) ) ;
#21522 = ADVANCED_FACE ( 'NONE', ( #29602 ), #11864, .T. ) ;
#21523 = B_SPLINE_CURVE_WITH_KNOTS ( 'NONE', 3,
 ( #19664, #31732, #32388, #21676, #3635, #22000, #19336, #32038, #19158, #19012, #29198, #1454, #9447, #23996, #29349, #22178, #11631, #9107, #31883, #29542, #6628, #21521, #27171, #9293, #14142, #16643, #16821, #29858, #19510, #1117, #27020, #6439 ),
 .UNSPECIFIED., .F., .F.,
 ( 4, 2, 2, 2, 2, 2, 2, 2, 2, 2, 2, 2, 2, 2, 2, 4 ),
 ( 8.673617379884035472E-19, 0.003232788846018234963, 0.004849183269027351577, 0.006465577692036469058, 0.008081972115045587407, 0.008890169326550144413, 0.009698366538054701419, 0.01050656374955926189, 0.01131476096106382237, 0.01293115538407293985, 0.01373935259557750033, 0.01454754980708205733, 0.01616394423009118522, 0.01939673307610943406, 0.02262952192212768984, 0.02586231076814594909 ),
 .UNSPECIFIED. ) ;
#21524 = ORIENTED_EDGE ( 'NONE', *, *, #551, .F. ) ;
#21525 = CARTESIAN_POINT ( 'NONE',  ( 0.2331433898338126642, -7.747061788033508201, 1.773832612458838609 ) ) ;
#21526 = ADVANCED_FACE ( 'NONE', ( #9175 ), #19063, .T. ) ;
#21527 = SECURITY_CLASSIFICATION_LEVEL ( 'unclassified' ) ;
#21528 = CARTESIAN_POINT ( 'NONE',  ( 84.96867291396014821, -4.109438037582242131, 4.074609222369775630 ) ) ;
#21529 = PLANE ( 'NONE',  #24030 ) ;
#21530 = CIRCLE ( 'NONE', #1775, 6.248999999999999666 ) ;
#21531 = CARTESIAN_POINT ( 'NONE',  ( 22.17497728449690086, -17.32537947343252682, -1.743178009048997001 ) ) ;
#21532 = DIRECTION ( 'NONE',  ( 0.000000000000000000, -0.5735764363510352792, -0.8191520442889993481 ) ) ;
#21533 =( BOUNDED_SURFACE ( )  B_SPLINE_SURFACE ( 1, 2, ( 
 ( #31605, #2898, #366, #16221, #23898, #3196, #693, #10884, #29101, #23407, #512, #32287, #29251, #12034, #9170, #6335, #32438, #1666, #9348, #29411, #17020, #14337, #11861, #19715, #16524, #26735, #4170, #24543, #19402, #27226, #22070, #19558, #29914, #3853, #14027, #29755, #6835, #29600, #21576, #6683, #16872, #4023, #21881, #16711, #4341, #24238, #27068, #1856, #26918, #6507, #1356, #14520, #24732, #22229, #9500, #16373, #11375, #26582, #3683, #31782, #13843, #24051, #32097, #1176, #11530, #8853, #9001, #19061, #14190, #21726, #31936, #19217, #24388, #1505, #11683, #17526, #32596, #27416, #17692, #25230, #19896 ),
 ( #20068, #17209, #23046, #4522, #22380, #12180, #30111, #30264, #32937, #30601, #14696, #12678, #15350, #10353, #7684, #22563, #9668, #14843, #22882, #168, #12526, #24895, #5020, #27906, #25555, #15198, #20564, #9856, #6997, #27573, #7187, #7335, #2160, #25042, #28075, #27720, #2007, #17380, #4673, #12829, #17882, #12344, #33084, #10162, #22733, #10007, #2660, #20383, #32778, #25400, #4828, #15009, #2351, #20217, #30413, #7491, #2510, #5172, #13174, #28575, #15849, #23864, #28225, #31258, #13501, #10508, #26405, #23532, #20720, #13661, #15994, #23715, #10661, #31086, #5981, #20872, #8176, #7843, #972, #18036, #13024 ) ),
 .UNSPECIFIED., .F., .F., .F. ) 
 B_SPLINE_SURFACE_WITH_KNOTS ( ( 2, 2 ),
 ( 3, 2, 2, 2, 2, 2, 2, 2, 2, 2, 2, 2, 2, 2, 2, 2, 2, 2, 2, 2, 2, 2, 2, 2, 2, 2, 2, 2, 2, 2, 2, 2, 2, 2, 2, 2, 2, 2, 2, 2, 3 ),
 ( 0.000000000000000000, 1.000000000000000000 ),
 ( 0.000000000000000000, 0.02500000000000000139, 0.05000000000000000278, 0.07499999999999999722, 0.1000000000000000056, 0.1250000000000000000, 0.1499999999999999944, 0.1749999999999999889, 0.2000000000000000111, 0.2250000000000000056, 0.2500000000000000000, 0.2750000000000000222, 0.2999999999999999889, 0.3250000000000000111, 0.3499999999999999778, 0.3750000000000000000, 0.4000000000000000222, 0.4249999999999999889, 0.4500000000000000111, 0.4749999999999999778, 0.5000000000000000000, 0.5250000000000000222, 0.5500000000000000444, 0.5749999999999999556, 0.5999999999999999778, 0.6250000000000000000, 0.6500000000000000222, 0.6750000000000000444, 0.6999999999999999556, 0.7249999999999999778, 0.7500000000000000000, 0.7750000000000000222, 0.8000000000000000444, 0.8249999999999999556, 0.8499999999999999778, 0.8750000000000000000, 0.9000000000000000222, 0.9250000000000000444, 0.9499999999999999556, 0.9749999999999999778, 1.000000000000000000 ),
 .UNSPECIFIED. ) 
 GEOMETRIC_REPRESENTATION_ITEM ( )  RATIONAL_B_SPLINE_SURFACE ( (
 ( 1.000000000000000000, 0.9238795325112867385, 1.000000000000000000, 0.9238795325112867385, 1.000000000000000000, 0.9238795325112867385, 1.000000000000000000, 0.9238795325112867385, 1.000000000000000000, 0.9238795325112867385, 1.000000000000000000, 0.9238795325112867385, 1.000000000000000000, 0.9238795325112867385, 1.000000000000000000, 0.9238795325112867385, 1.000000000000000000, 0.9238795325112867385, 1.000000000000000000, 0.9238795325112867385, 1.000000000000000000, 0.9238795325112867385, 1.000000000000000000, 0.9238795325112867385, 1.000000000000000000, 0.9238795325112867385, 1.000000000000000000, 0.9238795325112867385, 1.000000000000000000, 0.9238795325112867385, 1.000000000000000000, 0.9238795325112867385, 1.000000000000000000, 0.9238795325112867385, 1.000000000000000000, 0.9238795325112867385, 1.000000000000000000, 0.9238795325112867385, 1.000000000000000000, 0.9238795325112867385, 1.000000000000000000, 0.9238795325112867385, 1.000000000000000000, 0.9238795325112867385, 1.000000000000000000, 0.9238795325112867385, 1.000000000000000000, 0.9238795325112867385, 1.000000000000000000, 0.9238795325112867385, 1.000000000000000000, 0.9238795325112867385, 1.000000000000000000, 0.9238795325112867385, 1.000000000000000000, 0.9238795325112867385, 1.000000000000000000, 0.9238795325112867385, 1.000000000000000000, 0.9238795325112867385, 1.000000000000000000, 0.9238795325112867385, 1.000000000000000000, 0.9238795325112867385, 1.000000000000000000, 0.9238795325112867385, 1.000000000000000000, 0.9238795325112867385, 1.000000000000000000, 0.9238795325112867385, 1.000000000000000000, 0.9238795325112867385, 1.000000000000000000, 0.9238795325112867385, 1.000000000000000000, 0.9238795325112867385, 1.000000000000000000, 0.9238795325112867385, 1.000000000000000000, 0.9238795325112867385, 1.000000000000000000),
 ( 1.000000000000000000, 0.9238795325112867385, 1.000000000000000000, 0.9238795325112867385, 1.000000000000000000, 0.9238795325112867385, 1.000000000000000000, 0.9238795325112867385, 1.000000000000000000, 0.9238795325112867385, 1.000000000000000000, 0.9238795325112867385, 1.000000000000000000, 0.9238795325112867385, 1.000000000000000000, 0.9238795325112867385, 1.000000000000000000, 0.9238795325112867385, 1.000000000000000000, 0.9238795325112867385, 1.000000000000000000, 0.9238795325112867385, 1.000000000000000000, 0.9238795325112867385, 1.000000000000000000, 0.9238795325112867385, 1.000000000000000000, 0.9238795325112867385, 1.000000000000000000, 0.9238795325112867385, 1.000000000000000000, 0.9238795325112867385, 1.000000000000000000, 0.9238795325112867385, 1.000000000000000000, 0.9238795325112867385, 1.000000000000000000, 0.9238795325112867385, 1.000000000000000000, 0.9238795325112867385, 1.000000000000000000, 0.9238795325112867385, 1.000000000000000000, 0.9238795325112867385, 1.000000000000000000, 0.9238795325112867385, 1.000000000000000000, 0.9238795325112867385, 1.000000000000000000, 0.9238795325112867385, 1.000000000000000000, 0.9238795325112867385, 1.000000000000000000, 0.9238795325112867385, 1.000000000000000000, 0.9238795325112867385, 1.000000000000000000, 0.9238795325112867385, 1.000000000000000000, 0.9238795325112867385, 1.000000000000000000, 0.9238795325112867385, 1.000000000000000000, 0.9238795325112867385, 1.000000000000000000, 0.9238795325112867385, 1.000000000000000000, 0.9238795325112867385, 1.000000000000000000, 0.9238795325112867385, 1.000000000000000000, 0.9238795325112867385, 1.000000000000000000, 0.9238795325112867385, 1.000000000000000000, 0.9238795325112867385, 1.000000000000000000, 0.9238795325112867385, 1.000000000000000000, 0.9238795325112867385, 1.000000000000000000) ) ) 
 REPRESENTATION_ITEM ( '' )  SURFACE ( )  );
#21534 = VECTOR ( 'NONE', #991, 1000.000000000000114 ) ;
#21535 = EDGE_LOOP ( 'NONE', ( #30209, #22390, #28903 ) ) ;
#21536 = CIRCLE ( 'NONE', #7118, 0.5000000000000000000 ) ;
#21537 = CARTESIAN_POINT ( 'NONE',  ( 8.911384905465460804, 0.2172754300400931704, 1.412391582771745924 ) ) ;
#21538 = LINE ( 'NONE', #26059, #9146 ) ;
#21539 = AXIS2_PLACEMENT_3D ( 'NONE', #12698, #28096, #14866 ) ;
#21540 = CARTESIAN_POINT ( 'NONE',  ( 18.94410479637168621, -3.802018929891117338, -2.487845153640489748 ) ) ;
#21542 = ORIENTED_EDGE ( 'NONE', *, *, #8126, .T. ) ;
#21541 = DIRECTION ( 'NONE',  ( 0.000000000000000000, 0.000000000000000000, -1.000000000000000000 ) ) ;
#21543 = CARTESIAN_POINT ( 'NONE',  ( -2.112550801365593145, 1.088641768524161613, 3.675193018007247403 ) ) ;
#21544 = CARTESIAN_POINT ( 'NONE',  ( 108.2511986533483110, 19.57693314497984360, 2.802790312710702558 ) ) ;
#21545 = DIRECTION ( 'NONE',  ( 0.000000000000000000, 0.000000000000000000, -1.000000000000000000 ) ) ;
#21546 = LOCAL_TIME ( 16, 7, 10.00000000000000000, #31281 ) ;
#21547 = DIRECTION ( 'NONE',  ( -0.000000000000000000, -0.4226182617407035491, 0.9063077870366480493 ) ) ;
#21548 = CARTESIAN_POINT ( 'NONE',  ( 0.000000000000000000, 0.5000000000000000000, 0.000000000000000000 ) ) ;
#21549 = CARTESIAN_POINT ( 'NONE',  ( -34.48223484310472031, 0.5000000000000000000, 2.552009564962238297 ) ) ;
#21550 = CARTESIAN_POINT ( 'NONE',  ( 0.4398628304357217744, -12.95602692781729992, 5.485967528433935314 ) ) ;
#21551 = CARTESIAN_POINT ( 'NONE',  ( 0.000000000000000000, 0.000000000000000000, 0.000000000000000000 ) ) ;
#21552 = ORIENTED_EDGE ( 'NONE', *, *, #27516, .T. ) ;
#21553 = CARTESIAN_POINT ( 'NONE',  ( 25.36291098745260797, -17.54678857751243370, -1.252584024796136175 ) ) ;
#21554 = DIRECTION ( 'NONE',  ( 8.574039729943018344E-17, 1.000000000000000000, 0.000000000000000000 ) ) ;
#21555 = CARTESIAN_POINT ( 'NONE',  ( -4.037550801365593856, 3.675193018007246959, -1.088641768524161391 ) ) ;
#21556 = FACE_OUTER_BOUND ( 'NONE', #18797, .T. ) ;
#21557 = CARTESIAN_POINT ( 'NONE',  ( 41.35542541868176158, -7.892720653454384561, 2.184957211341423733 ) ) ;
#21558 = ORIENTED_EDGE ( 'NONE', *, *, #18117, .F. ) ;
#21559 = EDGE_CURVE ( 'NONE', #12555, #32100, #6685, .T. ) ;
#21560 = DIRECTION ( 'NONE',  ( 2.219124775574988582E-17, 0.2588190451025276784, -0.9659258262890664248 ) ) ;
#21561 = VECTOR ( 'NONE', #6058, 1000.000000000000000 ) ;
#21562 = ADVANCED_FACE ( 'NONE', ( #9502 ), #6837, .T. ) ;
#21563 = ORIENTED_EDGE ( 'NONE', *, *, #20179, .T. ) ;
#21564 = AXIS2_PLACEMENT_3D ( 'NONE', #13836, #5694, #13350 ) ;
#21565 = SECURITY_CLASSIFICATION_LEVEL ( 'unclassified' ) ;
#21567 = CARTESIAN_POINT ( 'NONE',  ( 85.03570040675890596, -5.202893351561465707, 3.995969900454463986 ) ) ;
#21566 = CC_DESIGN_APPROVAL ( #25149, ( #7706 ) ) ;
#21568 = CARTESIAN_POINT ( 'NONE',  ( -2.794738735352966685, 0.000000000000000000, -1.491740999229417941 ) ) ;
#21569 = VERTEX_POINT ( 'NONE', #22231 ) ;
#21570 = DIRECTION ( 'NONE',  ( -1.000000000000000000, -0.000000000000000000, -0.000000000000000000 ) ) ;
#21571 = ORIENTED_EDGE ( 'NONE', *, *, #24977, .T. ) ;
#21572 = ORIENTED_EDGE ( 'NONE', *, *, #11444, .T. ) ;
#21573 = MANIFOLD_SOLID_BREP ( 'Fillet6', #24296 ) ;
#21574 = CYLINDRICAL_SURFACE ( 'NONE', #7064, 4.000000000000001776 ) ;
#21575 = CARTESIAN_POINT ( 'NONE',  ( -5.212550801365593678, -1.828967928396026732, 3.368539882008728004 ) ) ;
#21576 = CARTESIAN_POINT ( 'NONE',  ( 23.86000000000000298, 1.573300977624590313, -1.942864903642426144 ) ) ;
#21577 = DIRECTION ( 'NONE',  ( 0.000000000000000000, 0.000000000000000000, -1.000000000000000000 ) ) ;
#21579 = ORIENTED_EDGE ( 'NONE', *, *, #32156, .F. ) ;
#21578 = CARTESIAN_POINT ( 'NONE',  ( 8.930755659325139817, 0.4999999999999980571, -1.500000000000000000 ) ) ;
#21580 = AXIS2_PLACEMENT_3D ( 'NONE', #32337, #14584, #4886 ) ;
#21581 = CARTESIAN_POINT ( 'NONE',  ( -7.687550801365593323, -2.752080473201636845, 2.228590825266444586 ) ) ;
#21582 = CARTESIAN_POINT ( 'NONE',  ( 19.82965097551559808, 15.28209255176019177, 1.499999999999766187 ) ) ;
#21583 = CARTESIAN_POINT ( 'NONE',  ( -32.99878091140236336, 0.000000000000000000, -0.9987809114023521451 ) ) ;
#21584 = CARTESIAN_POINT ( 'NONE',  ( -23.54713438637982748, 13.83847758521832993, 10.84763956049549805 ) ) ;
#21586 = VERTEX_POINT ( 'NONE', #19717 ) ;
#21585 = CARTESIAN_POINT ( 'NONE',  ( 23.00820037127764550, -17.39482224626776130, 1.688990564600256761 ) ) ;
#21587 = CARTESIAN_POINT ( 'NONE',  ( 22.17250000273118715, 2.378061970571979433, -1.291182301015470824 ) ) ;
#21588 = SECURITY_CLASSIFICATION ( '', '', #19831 ) ;
#21589 = CARTESIAN_POINT ( 'NONE',  ( -22.61376412419543414, 3.520075575297991755, 1.500000000000000000 ) ) ;
#21590 = CARTESIAN_POINT ( 'NONE',  ( 2.274274201625327230, -4.762163868918204201, -9.915734732513268312 ) ) ;
#21591 = CARTESIAN_POINT ( 'NONE',  ( -4.161545776608246427, -8.294432461897566000, -1.500000000000000000 ) ) ;
#21592 = EDGE_CURVE ( 'NONE', #30798, #23666, #17070, .T. ) ;
#21593 = CARTESIAN_POINT ( 'NONE',  ( 11.04311965146451158, 15.00000000000000178, 1.500000000000000000 ) ) ;
#21594 = CARTESIAN_POINT ( 'NONE',  ( 10.55147673363118876, 2.376879293651121383, -4.116875700062057497 ) ) ;
#21595 = DIRECTION ( 'NONE',  ( 1.000000000000000000, -0.000000000000000000, -0.000000000000000000 ) ) ;
#21596 = ORIENTED_EDGE ( 'NONE', *, *, #1343, .T. ) ;
#21597 = AXIS2_PLACEMENT_3D ( 'NONE', #2128, #32745, #25525 ) ;
#21598 = DIRECTION ( 'NONE',  ( 1.000000000000000000, 0.000000000000000000, 0.000000000000000000 ) ) ;
#21599 = ADVANCED_FACE ( 'NONE', ( #6510 ), #16713, .F. ) ;
#21600 = CARTESIAN_POINT ( 'NONE',  ( 18.68265047573912341, -6.724553502642427461, 4.522129901861162260 ) ) ;
#21602 = DIRECTION ( 'NONE',  ( 1.000000000000000000, -0.000000000000000000, 8.654346879536960414E-15 ) ) ;
#21601 = DIRECTION ( 'NONE',  ( 0.000000000000000000, 1.000000000000000000, 0.000000000000000000 ) ) ;
#21603 = ORIENTED_EDGE ( 'NONE', *, *, #23394, .T. ) ;
#21604 = CARTESIAN_POINT ( 'NONE',  ( 3.499999999999999556, -2.861184399890954300, -6.440778198864141935 ) ) ;
#21605 = ORIENTED_EDGE ( 'NONE', *, *, #22410, .T. ) ;
#21606 = CARTESIAN_POINT ( 'NONE',  ( -7.712942406915323623, 7.727249047114547632E-16, -2.999999999999999556 ) ) ;
#21608 = ORIENTED_EDGE ( 'NONE', *, *, #9768, .T. ) ;
#21607 = CARTESIAN_POINT ( 'NONE',  ( 28.69349675861934301, -5.619750657913020753, -3.999773682874202319 ) ) ;
#21609 = EDGE_CURVE ( 'NONE', #23825, #21273, #11745, .T. ) ;
#21610 = ORIENTED_EDGE ( 'NONE', *, *, #24060, .F. ) ;
#21611 = CARTESIAN_POINT ( 'NONE',  ( -8.000050800000000351, 3.400452463515772461, -1.145969202744355542 ) ) ;
#21612 = CARTESIAN_POINT ( 'NONE',  ( -6.100050802731187716, 1.549418761218566143, -2.853674364686379583 ) ) ;
#21614 = VERTEX_POINT ( 'NONE', #27909 ) ;
#21613 = CARTESIAN_POINT ( 'NONE',  ( -3.192834903017093051, -11.75164088162766873, -1.500000000000000222 ) ) ;
#21615 = CARTESIAN_POINT ( 'NONE',  ( 11.67104222929842372, 3.952383228471274990, -1.050000000000000044 ) ) ;
#21616 = CARTESIAN_POINT ( 'NONE',  ( -2.373172266667121555, -12.30297787492008688, -1.743844711840834449 ) ) ;
#21617 = EDGE_CURVE ( 'NONE', #11109, #12129, #12540, .T. ) ;
#21618 = CYLINDRICAL_SURFACE ( 'NONE', #31583, 2.999999999999999112 ) ;
#21619 = CARTESIAN_POINT ( 'NONE',  ( 7.931701156346584014, -9.929036423919631815, -1.500000000000359934 ) ) ;
#21620 = CARTESIAN_POINT ( 'NONE',  ( 107.9107100874947349, -16.78360958907837031, -2.272491201332555555 ) ) ;
#21621 = CARTESIAN_POINT ( 'NONE',  ( 6.356382228872879736, 3.475951004017332924, 7.873648075250509137 ) ) ;
#21622 = VECTOR ( 'NONE', #14746, 1000.000000000000000 ) ;
#21623 = ADVANCED_FACE ( 'NONE', ( #17694 ), #13984, .T. ) ;
#21624 = DIRECTION ( 'NONE',  ( -1.000000000000000000, 0.000000000000000000, 0.000000000000000000 ) ) ;
#21625 = CARTESIAN_POINT ( 'NONE',  ( -3.250050800000000795, -1.549418761218565255, 2.853674364686380471 ) ) ;
#21626 = CARTESIAN_POINT ( 'NONE',  ( 9.999999999999998224, -4.681538312723523276, 0.8254815157535098091 ) ) ;
#21627 = ORIENTED_EDGE ( 'NONE', *, *, #921, .T. ) ;
#21628 = DIRECTION ( 'NONE',  ( 1.000000000000000000, -0.000000000000000000, -0.000000000000000000 ) ) ;
#21629 = EDGE_CURVE ( 'NONE', #24805, #17980, #14945, .T. ) ;
#21630 = DIRECTION ( 'NONE',  ( 0.000000000000000000, 0.000000000000000000, 1.000000000000000000 ) ) ;
#21631 = ADVANCED_FACE ( 'NONE', ( #23232 ), #5517, .T. ) ;
#21632 = LINE ( 'NONE', #26978, #9783 ) ;
#21633 = ORIENTED_EDGE ( 'NONE', *, *, #27110, .T. ) ;
#21634 = DIRECTION ( 'NONE',  ( 0.000000000000000000, 0.000000000000000000, -1.000000000000000000 ) ) ;
#21635 = CARTESIAN_POINT ( 'NONE',  ( 3.063284526839888944, 8.152713396088756781, 3.174628368996099681 ) ) ;
#21636 = ORIENTED_EDGE ( 'NONE', *, *, #30110, .F. ) ;
#21637 = DIRECTION ( 'NONE',  ( -0.9164966213036979115, 0.4000424266736042900, 0.000000000000000000 ) ) ;
#21638 = VERTEX_POINT ( 'NONE', #3331 ) ;
#21639 = B_SPLINE_CURVE_WITH_KNOTS ( 'NONE', 3,
 ( #5696, #13691, #18903, #11035, #16216, #1169 ),
 .UNSPECIFIED., .F., .F.,
 ( 4, 2, 4 ),
 ( 6.133173666733496745E-19, 0.0003885750149250817857, 0.0007771500298501630294 ),
 .UNSPECIFIED. ) ;
#21640 = ORIENTED_EDGE ( 'NONE', *, *, #29137, .F. ) ;
#21641 = CARTESIAN_POINT ( 'NONE',  ( 24.61821134308479841, -17.47399247671392430, -1.556972331815056121 ) ) ;
#21642 = PERSON_AND_ORGANIZATION_ROLE ( 'classification_officer' ) ;
#21644 = ORIENTED_EDGE ( 'NONE', *, *, #12424, .T. ) ;
#21643 = CARTESIAN_POINT ( 'NONE',  ( 3.249999999999999556, -8.264486777890139635, 4.472189673936756371 ) ) ;
#21645 = ORIENTED_EDGE ( 'NONE', *, *, #14208, .T. ) ;
#21646 = DIRECTION ( 'NONE',  ( -0.000000000000000000, -0.000000000000000000, -1.000000000000000000 ) ) ;
#21647 = EDGE_CURVE ( 'NONE', #23090, #29226, #18679, .T. ) ;
#21648 = ORIENTED_EDGE ( 'NONE', *, *, #27368, .F. ) ;
#21649 = DIRECTION ( 'NONE',  ( 0.000000000000000000, 1.000000000000000000, 0.000000000000000000 ) ) ;
#21650 = FACE_OUTER_BOUND ( 'NONE', #2455, .T. ) ;
#21652 = ORIENTED_EDGE ( 'NONE', *, *, #19652, .T. ) ;
#21651 = CARTESIAN_POINT ( 'NONE',  ( 29.34042402277824735, -3.698761498129651493, -0.07017451553337591963 ) ) ;
#21653 = DIRECTION ( 'NONE',  ( 2.219124775575017240E-17, 0.2588190451025310646, -0.9659258262890655367 ) ) ;
#21654 = DIRECTION ( 'NONE',  ( 1.000000000000000000, -0.000000000000000000, -0.000000000000000000 ) ) ;
#21655 = CARTESIAN_POINT ( 'NONE',  ( 101.9216173105994301, -5.769792427975440674, 0.4426577266272666566 ) ) ;
#21656 = CARTESIAN_POINT ( 'NONE',  ( 3.063284526839887167, 4.729683950898978750, -7.360373001730866171 ) ) ;
#21657 = CARTESIAN_POINT ( 'NONE',  ( 108.0610369550560250, -18.94827908534190897, 4.525375360948980408 ) ) ;
#21658 = CARTESIAN_POINT ( 'NONE',  ( -1.671916146696470262, -10.12145986844939394, -5.485967528433938867 ) ) ;
#21659 = DIRECTION ( 'NONE',  ( 0.000000000000000000, 0.000000000000000000, 1.000000000000000000 ) ) ;
#21660 = CARTESIAN_POINT ( 'NONE',  ( 5.865515302491333571, 15.00000000000002132, -1.491740999229417941 ) ) ;
#21661 = EDGE_CURVE ( 'NONE', #9818, #18033, #3507, .T. ) ;
#21662 = LINE ( 'NONE', #31531, #31576 ) ;
#21663 = CARTESIAN_POINT ( 'NONE',  ( 2.330754651808344910E-16, 2.718385644597233863, -4.208382051008164204 ) ) ;
#21664 = LINE ( 'NONE', #17076, #16673 ) ;
#21665 = FACE_OUTER_BOUND ( 'NONE', #2697, .T. ) ;
#21666 = ADVANCED_FACE ( 'NONE', ( #25727 ), #20319, .T. ) ;
#21667 = CARTESIAN_POINT ( 'NONE',  ( 108.0849250792287961, 18.65105627586314085, 4.618623753023407552 ) ) ;
#21668 = EDGE_CURVE ( 'NONE', #3071, #16406, #13027, .T. ) ;
#21669 = CARTESIAN_POINT ( 'NONE',  ( -5.100050802731186828, 2.853674364686379583, 1.549418761218565921 ) ) ;
#21670 = ORIENTED_EDGE ( 'NONE', *, *, #12216, .T. ) ;
#21671 = CARTESIAN_POINT ( 'NONE',  ( -6.900050800000000706, 0.3135853898029611342, -2.983565686104819648 ) ) ;
#21672 = CARTESIAN_POINT ( 'NONE',  ( 3.249999999999999556, 1.699438267350371179, 9.241976615262162298 ) ) ;
#21673 = DIRECTION ( 'NONE',  ( 0.1908089953765452484, 0.000000000000000000, 0.9816271834476638647 ) ) ;
#21674 = CARTESIAN_POINT ( 'NONE',  ( 7.168700581566836760, -6.410142746917610879, 1.500000000000000222 ) ) ;
#21675 = EDGE_LOOP ( 'NONE', ( #20698, #11442, #19409 ) ) ;
#21676 = CARTESIAN_POINT ( 'NONE',  ( 7.106060642427864948, -3.992384276486344863, -1.499999999999999778 ) ) ;
#21677 = ORIENTED_EDGE ( 'NONE', *, *, #23131, .T. ) ;
#21678 = CARTESIAN_POINT ( 'NONE',  ( 0.3845462673029811929, -5.169103183424899939, 1.499999999999964695 ) ) ;
#21679 = PERSON_AND_ORGANIZATION_ROLE ( 'design_supplier' ) ;
#21680 = EDGE_LOOP ( 'NONE', ( #11759, #1494, #24624, #17403 ) ) ;
#21681 = CARTESIAN_POINT ( 'NONE',  ( 84.97936832875919322, -4.283865861999379021, 4.215289907553382953 ) ) ;
#21682 = EDGE_CURVE ( 'NONE', #15401, #4392, #32501, .T. ) ;
#21683 = CC_DESIGN_PERSON_AND_ORGANIZATION_ASSIGNMENT ( #1997, #16696, ( #26353 ) ) ;
#21684 = CARTESIAN_POINT ( 'NONE',  ( 18.88504792851585279, 14.44361348414706647, -1.050000000000000266 ) ) ;
#21685 = CARTESIAN_POINT ( 'NONE',  ( 84.97018126096170931, -4.134036538230700053, -4.093303008782878116 ) ) ;
#21686 = CARTESIAN_POINT ( 'NONE',  ( 21.59695500783953293, -17.14749606024714979, -1.524646196215473593 ) ) ;
#21687 = CARTESIAN_POINT ( 'NONE',  ( 15.55254023221933046, 20.42149909151570597, 5.412820279296878923 ) ) ;
#21688 = EDGE_LOOP ( 'NONE', ( #21677, #24013, #16928, #27318 ) ) ;
#21689 = CARTESIAN_POINT ( 'NONE',  ( 23.19969962673269492, -21.93395824423269147, -1.123858796072322974 ) ) ;
#21690 = DIRECTION ( 'NONE',  ( 0.000000000000000000, 0.000000000000000000, 1.000000000000000000 ) ) ;
#21691 = CARTESIAN_POINT ( 'NONE',  ( -2.794738735352966685, 0.000000000000000000, -1.000000000000000000 ) ) ;
#21693 = ORIENTED_EDGE ( 'NONE', *, *, #23075, .F. ) ;
#21692 = DIRECTION ( 'NONE',  ( 0.000000000000000000, 0.2588190451025172423, 0.9659258262890692004 ) ) ;
#21694 = CARTESIAN_POINT ( 'NONE',  ( -3.112550801365593145, 3.675193018007247403, -1.088641768524161391 ) ) ;
#21695 = DIRECTION ( 'NONE',  ( 1.000000000000000000, 0.000000000000000000, 0.000000000000000000 ) ) ;
#21696 = DIRECTION ( 'NONE',  ( 0.000000000000000000, -0.4226182617407066022, 0.9063077870366466060 ) ) ;
#21697 = CARTESIAN_POINT ( 'NONE',  ( 108.6181628074316450, 15.96285980845909158, 2.043459238665831013 ) ) ;
#21698 = DIRECTION ( 'NONE',  ( 1.000000000000000000, -0.000000000000000000, -0.000000000000000000 ) ) ;
#21699 = EDGE_CURVE ( 'NONE', #22155, #10298, #13703, .T. ) ;
#21700 = CARTESIAN_POINT ( 'NONE',  ( -29.34654203815345141, 5.521763387534528889, 1.291504468647948212 ) ) ;
#21701 = DIRECTION ( 'NONE',  ( -1.000000000000000000, 0.000000000000000000, 0.000000000000000000 ) ) ;
#21702 = FACE_OUTER_BOUND ( 'NONE', #24139, .T. ) ;
#21703 = CARTESIAN_POINT ( 'NONE',  ( -0.5616989984783476997, -12.44624546261724518, 4.522129901861159595 ) ) ;
#21704 = VERTEX_POINT ( 'NONE', #5333 ) ;
#21705 = LINE ( 'NONE', #17359, #164 ) ;
#21706 = VERTEX_POINT ( 'NONE', #20873 ) ;
#21707 = DIRECTION ( 'NONE',  ( -1.000000000000000000, 8.574039729943022041E-17, -3.081487911019577365E-33 ) ) ;
#21708 = CARTESIAN_POINT ( 'NONE',  ( -1.913028242501583209, 0.5824277790515788311, 3.167204378891976813 ) ) ;
#21709 = CARTESIAN_POINT ( 'NONE',  ( -3.837550801365593234, 1.088641768524161613, 3.675193018007246959 ) ) ;
#21710 = CARTESIAN_POINT ( 'NONE',  ( 25.75999999999999446, 2.338214438728005273, 1.985154692390100006 ) ) ;
#21711 = CARTESIAN_POINT ( 'NONE',  ( 0.6728001243833413580, -4.913284922779170394, -7.719803900032154331 ) ) ;
#21712 = EDGE_LOOP ( 'NONE', ( #28531, #13837, #31967, #607 ) ) ;
#21713 = DIRECTION ( 'NONE',  ( -1.000000000000000000, -0.000000000000000000, 0.000000000000000000 ) ) ;
#21714 =( BOUNDED_SURFACE ( )  B_SPLINE_SURFACE ( 3, 2, ( 
 ( #21845, #17164, #16991 ),
 ( #29565, #27374, #4489 ),
 ( #14663, #6650, #25078 ),
 ( #19935, #2536, #28249 ),
 ( #30142, #20420, #5199 ),
 ( #4861, #7218, #32965 ),
 ( #25581, #18060, #15225 ),
 ( #15044, #4707, #30800 ),
 ( #25265, #27604, #12379 ),
 ( #14876, #22600, #22757 ),
 ( #7868, #10034, #9883 ),
 ( #25760, #32812, #2382 ),
 ( #20098, #5359, #30447 ),
 ( #2693, #2192, #12554 ) ),
 .UNSPECIFIED., .F., .F., .F. ) 
 B_SPLINE_SURFACE_WITH_KNOTS ( ( 4, 2, 2, 2, 2, 2, 4 ),
 ( 3, 3 ),
 ( 8.673617379884035472E-19, 0.0002022161777894803118, 0.0003033242666842200612, 0.0004044323555789597563, 0.0005055404444736994515, 0.0006066485333684392550, 0.0008088647111579186453 ),
 ( 0.000000000000000000, 1.000000000000000000 ),
 .UNSPECIFIED. ) 
 GEOMETRIC_REPRESENTATION_ITEM ( )  RATIONAL_B_SPLINE_SURFACE ( (
 ( 1.000000000000000000, 0.7044453589051213882, 1.000000000000000000),
 ( 1.000000000000000000, 0.7046023864747805732, 1.000000000000000000),
 ( 1.000000000000000000, 0.7048235607688740911, 1.000000000000000000),
 ( 1.000000000000000000, 0.7054263556248401290, 1.000000000000000000),
 ( 1.000000000000000000, 0.7056784645812754775, 1.000000000000000000),
 ( 1.000000000000000000, 0.7063102947743578053, 1.000000000000000000),
 ( 1.000000000000000000, 0.7067030625551506962, 1.000000000000000000),
 ( 1.000000000000000000, 0.7074976564992083716, 1.000000000000000000),
 ( 1.000000000000000000, 0.7078925116172140042, 1.000000000000000000),
 ( 1.000000000000000000, 0.7085287470472093618, 1.000000000000000000),
 ( 1.000000000000000000, 0.7087824354666338866, 1.000000000000000000),
 ( 1.000000000000000000, 0.7093860731733975244, 1.000000000000000000),
 ( 1.000000000000000000, 0.7096079946502726887, 1.000000000000000000),
 ( 1.000000000000000000, 0.7097644798780707864, 1.000000000000000000) ) ) 
 REPRESENTATION_ITEM ( '' )  SURFACE ( )  );
#21715 = EDGE_LOOP ( 'NONE', ( #32574, #31505, #8078 ) ) ;
#21716 = PERSON_AND_ORGANIZATION ( #6766, #25292 ) ;
#21717 = FACE_OUTER_BOUND ( 'NONE', #9665, .T. ) ;
#21718 = EDGE_CURVE ( 'NONE', #21723, #7241, #4973, .T. ) ;
#21719 = CARTESIAN_POINT ( 'NONE',  ( 8.250826798929582040, -2.275785942832204256, -1.000000000000000000 ) ) ;
#21720 = ORIENTED_EDGE ( 'NONE', *, *, #29930, .T. ) ;
#21721 = DIRECTION ( 'NONE',  ( 0.000000000000000000, 0.000000000000000000, -1.000000000000000000 ) ) ;
#21722 = ORIENTED_EDGE ( 'NONE', *, *, #19203, .F. ) ;
#21723 = VERTEX_POINT ( 'NONE', #7998 ) ;
#21724 = CARTESIAN_POINT ( 'NONE',  ( 24.35999999999999943, -1.573300977624594976, 1.942864903642425700 ) ) ;
#21725 = DIRECTION ( 'NONE',  ( 1.000000000000000000, -0.000000000000000000, -0.000000000000000000 ) ) ;
#21726 = CARTESIAN_POINT ( 'NONE',  ( 21.92250000000000298, 2.378061970571979433, -1.291182301015470824 ) ) ;
#21727 = CARTESIAN_POINT ( 'NONE',  ( 0.6277548181752619083, -4.204133288872636598, -1.499999999999860778 ) ) ;
#21729 = VERTEX_POINT ( 'NONE', #649 ) ;
#21728 = CARTESIAN_POINT ( 'NONE',  ( 5.612718761614564400, 3.934162523501332220, -7.212912035758772156 ) ) ;
#21730 = CARTESIAN_POINT ( 'NONE',  ( -7.737550801365593145, -1.828967928396026510, 3.368539882008728004 ) ) ;
#21731 = CARTESIAN_POINT ( 'NONE',  ( 107.8265048288121051, 17.21207035378186845, -2.248242208486546989 ) ) ;
#21732 = CARTESIAN_POINT ( 'NONE',  ( 5.489321486716458587, 1.512021494499692809, -7.976795196726671477 ) ) ;
#21733 = LINE ( 'NONE', #29922, #7593 ) ;
#21734 = EDGE_LOOP ( 'NONE', ( #21358, #6145, #7723, #13604 ) ) ;
#21735 = ADVANCED_FACE ( 'NONE', ( #10844 ), #28722, .T. ) ;
#21737 = ORIENTED_EDGE ( 'NONE', *, *, #32426, .F. ) ;
#21736 = CARTESIAN_POINT ( 'NONE',  ( 21.03177542174608661, -17.18603084754167298, 1.753176640694531274 ) ) ;
#21738 = EDGE_CURVE ( 'NONE', #29013, #5075, #1626, .T. ) ;
#21739 = FACE_OUTER_BOUND ( 'NONE', #20286, .T. ) ;
#21740 = ADVANCED_FACE ( 'NONE', ( #14159 ), #5353, .T. ) ;
#21741 = CARTESIAN_POINT ( 'NONE',  ( 23.04750000273119070, 0.7685399846772009713, -2.594547506269381909 ) ) ;
#21742 = CARTESIAN_POINT ( 'NONE',  ( 7.249760686538667009, -0.8180878109961253752, -8.711672189281435053 ) ) ;
#21743 = CARTESIAN_POINT ( 'NONE',  ( -30.49072021767876706, 13.22775097665176958, 1.500000000000000000 ) ) ;
#21744 = FACE_OUTER_BOUND ( 'NONE', #5523, .T. ) ;
#21745 = CARTESIAN_POINT ( 'NONE',  ( 56.97280603064898941, -277.2763395528616002, 1.508259000770581615 ) ) ;
#21746 = B_SPLINE_SURFACE_WITH_KNOTS ( 'NONE', 3, 3, ( 
 ( #27826, #27510, #4943, #7606, #15288, #30026, #12122, #17620, #22318, #15125 ),
 ( #32531, #32873, #25490, #88, #2448, #4454, #25336, #28014, #4609, #30351 ),
 ( #12616, #5110, #20003, #20498, #30712, #2598, #17462, #14786, #24984, #7115 ),
 ( #22817, #9594, #22969, #4765, #14939, #30200, #17316, #10278, #2094, #33022 ) ),
 .UNSPECIFIED., .F., .F., .F.,
 ( 4, 4 ),
 ( 4, 3, 3, 4 ),
 ( 1.412182049029299374E-10, 1.000000000000000000 ),
 ( 0.009544196576262833909, 0.5047720982881089835, 0.7523860491440320653, 0.9999999999999551470 ),
 .UNSPECIFIED. ) ;
#21747 = CARTESIAN_POINT ( 'NONE',  ( 9.282537329959909655, 0.2172754300399125094, 1.041239158277188048 ) ) ;
#21748 = CARTESIAN_POINT ( 'NONE',  ( -3.287550801365593856, 2.752080473201636845, -2.228590825266444142 ) ) ;
#21749 = DIRECTION ( 'NONE',  ( 0.000000000000000000, 0.000000000000000000, 1.000000000000000000 ) ) ;
#21750 = EDGE_LOOP ( 'NONE', ( #25939, #11987, #12634, #9616 ) ) ;
#21751 = CARTESIAN_POINT ( 'NONE',  ( 10.57125986779756843, 1.115095498423374076, -4.884328206559825247 ) ) ;
#21752 = CARTESIAN_POINT ( 'NONE',  ( 25.86240141410256044, 23.76612641949138549, -0.4463807625373443777 ) ) ;
#21754 = CARTESIAN_POINT ( 'NONE',  ( 22.17354848663391920, -17.00157258782028080, 1.495009212619065497 ) ) ;
#21753 = CARTESIAN_POINT ( 'NONE',  ( 6.037141812302425414, -1.911013226338353688, -8.256172215043598328 ) ) ;
#21755 = ORIENTED_EDGE ( 'NONE', *, *, #18926, .F. ) ;
#21756 = CARTESIAN_POINT ( 'NONE',  ( 3.063284526839887167, 0.000000000000000000, 0.000000000000000000 ) ) ;
#21757 = ORIENTED_EDGE ( 'NONE', *, *, #6689, .F. ) ;
#21758 = CARTESIAN_POINT ( 'NONE',  ( 21.32535692059145660, -21.82495604402121003, -1.318256435726663955 ) ) ;
#21760 = ORIENTED_EDGE ( 'NONE', *, *, #3062, .F. ) ;
#21759 = CARTESIAN_POINT ( 'NONE',  ( 40.87773863319960554, -5.749898180376480816, -3.995336175111656285 ) ) ;
#21761 = ORIENTED_EDGE ( 'NONE', *, *, #12942, .T. ) ;
#21762 = CARTESIAN_POINT ( 'NONE',  ( -6.162942409646512409, 7.727249047114547632E-16, -2.999999999999999556 ) ) ;
#21763 = EDGE_CURVE ( 'NONE', #14980, #21865, #10153, .T. ) ;
#21765 = ORIENTED_EDGE ( 'NONE', *, *, #17786, .T. ) ;
#21764 = CARTESIAN_POINT ( 'NONE',  ( -0.6222083319099647181, -14.83248753350331306, -1.499999999999999334 ) ) ;
#21766 = CARTESIAN_POINT ( 'NONE',  ( 9.548498637265968370, 1.402184917482039994, -1.500000000000000000 ) ) ;
#21767 = DIRECTION ( 'NONE',  ( 0.000000000000000000, 0.000000000000000000, -1.000000000000000000 ) ) ;
#21768 = CARTESIAN_POINT ( 'NONE',  ( 108.0331448824852032, -18.54664017899650830, -4.208585127045829211 ) ) ;
#21769 = CARTESIAN_POINT ( 'NONE',  ( 10.11068945975151756, -12.10067465534980080, -1.000000000000000000 ) ) ;
#21771 = EDGE_LOOP ( 'NONE', ( #23026, #499, #32922, #968 ) ) ;
#21770 = CARTESIAN_POINT ( 'NONE',  ( 107.9600896886990853, -17.49466356266586686, -4.826758019528888610 ) ) ;
#21772 = FACE_OUTER_BOUND ( 'NONE', #12092, .T. ) ;
#21773 = CARTESIAN_POINT ( 'NONE',  ( -12.44989959798873791, 19.51744974835124680, -2.318435636271050537 ) ) ;
#21774 = FACE_OUTER_BOUND ( 'NONE', #29779, .T. ) ;
#21775 = B_SPLINE_CURVE_WITH_KNOTS ( 'NONE', 3,
 ( #887, #13090, #7902, #723, #23432, #13565 ),
 .UNSPECIFIED., .F., .F.,
 ( 4, 2, 4 ),
 ( 0.009527197497156560113, 0.5047635987485782350, 1.000000000000000000 ),
 .UNSPECIFIED. ) ;
#21776 = DIRECTION ( 'NONE',  ( 0.000000000000000000, 0.03489949670250105246, -0.9993908270190957621 ) ) ;
#21777 = CARTESIAN_POINT ( 'NONE',  ( 29.25343337322282622, -7.426690278353109242, -4.522129901861164036 ) ) ;
#21778 =( BOUNDED_CURVE ( )  B_SPLINE_CURVE ( 2, ( #20108, #17564, #22608, #4715, #25594, #217, #2703, #30810, #7878, #28112, #5370 ),
 .UNSPECIFIED., .F., .F. ) 
 B_SPLINE_CURVE_WITH_KNOTS ( ( 3, 2, 2, 2, 2, 3 ),
 ( 0.5966116191895003418, 0.5999999999999999778, 0.6250000000000000000, 0.6500000000000000222, 0.6750000000000000444, 0.6966116191895003196 ),
 .UNSPECIFIED. ) 
 CURVE ( )  GEOMETRIC_REPRESENTATION_ITEM ( )  RATIONAL_B_SPLINE_CURVE ( ( 0.9821626249036858880, 0.9896829947469992783, 1.000000000000000000, 0.9238795325112867385, 1.000000000000000000, 0.9238795325112867385, 1.000000000000000000, 0.9238795325112867385, 1.000000000000000000, 0.9341965377642874602, 0.9821626249036858880 ) ) 
 REPRESENTATION_ITEM ( '' )  );
#21779 = EDGE_LOOP ( 'NONE', ( #31900, #7050, #28909 ) ) ;
#21780 = CARTESIAN_POINT ( 'NONE',  ( 0.3749743548324803166, 0.8908839545096812751, 10.05686762493600384 ) ) ;
#21781 = CYLINDRICAL_SURFACE ( 'NONE', #20964, 8.500000000000000000 ) ;
#21782 = DIRECTION ( 'NONE',  ( 0.000000000000000000, 0.000000000000000000, -1.000000000000000000 ) ) ;
#21783 = ORIENTED_EDGE ( 'NONE', *, *, #30760, .F. ) ;
#21784 = CARTESIAN_POINT ( 'NONE',  ( 2.864531314636029613, -6.140839842381227598, 7.330015575757884427 ) ) ;
#21785 = CARTESIAN_POINT ( 'NONE',  ( 6.749760686538667009, 0.000000000000000000, 5.500000000000000000 ) ) ;
#21786 = ORIENTED_EDGE ( 'NONE', *, *, #15336, .F. ) ;
#21787 = CARTESIAN_POINT ( 'NONE',  ( 3.858046770353062982, -11.79229388856150784, -1.499999999999999556 ) ) ;
#21788 = ADVANCED_FACE ( 'NONE', ( #19357 ), #21843, .F. ) ;
#21789 = ORIENTED_EDGE ( 'NONE', *, *, #16232, .F. ) ;
#21790 = B_SPLINE_CURVE_WITH_KNOTS ( 'NONE', 3,
 ( #3023, #15707, #20391, #17699, #17533, #27913, #22739, #5338 ),
 .UNSPECIFIED., .F., .F.,
 ( 4, 2, 2, 4 ),
 ( 0.0001261938424379285015, 0.0002444035063406801295, 0.0003626131702434317846, 0.0005990324980489345526 ),
 .UNSPECIFIED. ) ;
#21791 = EDGE_LOOP ( 'NONE', ( #4316, #29288, #24812, #3754 ) ) ;
#21792 = CARTESIAN_POINT ( 'NONE',  ( 25.48003164478615190, -17.55790041459374962, -1.000000000000000444 ) ) ;
#21793 = EDGE_CURVE ( 'NONE', #31825, #7812, #27188, .T. ) ;
#21795 = EDGE_LOOP ( 'NONE', ( #747, #27071, #27754, #24149, #1808 ) ) ;
#21794 = CARTESIAN_POINT ( 'NONE',  ( 21.04494988260864474, -21.68420912488519647, -1.499840339240438469 ) ) ;
#21796 = ORIENTED_EDGE ( 'NONE', *, *, #8031, .T. ) ;
#21797 = CARTESIAN_POINT ( 'NONE',  ( 22.79750000136559862, 0.3178988483021036315, 3.024605502323848949 ) ) ;
#21798 = ORIENTED_EDGE ( 'NONE', *, *, #24873, .T. ) ;
#21799 = DIRECTION ( 'NONE',  ( 1.735780866781622650E-15, -0.000000000000000000, -1.000000000000000000 ) ) ;
#21800 = CARTESIAN_POINT ( 'NONE',  ( 0.000000000000000000, 0.000000000000000000, 0.000000000000000000 ) ) ;
#21802 = ORIENTED_EDGE ( 'NONE', *, *, #13688, .T. ) ;
#21801 = CARTESIAN_POINT ( 'NONE',  ( 10.57125986779756843, 0.8254815157535864145, -4.681538312723508177 ) ) ;
#21803 = CARTESIAN_POINT ( 'NONE',  ( 101.6441386174529384, -1.774168274679073454, -2.184956718804114573 ) ) ;
#21804 = CARTESIAN_POINT ( 'NONE',  ( 6.356381935169119757, 0.9265622495396906855, -8.556754636093199196 ) ) ;
#21805 = EDGE_CURVE ( 'NONE', #20282, #29098, #1073, .T. ) ;
#21806 = DIRECTION ( 'NONE',  ( 0.1908089953765452762, 0.000000000000000000, 0.9816271834476639757 ) ) ;
#21807 = EDGE_CURVE ( 'NONE', #8819, #16362, #21897, .T. ) ;
#21808 = CARTESIAN_POINT ( 'NONE',  ( 6.883866621640341243, 5.066432324612723193, 7.111352071735041136 ) ) ;
#21809 = CARTESIAN_POINT ( 'NONE',  ( 107.5624059028085497, -18.99272140073565751, 4.497205547310911378 ) ) ;
#21810 = DIRECTION ( 'NONE',  ( -1.000000000000000000, 0.000000000000000000, 0.000000000000000000 ) ) ;
#21811 = DIRECTION ( 'NONE',  ( 0.000000000000000000, 0.000000000000000000, 1.000000000000000000 ) ) ;
#21812 = LINE ( 'NONE', #18996, #20017 ) ;
#21813 = EDGE_CURVE ( 'NONE', #5237, #16550, #29717, .T. ) ;
#21814 = DIRECTION ( 'NONE',  ( -1.387778780781444413E-14, -1.000000000000000000, 0.000000000000000000 ) ) ;
#21815 = DIRECTION ( 'NONE',  ( 0.000000000000000000, 0.000000000000000000, 1.000000000000000000 ) ) ;
#21816 = DIRECTION ( 'NONE',  ( -1.000000000000000000, 0.000000000000000000, -8.654346879536960414E-15 ) ) ;
#21817 = CARTESIAN_POINT ( 'NONE',  ( 108.0731628266868540, 18.58555941254615007, 4.648189127559274603 ) ) ;
#21818 = CARTESIAN_POINT ( 'NONE',  ( -7.250050802731188071, -2.331437884370912705, 1.887961173149512062 ) ) ;
#21819 = VERTEX_POINT ( 'NONE', #24504 ) ;
#21820 = ADVANCED_FACE ( 'NONE', ( #1816 ), #9129, .T. ) ;
#21821 = CARTESIAN_POINT ( 'NONE',  ( -5.900050800000000706, 2.983565686104819648, 0.3135853898029609677 ) ) ;
#21822 = FACE_OUTER_BOUND ( 'NONE', #15102, .T. ) ;
#21823 = DIRECTION ( 'NONE',  ( 0.000000000000000000, -0.8660254037844432595, 0.4999999999999918954 ) ) ;
#21824 = CARTESIAN_POINT ( 'NONE',  ( 4.749760686538667009, -1.391664247347281780, 7.892520144992429820 ) ) ;
#21825 = ORIENTED_EDGE ( 'NONE', *, *, #9172, .F. ) ;
#21826 = DIRECTION ( 'NONE',  ( 1.000000000000000000, 0.000000000000000000, 0.000000000000000000 ) ) ;
#21827 = B_SPLINE_CURVE_WITH_KNOTS ( 'NONE', 3,
 ( #29864, #14957, #4129, #29548, #2292, #19835, #9802, #11803, #22011, #20024, #12293, #14458, #14295, #25171, #9615, #12478, #16826, #27359, #32234, #22505, #22184, #19516, #1801, #9300, #7138, #22690, #11988, #6946, #9116, #19345, #17147, #4475 ),
 .UNSPECIFIED., .F., .F.,
 ( 4, 2, 2, 2, 2, 2, 2, 2, 2, 2, 2, 2, 2, 2, 2, 4 ),
 ( 0.000000000000000000, 0.004377979416501958515, 0.008755958833003917030, 0.01313393824950587208, 0.01751191766600783059, 0.01860641252013331415, 0.01970090737425880464, 0.02188989708250978217, 0.02298439193663526572, 0.02407888679076075275, 0.02517338164488623631, 0.02626787649901171987, 0.02845686620726269739, 0.02955136106138818441, 0.03064585591551366797, 0.03502383533201561261 ),
 .UNSPECIFIED. ) ;
#21828 = ORIENTED_EDGE ( 'NONE', *, *, #26592, .F. ) ;
#21829 = CARTESIAN_POINT ( 'NONE',  ( 0.1143091695231461258, -6.518402738280636655, 1.773884761005948274 ) ) ;
#21830 = PERSON_AND_ORGANIZATION ( #6766, #25292 ) ;
#21831 = CARTESIAN_POINT ( 'NONE',  ( 6.880159329304571081, 6.122988934091276647, 6.224287131858821986 ) ) ;
#21832 = ORIENTED_EDGE ( 'NONE', *, *, #24301, .T. ) ;
#21833 = CARTESIAN_POINT ( 'NONE',  ( 69.04806619053955785, -5.668245219738529350, 4.312042181580753031 ) ) ;
#21834 = CARTESIAN_POINT ( 'NONE',  ( 24.14622570346762842, 18.13272393406391814, -1.049999999999999822 ) ) ;
#21835 = LINE ( 'NONE', #29361, #5407 ) ;
#21836 = CARTESIAN_POINT ( 'NONE',  ( -5.749676575031998027, 0.000000000000000000, 0.000000000000000000 ) ) ;
#21837 = ORIENTED_EDGE ( 'NONE', *, *, #27272, .T. ) ;
#21838 = ADVANCED_FACE ( 'NONE', ( #14306 ), #22024, .F. ) ;
#21839 = CARTESIAN_POINT ( 'NONE',  ( 9.065183082710460027, 0.01785380481418138293, 1.195037335522169730 ) ) ;
#21840 = ADVANCED_FACE ( 'NONE', ( #16664 ), #26549, .F. ) ;
#21841 = CARTESIAN_POINT ( 'NONE',  ( 107.7310687598602215, 16.68064466458321959, 1.424544220713904963 ) ) ;
#21842 = DIRECTION ( 'NONE',  ( -1.000000000000000000, 0.000000000000000000, 0.000000000000000000 ) ) ;
#21844 = ORIENTED_EDGE ( 'NONE', *, *, #21018, .F. ) ;
#21843 = PLANE ( 'NONE',  #27774 ) ;
#21845 = CARTESIAN_POINT ( 'NONE',  ( 108.1156589233280272, 18.82219444680286458, -4.397958565568440115 ) ) ;
#21846 = CARTESIAN_POINT ( 'NONE',  ( -31.67864539881508179, -21.93013659627822776, 1.095404497688272194 ) ) ;
#21847 = CARTESIAN_POINT ( 'NONE',  ( -4.562942409646513653, -3.366872799099910998E-15, -3.000000000000000000 ) ) ;
#21848 = DIRECTION ( 'NONE',  ( -1.000000000000000000, 0.000000000000000000, 0.000000000000000000 ) ) ;
#21849 = CARTESIAN_POINT ( 'NONE',  ( 2.857987970441405956, -8.861329655858749987, 3.588272043363009534 ) ) ;
#21850 = ADVANCED_FACE ( 'NONE', ( #13806 ), #13980, .F. ) ;
#21851 = CARTESIAN_POINT ( 'NONE',  ( -31.67864539881508179, -21.93013659627822776, 1.095404497688272194 ) ) ;
#21852 = DIRECTION ( 'NONE',  ( 1.000000000000000000, -0.000000000000000000, -0.000000000000000000 ) ) ;
#21853 = DIRECTION ( 'NONE',  ( 0.000000000000000000, 0.000000000000000000, -1.000000000000000000 ) ) ;
#21854 = VECTOR ( 'NONE', #4092, 1000.000000000000000 ) ;
#21855 = VERTEX_POINT ( 'NONE', #31899 ) ;
#21856 = CARTESIAN_POINT ( 'NONE',  ( 5.612974259723589654, 2.621729824970383760, 7.786824029658776070 ) ) ;
#21857 = EDGE_LOOP ( 'NONE', ( #25165, #25135, #1641 ) ) ;
#21858 = ADVANCED_FACE ( 'NONE', ( #14661 ), #27538, .T. ) ;
#21859 = CARTESIAN_POINT ( 'NONE',  ( 3.499999999999999556, 5.904264776415098837, 2.046865518294726183 ) ) ;
#21860 = VECTOR ( 'NONE', #21495, 1000.000000000000227 ) ;
#21861 = DIRECTION ( 'NONE',  ( -0.000000000000000000, -1.000000000000000000, -0.000000000000000000 ) ) ;
#21862 = FACE_OUTER_BOUND ( 'NONE', #16370, .T. ) ;
#21863 = CARTESIAN_POINT ( 'NONE',  ( 33.81874022276149105, 19.51744974835125035, 2.318435636271284128 ) ) ;
#21864 = CARTESIAN_POINT ( 'NONE',  ( 29.19739603783667548, -7.896110766392163249, 1.873788768274956995 ) ) ;
#21865 = VERTEX_POINT ( 'NONE', #412 ) ;
#21866 = CARTESIAN_POINT ( 'NONE',  ( -59.39818691134999540, -5.278984095179490410, 5.312697832964588862 ) ) ;
#21867 = VECTOR ( 'NONE', #15657, 1000.000000000000000 ) ;
#21868 = ORIENTED_EDGE ( 'NONE', *, *, #9385, .T. ) ;
#21869 = COORDINATED_UNIVERSAL_TIME_OFFSET ( 0, 0, .AHEAD. ) ;
#21870 = CARTESIAN_POINT ( 'NONE',  ( 102.4231535280176217, -3.997791915949104435, 3.996604656711563397 ) ) ;
#21871 = EDGE_CURVE ( 'NONE', #19072, #20419, #14405, .T. ) ;
#21872 = AXIS2_PLACEMENT_3D ( 'NONE', #22327, #32539, #22498 ) ;
#21873 = CARTESIAN_POINT ( 'NONE',  ( 8.013022481854630286, -2.861148639377020686, -1.000000000000000000 ) ) ;
#21874 = CIRCLE ( 'NONE', #19763, 4.000000000000002665 ) ;
#21875 = DIRECTION ( 'NONE',  ( 0.000000000000000000, 0.9510565162951523099, 0.3090169943749516701 ) ) ;
#21876 = ORIENTED_EDGE ( 'NONE', *, *, #18777, .F. ) ;
#21877 = ORIENTED_EDGE ( 'NONE', *, *, #30395, .T. ) ;
#21878 = EDGE_CURVE ( 'NONE', #15946, #18549, #17966, .T. ) ;
#21879 = CARTESIAN_POINT ( 'NONE',  ( 24.30656763371926132, -0.8852964313267484009, 2.499999999999997780 ) ) ;
#21880 = DIRECTION ( 'NONE',  ( 0.000000000000000000, 0.9659258262890660918, 0.2588190451025291772 ) ) ;
#21881 = CARTESIAN_POINT ( 'NONE',  ( 23.61000000000000298, -1.942864903642428587, -1.573300977624592756 ) ) ;
#21882 = CARTESIAN_POINT ( 'NONE',  ( 7.168280658702385288, -13.96541762984794310, -1.755547115761689314 ) ) ;
#21883 = AXIS2_PLACEMENT_3D ( 'NONE', #24784, #32644, #27279 ) ;
#21885 = ORIENTED_EDGE ( 'NONE', *, *, #9978, .T. ) ;
#21884 = CARTESIAN_POINT ( 'NONE',  ( 0.000000000000000000, 0.000000000000000000, 0.000000000000000000 ) ) ;
#21886 = CARTESIAN_POINT ( 'NONE',  ( -3.137550801365593500, 3.368539882008727115, 1.828967928396026954 ) ) ;
#21887 = CARTESIAN_POINT ( 'NONE',  ( 10.56870887191539587, -1.476463073999605857, -4.787500056513382063 ) ) ;
#21888 = CARTESIAN_POINT ( 'NONE',  ( -57.84278510284880781, -3.116935358302278747, 5.499999999999997335 ) ) ;
#21889 = LINE ( 'NONE', #21584, #742 ) ;
#21890 = VERTEX_POINT ( 'NONE', #13110 ) ;
#21892 = ORIENTED_EDGE ( 'NONE', *, *, #24442, .F. ) ;
#21891 = DIRECTION ( 'NONE',  ( -0.4999999999999952816, -0.8660254037844413721, -0.000000000000000000 ) ) ;
#21893 = CARTESIAN_POINT ( 'NONE',  ( -6.700050800000000528, 2.983565686104819648, 0.3135853898029609677 ) ) ;
#21894 = CARTESIAN_POINT ( 'NONE',  ( 20.67250000273118715, -2.378061970571983430, 1.291182301015471712 ) ) ;
#21895 = AXIS2_PLACEMENT_3D ( 'NONE', #3157, #21200, #31397 ) ;
#21896 = CARTESIAN_POINT ( 'NONE',  ( -23.54713438637984169, 18.90773822806172433, 1.500000000000000000 ) ) ;
#21898 = ADVANCED_FACE ( 'NONE', ( #9465 ), #25830, .T. ) ;
#21897 = CIRCLE ( 'NONE', #24561, 2.999999999999999112 ) ;
#21899 = LINE ( 'NONE', #27084, #3307 ) ;
#21900 = CARTESIAN_POINT ( 'NONE',  ( -23.35000000000000142, -10.96966150227469505, -1.499999999999999556 ) ) ;
#21901 = CARTESIAN_POINT ( 'NONE',  ( 1.750000000000000222, -2.417132211460010005, -8.149077976821821778 ) ) ;
#21902 = VECTOR ( 'NONE', #26133, 1000.000000000000000 ) ;
#21903 = CARTESIAN_POINT ( 'NONE',  ( 84.85832005755366936, -2.331047133796893434, 0.4367664088711343817 ) ) ;
#21904 = CARTESIAN_POINT ( 'NONE',  ( -3.637550801365593944, -3.675193018007246071, 1.088641768524163167 ) ) ;
#21905 = ORIENTED_EDGE ( 'NONE', *, *, #5165, .T. ) ;
#21906 = DIRECTION ( 'NONE',  ( 0.000000000000000000, 0.000000000000000000, 1.000000000000000000 ) ) ;
#21907 = VERTEX_POINT ( 'NONE', #32405 ) ;
#21908 = VECTOR ( 'NONE', #32742, 1000.000000000000114 ) ;
#21909 = PLANE ( 'NONE',  #4401 ) ;
#21910 = CARTESIAN_POINT ( 'NONE',  ( 48.01729800609908949, -4.703650321870251894, -4.522129901861162260 ) ) ;
#21912 = LINE ( 'NONE', #1699, #25701 ) ;
#21911 = CARTESIAN_POINT ( 'NONE',  ( 7.064423600674403225, 2.210816291637418551, 8.466096581344331184 ) ) ;
#21913 = VERTEX_POINT ( 'NONE', #24857 ) ;
#21914 = EDGE_CURVE ( 'NONE', #21819, #14956, #4296, .T. ) ;
#21915 = DIRECTION ( 'NONE',  ( -1.000000000000000000, 0.000000000000000000, 0.000000000000000000 ) ) ;
#21916 = PERSON ( 'NAUO-PER7', 'UNSPECIFIED', 'UNSPECIFIED', ('UNSPECIFIED'), ('UNSPECIFIED'), ('UNSPECIFIED') ) ;
#21917 = ORIENTED_EDGE ( 'NONE', *, *, #4476, .F. ) ;
#21918 = DIRECTION ( 'NONE',  ( 1.000000000000000000, 0.000000000000000000, 0.000000000000000000 ) ) ;
#21919 = EDGE_CURVE ( 'NONE', #11908, #32312, #4635, .T. ) ;
#21921 = VERTEX_POINT ( 'NONE', #28154 ) ;
#21920 = CARTESIAN_POINT ( 'NONE',  ( 84.96563828038404154, -4.059947112070683595, -3.995005841611614095 ) ) ;
#21922 = AXIS2_PLACEMENT_3D ( 'NONE', #5025, #30418, #27579 ) ;
#21923 = EDGE_LOOP ( 'NONE', ( #2146, #20707, #18932, #26028, #33040, #4546, #27424, #29941, #24452, #12074, #17596, #16577 ) ) ;
#21924 = CARTESIAN_POINT ( 'NONE',  ( 7.064632951172269415, 6.147671362329299782, -6.226446564517853943 ) ) ;
#21925 = VECTOR ( 'NONE', #561, 1000.000000000000114 ) ;
#21926 = CYLINDRICAL_SURFACE ( 'NONE', #21463, 4.999999999999997335 ) ;
#21928 = EDGE_LOOP ( 'NONE', ( #27984, #20511 ) ) ;
#21927 = CARTESIAN_POINT ( 'NONE',  ( -3.135269660805078740, -0.5000000000000000000, -1.500000000000000000 ) ) ;
#21929 = PLANE ( 'NONE',  #32199 ) ;
#21930 = VECTOR ( 'NONE', #22843, 1000.000000000000227 ) ;
#21931 = DIRECTION ( 'NONE',  ( -1.000000000000000000, 0.000000000000000000, 0.000000000000000000 ) ) ;
#21932 = CARTESIAN_POINT ( 'NONE',  ( 7.249760686538667009, 0.000000000000000000, 0.000000000000000000 ) ) ;
#21933 = CARTESIAN_POINT ( 'NONE',  ( 12.08436850396365259, -13.77779907615468247, -1.500000000000000000 ) ) ;
#21935 = ORIENTED_EDGE ( 'NONE', *, *, #5897, .T. ) ;
#21934 = CARTESIAN_POINT ( 'NONE',  ( 108.0402073727359351, -18.64833828181508224, -4.957871595061241088 ) ) ;
#21936 = CARTESIAN_POINT ( 'NONE',  ( 2.795120667416425508, -7.433119754668519263, 6.320583870820093431 ) ) ;
#21937 = CIRCLE ( 'NONE', #28879, 0.5000000000000008882 ) ;
#21938 = CARTESIAN_POINT ( 'NONE',  ( 2.589202905186834158, 4.126870756446594513, -9.453729690310105127 ) ) ;
#21939 = DIRECTION ( 'NONE',  ( 0.000000000000000000, 1.000000000000000000, 0.000000000000000000 ) ) ;
#21940 = DIRECTION ( 'NONE',  ( 0.000000000000000000, -0.9993908270190956511, 0.03489949670250104552 ) ) ;
#21941 = CARTESIAN_POINT ( 'NONE',  ( 0.7212198416532934475, -5.676697589997725224, 6.922088825881682617 ) ) ;
#21942 = ORIENTED_EDGE ( 'NONE', *, *, #25966, .F. ) ;
#21943 = CARTESIAN_POINT ( 'NONE',  ( 0.000000000000000000, 0.000000000000000000, 0.000000000000000000 ) ) ;
#21944 = CIRCLE ( 'NONE', #12320, 0.5000000000000004441 ) ;
#21945 = DIRECTION ( 'NONE',  ( 7.472768010110316618E-18, 0.08715574274764853469, 0.9961946980917464334 ) ) ;
#21946 = FACE_OUTER_BOUND ( 'NONE', #24795, .T. ) ;
#21947 = ORIENTED_EDGE ( 'NONE', *, *, #22054, .T. ) ;
#21948 = AXIS2_PLACEMENT_3D ( 'NONE', #11335, #3814, #21545 ) ;
#21949 = CIRCLE ( 'NONE', #31068, 303.6457063863959434 ) ;
#21950 = CARTESIAN_POINT ( 'NONE',  ( -8.000050800000009232, 1.732502019020233597, -3.080952105985496292 ) ) ;
#21951 = CARTESIAN_POINT ( 'NONE',  ( -5.304000690461529555E-12, -21.43932300456189566, -1.000000000000000000 ) ) ;
#21952 = VERTEX_POINT ( 'NONE', #19681 ) ;
#21953 = DIRECTION ( 'NONE',  ( 0.04710975479914575326, 0.5265925107009691297, -0.8488115212910426477 ) ) ;
#21954 = EDGE_CURVE ( 'NONE', #3611, #18559, #10590, .T. ) ;
#21955 = ORIENTED_EDGE ( 'NONE', *, *, #12704, .F. ) ;
#21956 = EDGE_CURVE ( 'NONE', #19600, #4093, #11207, .T. ) ;
#21957 = CIRCLE ( 'NONE', #7550, 8.749000000000002331 ) ;
#21958 = EDGE_LOOP ( 'NONE', ( #25494, #23583, #22592, #32187 ) ) ;
#21959 = DIRECTION ( 'NONE',  ( 4.917867153432958970E-17, 0.5735764363510412744, 0.8191520442889951292 ) ) ;
#21960 = DATE_AND_TIME ( #11757, #23758 ) ;
#21962 = ORIENTED_EDGE ( 'NONE', *, *, #31416, .F. ) ;
#21961 = CARTESIAN_POINT ( 'NONE',  ( -46.10000000000000142, -10.96966150227468972, 7.500000000000000000 ) ) ;
#21963 = ORIENTED_EDGE ( 'NONE', *, *, #30021, .T. ) ;
#21964 = CARTESIAN_POINT ( 'NONE',  ( 20.92250000136559507, -1.913930629741527500, 2.363507492473149618 ) ) ;
#21965 = ORIENTED_EDGE ( 'NONE', *, *, #6188, .F. ) ;
#21966 = CARTESIAN_POINT ( 'NONE',  ( 10.57125986779756843, 4.681538312723516171, 0.8254815157535410064 ) ) ;
#21967 = CARTESIAN_POINT ( 'NONE',  ( 0.3045634635874763796, 2.226307684702712120, -10.03290811084087508 ) ) ;
#21969 = ORIENTED_EDGE ( 'NONE', *, *, #11171, .F. ) ;
#21968 = CARTESIAN_POINT ( 'NONE',  ( -5.304000690461529555E-12, -21.43932300456189566, -1.500000000000000000 ) ) ;
#21970 = LINE ( 'NONE', #9892, #6011 ) ;
#21971 = CARTESIAN_POINT ( 'NONE',  ( -1.750050802731187405, -0.3135853898029607456, 2.983565686104819648 ) ) ;
#21972 = AXIS2_PLACEMENT_3D ( 'NONE', #1730, #1555, #32341 ) ;
#21973 = CARTESIAN_POINT ( 'NONE',  ( -29.65619690862280677, -27.93932300454937590, 11.50000000000000000 ) ) ;
#21974 = LINE ( 'NONE', #11612, #29028 ) ;
#21975 = VECTOR ( 'NONE', #24436, 1000.000000000000000 ) ;
#21976 =( BOUNDED_CURVE ( )  B_SPLINE_CURVE ( 3, ( #20522, #22994, #12483, #33042 ),
 .UNSPECIFIED., .F., .F. ) 
 B_SPLINE_CURVE_WITH_KNOTS ( ( 4, 4 ),
 ( 3.159180468610128578, 3.757378358066267854 ),
 .UNSPECIFIED. ) 
 CURVE ( )  GEOMETRIC_REPRESENTATION_ITEM ( )  RATIONAL_B_SPLINE_CURVE ( ( 1.000000000000000000, 0.9704015875404256031, 0.9704015875404256031, 1.000000000000000000 ) ) 
 REPRESENTATION_ITEM ( '' )  );
#21977 = CIRCLE ( 'NONE', #17731, 2.999999999999998668 ) ;
#21978 = CARTESIAN_POINT ( 'NONE',  ( -1.293118168543757385, -1.473601950426213447, -5.485967528433938867 ) ) ;
#21979 = CARTESIAN_POINT ( 'NONE',  ( 10.56183597391177464, 0.2500000000000523470, -5.003758587302145955 ) ) ;
#21980 = CARTESIAN_POINT ( 'NONE',  ( 7.437041877750292684, 18.60036511249582958, -1.491740999229418385 ) ) ;
#21981 = VECTOR ( 'NONE', #15512, 1000.000000000000000 ) ;
#21982 = AXIS2_PLACEMENT_3D ( 'NONE', #7399, #10071, #2930 ) ;
#21983 = AXIS2_PLACEMENT_3D ( 'NONE', #5507, #2846, #20716 ) ;
#21984 = CARTESIAN_POINT ( 'NONE',  ( 0.000000000000000000, 0.000000000000000000, 0.000000000000000000 ) ) ;
#21985 = DIRECTION ( 'NONE',  ( 0.000000000000000000, 0.000000000000000000, -1.000000000000000000 ) ) ;
#21986 = DIRECTION ( 'NONE',  ( 0.000000000000000000, -1.000000000000000000, 0.000000000000000000 ) ) ;
#21987 = CARTESIAN_POINT ( 'NONE',  ( 3.063284526843245370, -8.152713396074034335, 3.174628368989241611 ) ) ;
#21988 = CARTESIAN_POINT ( 'NONE',  ( -5.700050802731187360, -1.549418761218565477, 2.853674364686380471 ) ) ;
#21989 = VERTEX_POINT ( 'NONE', #15786 ) ;
#21990 = CARTESIAN_POINT ( 'NONE',  ( -4.200050800000000528, 1.887961173149511618, 2.331437884370912705 ) ) ;
#21991 = EDGE_CURVE ( 'NONE', #866, #25870, #23155, .T. ) ;
#21992 = TOROIDAL_SURFACE ( 'NONE', #7589, 6.818740222761507042, 0.5000000000000000000 ) ;
#21993 = AXIS2_PLACEMENT_3D ( 'NONE', #29152, #11095, #3587 ) ;
#21994 = DIRECTION ( 'NONE',  ( 1.000000000000000000, 0.000000000000000000, 0.000000000000000000 ) ) ;
#21995 = CARTESIAN_POINT ( 'NONE',  ( 17.75999999999999801, -2.208672634433321348E-15, -2.499999999999996891 ) ) ;
#21996 = CARTESIAN_POINT ( 'NONE',  ( 6.694810660865657681, -7.699995848972423396, 1.500000000000000000 ) ) ;
#21998 = ORIENTED_EDGE ( 'NONE', *, *, #16922, .T. ) ;
#21997 = VECTOR ( 'NONE', #26742, 1000.000000000000114 ) ;
#21999 = CARTESIAN_POINT ( 'NONE',  ( -1.950050802731187138, 2.983565686104819648, 0.3135853898029609677 ) ) ;
#22000 = CARTESIAN_POINT ( 'NONE',  ( 6.751043368244978637, -5.560327249377557735, -1.500000000000000000 ) ) ;
#22001 = EDGE_CURVE ( 'NONE', #23179, #1670, #3098, .T. ) ;
#22002 = AXIS2_PLACEMENT_3D ( 'NONE', #18122, #18783, #10761 ) ;
#22003 = VECTOR ( 'NONE', #6041, 1000.000000000000114 ) ;
#22004 = AXIS2_PLACEMENT_3D ( 'NONE', #2668, #31092, #2357 ) ;
#22005 = VERTEX_POINT ( 'NONE', #268 ) ;
#22006 = CARTESIAN_POINT ( 'NONE',  ( 0.7768566917565598029, -9.232541975952356594, 1.768685230608914694 ) ) ;
#22007 = COORDINATED_UNIVERSAL_TIME_OFFSET ( 0, 0, .AHEAD. ) ;
#22009 = ADVANCED_FACE ( 'NONE', ( #14812 ), #2951, .F. ) ;
#22008 = DIRECTION ( 'NONE',  ( 0.000000000000000000, 0.000000000000000000, 1.000000000000000000 ) ) ;
#22010 = VERTEX_POINT ( 'NONE', #7924 ) ;
#22011 = CARTESIAN_POINT ( 'NONE',  ( 2.040190332798762274, -16.78709061960636006, 1.500000000000000444 ) ) ;
#22012 = AXIS2_PLACEMENT_3D ( 'NONE', #9487, #21560, #19046 ) ;
#22013 = CIRCLE ( 'NONE', #32176, 8.750000000000000000 ) ;
#22014 = B_SPLINE_CURVE_WITH_KNOTS ( 'NONE', 3,
 ( #25517, #9970, #4974, #2625 ),
 .UNSPECIFIED., .F., .F.,
 ( 4, 4 ),
 ( 0.01682050255744390113, 0.01682075285862147038 ),
 .UNSPECIFIED. ) ;
#22015 = CARTESIAN_POINT ( 'NONE',  ( -5.712942406915326288, 3.284080845023683730E-15, 3.000000000000000000 ) ) ;
#22016 = CARTESIAN_POINT ( 'NONE',  ( 54.97099024851991800, -6.281314660059669208, -4.215290387854291332 ) ) ;
#22017 = CARTESIAN_POINT ( 'NONE',  ( 23.88966202700583707, -17.43474874481648484, -1.573876621503120576 ) ) ;
#22018 = DIRECTION ( 'NONE',  ( 0.000000000000000000, 0.8191520442889873577, 0.5735764363510524877 ) ) ;
#22019 = ORIENTED_EDGE ( 'NONE', *, *, #11165, .F. ) ;
#22020 = EDGE_CURVE ( 'NONE', #926, #7472, #2756, .T. ) ;
#22021 = CARTESIAN_POINT ( 'NONE',  ( 23.09498300328091247, -21.93193249238094822, -1.086362660086072296 ) ) ;
#22022 = CARTESIAN_POINT ( 'NONE',  ( 2.357330042320751939, -5.240837896778892890, -9.485534025193874896 ) ) ;
#22023 = AXIS2_PLACEMENT_3D ( 'NONE', #30738, #15160, #2121 ) ;
#22025 = VERTEX_POINT ( 'NONE', #17162 ) ;
#22024 = CYLINDRICAL_SURFACE ( 'NONE', #32588, 3.750000000000000444 ) ;
#22026 = CIRCLE ( 'NONE', #16666, 10.46966150227469150 ) ;
#22027 = CARTESIAN_POINT ( 'NONE',  ( 2.274274201621893976, 10.90201369671108722, -1.464956435144929570 ) ) ;
#22028 = PRODUCT ( 'Part8_handle2Sleeve', 'Part8_handle2Sleeve', '', ( #22551 ) ) ;
#22029 = TOROIDAL_SURFACE ( 'NONE', #162, 301.4345239564033250, 4.999999999999999112 ) ;
#22030 = LINE ( 'NONE', #11651, #45 ) ;
#22031 = DIRECTION ( 'NONE',  ( 1.000000000000000000, 0.000000000000000000, -0.000000000000000000 ) ) ;
#22032 = ADVANCED_FACE ( 'NONE', ( #4487 ), #1975, .T. ) ;
#22033 = CARTESIAN_POINT ( 'NONE',  ( 10.56870887191539587, 1.625881193364757449, -4.467071865485455540 ) ) ;
#22034 = DIRECTION ( 'NONE',  ( 1.000000000000000000, 0.000000000000000000, 0.000000000000000000 ) ) ;
#22035 = AXIS2_PLACEMENT_3D ( 'NONE', #8050, #2405, #5575 ) ;
#22036 = AXIS2_PLACEMENT_3D ( 'NONE', #31345, #13262, #11093 ) ;
#22037 = LINE ( 'NONE', #30075, #25221 ) ;
#22038 = CARTESIAN_POINT ( 'NONE',  ( 6.883866621640341243, -6.224335161394975557, -6.123537914202305643 ) ) ;
#22039 = DIRECTION ( 'NONE',  ( 0.000000000000000000, 0.000000000000000000, -1.000000000000000000 ) ) ;
#22040 = CARTESIAN_POINT ( 'NONE',  ( -25.11562363250528662, 4.199264901004248429, 2.140598393455739767 ) ) ;
#22041 = ORIENTED_EDGE ( 'NONE', *, *, #7785, .F. ) ;
#22042 = EDGE_CURVE ( 'NONE', #23417, #18225, #29027, .T. ) ;
#22043 = CARTESIAN_POINT ( 'NONE',  ( -2.962942409646513564, 4.884725290497410777E-15, -2.999999999999999556 ) ) ;
#22044 = ORIENTED_EDGE ( 'NONE', *, *, #11401, .T. ) ;
#22045 = VECTOR ( 'NONE', #21721, 1000.000000000000000 ) ;
#22046 = CARTESIAN_POINT ( 'NONE',  ( 10.00000000000000000, -1.625881193364669297, -4.467071865485488402 ) ) ;
#22047 = CARTESIAN_POINT ( 'NONE',  ( 108.9971408137216287, 18.07315888506168733, 5.421472300029551050 ) ) ;
#22048 = DIRECTION ( 'NONE',  ( -1.000000000000000000, 8.574039729943019576E-17, 1.232595164407830946E-32 ) ) ;
#22049 = EDGE_CURVE ( 'NONE', #29154, #3757, #13253, .T. ) ;
#22050 = CARTESIAN_POINT ( 'NONE',  ( 25.75999999999999446, 1.024942698525265428, 2.863353032229740691 ) ) ;
#22051 = CARTESIAN_POINT ( 'NONE',  ( 23.64680669414060787, -7.447390197411329460, 2.184956778807267241 ) ) ;
#22052 = ORIENTED_EDGE ( 'NONE', *, *, #4662, .T. ) ;
#22053 = FACE_OUTER_BOUND ( 'NONE', #15494, .T. ) ;
#22054 = EDGE_CURVE ( 'NONE', #30035, #572, #20127, .T. ) ;
#22055 = VECTOR ( 'NONE', #15961, 1000.000000000000000 ) ;
#22056 = ORIENTED_EDGE ( 'NONE', *, *, #19522, .T. ) ;
#22057 = PERSON_AND_ORGANIZATION_ROLE ( 'design_supplier' ) ;
#22058 = CARTESIAN_POINT ( 'NONE',  ( 28.66452313916941108, -6.748747283354279425, 4.018750267705075707 ) ) ;
#22059 = CIRCLE ( 'NONE', #14547, 0.4499999999999990119 ) ;
#22060 = EDGE_CURVE ( 'NONE', #2638, #13159, #16041, .T. ) ;
#22061 = AXIS2_PLACEMENT_3D ( 'NONE', #21745, #6051, #29119 ) ;
#22062 = DIRECTION ( 'NONE',  ( -1.000000000000000000, 0.000000000000000000, 0.000000000000000000 ) ) ;
#22063 = LINE ( 'NONE', #14185, #3375 ) ;
#22065 = ORIENTED_EDGE ( 'NONE', *, *, #29364, .F. ) ;
#22064 = VECTOR ( 'NONE', #11650, 1000.000000000000000 ) ;
#22066 = EDGE_LOOP ( 'NONE', ( #23352, #23746, #27838, #14077 ) ) ;
#22067 = AXIS2_PLACEMENT_3D ( 'NONE', #16431, #17551, #2885 ) ;
#22068 = CYLINDRICAL_SURFACE ( 'NONE', #2842, 5.010000000000000675 ) ;
#22069 = DIRECTION ( 'NONE',  ( 0.000000000000000000, 0.000000000000000000, 1.000000000000000000 ) ) ;
#22070 = CARTESIAN_POINT ( 'NONE',  ( 24.35999999999999943, -1.573300977624594976, 1.942864903642425700 ) ) ;
#22071 = EDGE_CURVE ( 'NONE', #28865, #28172, #25120, .T. ) ;
#22072 = CARTESIAN_POINT ( 'NONE',  ( 1.873231708749834912, -10.12253852703719126, -1.500000000000000000 ) ) ;
#22074 = ORIENTED_EDGE ( 'NONE', *, *, #15446, .F. ) ;
#22073 = CARTESIAN_POINT ( 'NONE',  ( 5.377543748152549874, 4.007137495034909236, -6.940565734314555257 ) ) ;
#22075 = CARTESIAN_POINT ( 'NONE',  ( -7.762550801365593500, 2.228590825266444142, 2.752080473201636845 ) ) ;
#22076 = PLANE ( 'NONE',  #11772 ) ;
#22077 = CARTESIAN_POINT ( 'NONE',  ( 24.25111450864415730, -3.256483526998273983E-15, 2.499999999999998668 ) ) ;
#22078 = CARTESIAN_POINT ( 'NONE',  ( -15.12340757463330654, -21.43932300455815465, -1.500000000000000000 ) ) ;
#22079 = ORIENTED_EDGE ( 'NONE', *, *, #28473, .F. ) ;
#22081 = EDGE_LOOP ( 'NONE', ( #17102, #15856, #24006, #7961 ) ) ;
#22080 = CARTESIAN_POINT ( 'NONE',  ( 2.482257818914018532, 0.000000000000000000, 1.712210361609934672 ) ) ;
#22082 = AXIS2_PLACEMENT_3D ( 'NONE', #27653, #27325, #1768 ) ;
#22083 = CARTESIAN_POINT ( 'NONE',  ( 14.29722302835932624, 9.309426707029093251, 1.500000000000000222 ) ) ;
#22084 = AXIS2_PLACEMENT_3D ( 'NONE', #3657, #26702, #8660 ) ;
#22085 = CARTESIAN_POINT ( 'NONE',  ( 6.357667697713668353, 8.357963647880076508, 2.056386458247302595 ) ) ;
#22086 = AXIS2_PLACEMENT_3D ( 'NONE', #4320, #22362, #24709 ) ;
#22087 = EDGE_CURVE ( 'NONE', #29681, #436, #32612, .T. ) ;
#22088 = VECTOR ( 'NONE', #10570, 1000.000000000000000 ) ;
#22089 = CARTESIAN_POINT ( 'NONE',  ( 25.17250000136559507, -3.024605502323851169, 0.3178988483021052969 ) ) ;
#22090 = VECTOR ( 'NONE', #32105, 1000.000000000000000 ) ;
#22091 = CARTESIAN_POINT ( 'NONE',  ( -6.450050802731187360, -2.331437884370912705, 1.887961173149512062 ) ) ;
#22092 = CARTESIAN_POINT ( 'NONE',  ( -3.789055215328666737, -3.339008135070082872, -1.747105332058888738 ) ) ;
#22093 = CARTESIAN_POINT ( 'NONE',  ( 7.064632940817594076, 7.199384779417120406, 4.973063321323900610 ) ) ;
#22094 = EDGE_CURVE ( 'NONE', #20952, #25185, #10752, .T. ) ;
#22095 = CC_DESIGN_APPROVAL ( #29663, ( #15168 ) ) ;
#22096 = CARTESIAN_POINT ( 'NONE',  ( 35.33811999951200278, -4.049688432971601415, 1.529339875354069012 ) ) ;
#22097 = CARTESIAN_POINT ( 'NONE',  ( -2.837550801365592790, -3.675193018007246071, 1.088641768524163167 ) ) ;
#22098 = VERTEX_POINT ( 'NONE', #18608 ) ;
#22099 = CARTESIAN_POINT ( 'NONE',  ( 3.499999999999999556, -2.861184399891040009, 6.440778198864103743 ) ) ;
#22100 = EDGE_LOOP ( 'NONE', ( #3316, #12299, #13957, #9216 ) ) ;
#22101 = LINE ( 'NONE', #4195, #11852 ) ;
#22102 = CARTESIAN_POINT ( 'NONE',  ( 7.249760686538667009, 7.530955069117513112, 2.741043480754951744 ) ) ;
#22103 = CARTESIAN_POINT ( 'NONE',  ( 21.62838417909457434, -16.89547707397456833, 1.499999999999873879 ) ) ;
#22104 = VERTEX_POINT ( 'NONE', #18954 ) ;
#22105 = VECTOR ( 'NONE', #32984, 1000.000000000000114 ) ;
#22106 = CARTESIAN_POINT ( 'NONE',  ( 7.249760686538667009, 2.741043480755029016, -7.530955069117485579 ) ) ;
#22107 = CIRCLE ( 'NONE', #26897, 8.500000000000000000 ) ;
#22108 = ORIENTED_EDGE ( 'NONE', *, *, #14889, .F. ) ;
#22109 = CARTESIAN_POINT ( 'NONE',  ( 8.917092964420161749, 0.3005351010058840977, 1.469472172318631920 ) ) ;
#22111 = ORIENTED_EDGE ( 'NONE', *, *, #6195, .F. ) ;
#22110 = CARTESIAN_POINT ( 'NONE',  ( 18.86047280610195997, -4.736856733801993791, -3.994702635770043475 ) ) ;
#22112 = ORIENTED_EDGE ( 'NONE', *, *, #1379, .T. ) ;
#22113 = AXIS2_PLACEMENT_3D ( 'NONE', #4738, #15407, #24955 ) ;
#22114 = LINE ( 'NONE', #17415, #5992 ) ;
#22115 = EDGE_CURVE ( 'NONE', #9547, #24839, #25677, .T. ) ;
#22117 = ORIENTED_EDGE ( 'NONE', *, *, #6106, .T. ) ;
#22116 = CARTESIAN_POINT ( 'NONE',  ( 25.76000000000000512, 2.749440278475487442, 1.299952413566024756 ) ) ;
#22118 = DIRECTION ( 'NONE',  ( 3.471561733563245301E-15, 0.000000000000000000, -1.000000000000000000 ) ) ;
#22119 = CARTESIAN_POINT ( 'NONE',  ( 22.73500000000000298, -0.2613211581691358698, -2.486304738420681559 ) ) ;
#22120 = CYLINDRICAL_SURFACE ( 'NONE', #30549, 8.749000000000002331 ) ;
#22121 = LOCAL_TIME ( 16, 7, 10.00000000000000000, #1610 ) ;
#22122 = CARTESIAN_POINT ( 'NONE',  ( 0.000000000000000000, 0.000000000000000000, 0.000000000000000000 ) ) ;
#22124 = ORIENTED_EDGE ( 'NONE', *, *, #5217, .F. ) ;
#22123 = CARTESIAN_POINT ( 'NONE',  ( 107.9881338863072955, -17.89849303138035808, -5.107378633373170551 ) ) ;
#22125 = CARTESIAN_POINT ( 'NONE',  ( 7.249760686538667009, -2.741043480754977946, 7.530955069117504230 ) ) ;
#22126 = CARTESIAN_POINT ( 'NONE',  ( 23.49290772595113097, 0.1310194482076003919, 2.499999999999998668 ) ) ;
#22127 = CARTESIAN_POINT ( 'NONE',  ( 24.11000000136559862, -3.156283516753370044, -0.9349337715887220401 ) ) ;
#22128 = ADVANCED_FACE ( 'NONE', ( #6231 ), #28808, .T. ) ;
#22129 = CARTESIAN_POINT ( 'NONE',  ( -2.794738735352966685, 0.000000000000000000, 1.000000000000000000 ) ) ;
#22130 = CARTESIAN_POINT ( 'NONE',  ( 3.499999999999999556, -2.861184399890954300, -6.440778198864141935 ) ) ;
#22131 = VECTOR ( 'NONE', #27331, 1000.000000000000000 ) ;
#22132 = ORIENTED_EDGE ( 'NONE', *, *, #22372, .F. ) ;
#22133 = CARTESIAN_POINT ( 'NONE',  ( 0.08034252266819506827, 1.301095883299763667, 10.71005054582427185 ) ) ;
#22134 = EDGE_CURVE ( 'NONE', #4533, #256, #10945, .T. ) ;
#22135 = CARTESIAN_POINT ( 'NONE',  ( 101.6022419886208610, -1.170867242066746083, -0.4426577266578177183 ) ) ;
#22136 = PLANE ( 'NONE',  #1779 ) ;
#22137 = ORIENTED_EDGE ( 'NONE', *, *, #21010, .F. ) ;
#22138 = DIRECTION ( 'NONE',  ( 0.000000000000000000, 0.000000000000000000, -1.000000000000000000 ) ) ;
#22139 = CARTESIAN_POINT ( 'NONE',  ( 2.748213864407169638, 0.2993382933193693418, -1.561876010259312775 ) ) ;
#22140 = CC_DESIGN_APPROVAL ( #16528, ( #8765 ) ) ;
#22141 = VERTEX_POINT ( 'NONE', #25446 ) ;
#22142 = CARTESIAN_POINT ( 'NONE',  ( 3.249999999999999556, -2.223716399045513548, -8.461683424509336859 ) ) ;
#22143 = EDGE_LOOP ( 'NONE', ( #7152, #17735, #8841, #1459 ) ) ;
#22144 = ORIENTED_EDGE ( 'NONE', *, *, #19773, .T. ) ;
#22145 = CARTESIAN_POINT ( 'NONE',  ( -2.880987360464337677, -0.6119841066606553914, 1.500000000000000000 ) ) ;
#22147 = ORIENTED_EDGE ( 'NONE', *, *, #14296, .T. ) ;
#22146 = CARTESIAN_POINT ( 'NONE',  ( 20.71913853892379009, -21.61372392228101802, -1.559032431776657068 ) ) ;
#22148 = VERTEX_POINT ( 'NONE', #17750 ) ;
#22149 = CARTESIAN_POINT ( 'NONE',  ( 20.79750000136559507, 0.3178988483021036315, 3.024605502323848949 ) ) ;
#22150 = ORIENTED_EDGE ( 'NONE', *, *, #16680, .T. ) ;
#22151 = CARTESIAN_POINT ( 'NONE',  ( 3.499999999999999556, 7.008469740302810891, 2.257469275785292329 ) ) ;
#22152 = CARTESIAN_POINT ( 'NONE',  ( -1.218076164763124636, -14.00532792343563848, 1.500000000000000000 ) ) ;
#22153 = CIRCLE ( 'NONE', #4548, 0.4500000000000025646 ) ;
#22155 = VERTEX_POINT ( 'NONE', #20114 ) ;
#22154 = CARTESIAN_POINT ( 'NONE',  ( 68.94677942527458470, -3.651108094208722843, -1.873789666860088632 ) ) ;
#22156 = CARTESIAN_POINT ( 'NONE',  ( 14.23800746264082839, 22.11259878822726321, 1.508259000770582059 ) ) ;
#22157 = CARTESIAN_POINT ( 'NONE',  ( 3.020080166733955185, 2.264483761675466056, -8.666653390702911963 ) ) ;
#22158 = DIRECTION ( 'NONE',  ( 1.000000000000000000, 0.000000000000000000, -0.000000000000000000 ) ) ;
#22159 = CARTESIAN_POINT ( 'NONE',  ( 24.61000000136559862, 3.156283516753366047, 0.9349337715887203748 ) ) ;
#22160 = CARTESIAN_POINT ( 'NONE',  ( -56.27770248097862549, -0.0003384977252891612984, 0.000000000000000000 ) ) ;
#22161 = CARTESIAN_POINT ( 'NONE',  ( -2.794738735352966685, 0.000000000000000000, 1.000000000000000000 ) ) ;
#22162 = DIRECTION ( 'NONE',  ( -1.000000000000000000, 0.000000000000000000, -0.000000000000000000 ) ) ;
#22163 = CARTESIAN_POINT ( 'NONE',  ( -56.33578448492038859, 0.003046479527604620090, -1.000000000000000000 ) ) ;
#22164 = EDGE_CURVE ( 'NONE', #20879, #8919, #10050, .T. ) ;
#22165 = EDGE_CURVE ( 'NONE', #15916, #27615, #59, .T. ) ;
#22166 = LINE ( 'NONE', #24473, #16589 ) ;
#22167 = DIRECTION ( 'NONE',  ( -1.000000000000000000, 0.000000000000000000, 0.000000000000000000 ) ) ;
#22168 = CARTESIAN_POINT ( 'NONE',  ( -12.44989959798873791, 0.5000000000000000000, -2.982234843104710986 ) ) ;
#22169 = EDGE_CURVE ( 'NONE', #4162, #24626, #24035, .T. ) ;
#22170 = DIRECTION ( 'NONE',  ( 0.000000000000000000, -0.9659258262890689783, -0.2588190451025185190 ) ) ;
#22171 = CARTESIAN_POINT ( 'NONE',  ( -4.450050802731187360, 2.331437884370912705, -1.887961173149511618 ) ) ;
#22172 = VERTEX_POINT ( 'NONE', #30817 ) ;
#22173 = CARTESIAN_POINT ( 'NONE',  ( -3.800050800000000617, -1.887961173149512062, -2.331437884370912261 ) ) ;
#22174 = FACE_OUTER_BOUND ( 'NONE', #25270, .T. ) ;
#22175 = CARTESIAN_POINT ( 'NONE',  ( 3.122314033877900197E-16, 3.641590349731971710, -3.055657119358763829 ) ) ;
#22176 = ORIENTED_EDGE ( 'NONE', *, *, #5664, .T. ) ;
#22177 = CARTESIAN_POINT ( 'NONE',  ( 7.249760686538667009, 1.391664247347228045, 7.892520144992438702 ) ) ;
#22178 = CARTESIAN_POINT ( 'NONE',  ( 7.868768533615001282, -10.68327055928632063, -1.499999999999999778 ) ) ;
#22179 = ORIENTED_EDGE ( 'NONE', *, *, #8134, .T. ) ;
#22180 = CARTESIAN_POINT ( 'NONE',  ( 101.7221769401408409, -2.897900707892763439, -3.993434276071010203 ) ) ;
#22181 = CALENDAR_DATE ( 2026, 6, 10 ) ;
#22182 = PLANE ( 'NONE',  #15501 ) ;
#22183 = VERTEX_POINT ( 'NONE', #10550 ) ;
#22184 = CARTESIAN_POINT ( 'NONE',  ( -3.828326524025771782, -10.43756472495370247, 1.499999999999999778 ) ) ;
#22185 =( BOUNDED_CURVE ( )  B_SPLINE_CURVE ( 2, ( #3140, #26036, #13297, #21027, #31533, #26377, #23837, #13635, #28366, #15672, #31235 ),
 .UNSPECIFIED., .F., .F. ) 
 B_SPLINE_CURVE_WITH_KNOTS ( ( 3, 2, 2, 2, 2, 3 ),
 ( 0.4966116191895003640, 0.5000000000000000000, 0.5250000000000000222, 0.5500000000000000444, 0.5749999999999999556, 0.5966116191895003418 ),
 .UNSPECIFIED. ) 
 CURVE ( )  GEOMETRIC_REPRESENTATION_ITEM ( )  RATIONAL_B_SPLINE_CURVE ( ( 0.9821626249036858880, 0.9896829947469992783, 1.000000000000000000, 0.9238795325112867385, 1.000000000000000000, 0.9238795325112867385, 1.000000000000000000, 0.9238795325112867385, 1.000000000000000000, 0.9341965377642874602, 0.9821626249036858880 ) ) 
 REPRESENTATION_ITEM ( '' )  );
#22186 = CARTESIAN_POINT ( 'NONE',  ( -5.850050800000001772, 2.853674364686379583, 1.549418761218565921 ) ) ;
#22187 = CARTESIAN_POINT ( 'NONE',  ( 28.66410178494867367, -6.765307663812238914, -3.993434336023267139 ) ) ;
#22188 = FACE_OUTER_BOUND ( 'NONE', #10680, .T. ) ;
#22189 = DIRECTION ( 'NONE',  ( -0.000000000000000000, -0.3746065934159164001, 0.9271838545667856479 ) ) ;
#22190 = B_SPLINE_CURVE_WITH_KNOTS ( 'NONE', 3,
 ( #31015, #17977, #15795, #23168, #30864, #7934, #28319, #23320, #26001, #422 ),
 .UNSPECIFIED., .F., .F.,
 ( 4, 2, 2, 2, 4 ),
 ( 3.032460776734494555E-07, 0.0005479053915603975021, 0.001095507537043121683, 0.001643109682525845539, 0.002190711828008569395 ),
 .UNSPECIFIED. ) ;
#22191 = ORIENTED_EDGE ( 'NONE', *, *, #28996, .T. ) ;
#22192 = DIRECTION ( 'NONE',  ( 0.000000000000000000, 0.4226182617406914477, 0.9063077870366536004 ) ) ;
#22193 = CARTESIAN_POINT ( 'NONE',  ( 23.27353193731599745, -21.94187811905321794, -1.045377498472113587 ) ) ;
#22194 = CARTESIAN_POINT ( 'NONE',  ( 0.000000000000000000, 0.5000000000000000000, 7.482234843104714983 ) ) ;
#22195 = EDGE_CURVE ( 'NONE', #3357, #8422, #2714, .T. ) ;
#22197 = ORIENTED_EDGE ( 'NONE', *, *, #178, .F. ) ;
#22196 = DIRECTION ( 'NONE',  ( -0.000000000000000000, -0.000000000000000000, -1.000000000000000000 ) ) ;
#22198 = CARTESIAN_POINT ( 'NONE',  ( 0.000000000000000000, -5.349675154362342866, 3.229702268444914370 ) ) ;
#22199 = CARTESIAN_POINT ( 'NONE',  ( 25.75999999999999801, -1.838216977691246972E-15, 3.024999999999999911 ) ) ;
#22200 = DIRECTION ( 'NONE',  ( -4.917867153432939248E-17, -0.5735764363510388320, -0.8191520442889969056 ) ) ;
#22201 = CARTESIAN_POINT ( 'NONE',  ( 24.97915472029188066, 18.93975620935289683, 1.499999999999998446 ) ) ;
#22202 = LINE ( 'NONE', #24206, #18912 ) ;
#22203 = CARTESIAN_POINT ( 'NONE',  ( 6.524594682510452159, 0.6222547417166542916, 8.636529731786346531 ) ) ;
#22204 = CYLINDRICAL_SURFACE ( 'NONE', #26794, 4.000000000000001776 ) ;
#22205 = FACE_OUTER_BOUND ( 'NONE', #17479, .T. ) ;
#22206 = CARTESIAN_POINT ( 'NONE',  ( -30.17749803717425294, 10.76421938935684075, 1.964586347758968232 ) ) ;
#22207 = EDGE_LOOP ( 'NONE', ( #19704, #12066, #3061, #19827 ) ) ;
#22208 = CARTESIAN_POINT ( 'NONE',  ( 3.499999999999999556, -4.147285340411824173, 5.698247474649390298 ) ) ;
#22209 = ORIENTED_EDGE ( 'NONE', *, *, #16398, .T. ) ;
#22210 = CARTESIAN_POINT ( 'NONE',  ( -6.054531657079158080, 1.545410377633947174, -2.846291840500173365 ) ) ;
#22211 = CARTESIAN_POINT ( 'NONE',  ( -3.529825581556913254E-16, -4.116875700062066379, -2.376879293651108060 ) ) ;
#22212 = LINE ( 'NONE', #9649, #20499 ) ;
#22213 = CARTESIAN_POINT ( 'NONE',  ( 2.437082530871053532, 9.289394354155845690, -5.244446742619389035 ) ) ;
#22214 = DIRECTION ( 'NONE',  ( -1.000000000000000000, 0.000000000000000000, 0.000000000000000000 ) ) ;
#22215 = EDGE_LOOP ( 'NONE', ( #6113, #26203, #4568, #14416 ) ) ;
#22216 = DIRECTION ( 'NONE',  ( -1.000000000000000000, 0.000000000000000000, 0.000000000000000000 ) ) ;
#22217 = VERTEX_POINT ( 'NONE', #2555 ) ;
#22218 = SECURITY_CLASSIFICATION_LEVEL ( 'unclassified' ) ;
#22219 = EDGE_CURVE ( 'NONE', #15097, #7918, #18180, .T. ) ;
#22220 = CARTESIAN_POINT ( 'NONE',  ( 85.03457044784497043, -5.184453191149429152, 4.023789378550656437 ) ) ;
#22221 = B_SPLINE_CURVE_WITH_KNOTS ( 'NONE', 3,
 ( #13810, #8338, #3654, #24016, #13506, #8181 ),
 .UNSPECIFIED., .F., .F.,
 ( 4, 2, 4 ),
 ( 0.000000000000000000, 0.001111101127398034585, 0.002222202254796068737 ),
 .UNSPECIFIED. ) ;
#22222 = CARTESIAN_POINT ( 'NONE',  ( 7.259701896292244605, -5.595974087570425581, -0.9999999999999997780 ) ) ;
#22224 = DIRECTION ( 'NONE',  ( 1.000000000000000000, -0.000000000000000000, -0.000000000000000000 ) ) ;
#22223 = DIRECTION ( 'NONE',  ( -1.000000000000000000, 0.000000000000000000, 0.000000000000000000 ) ) ;
#22225 = ADVANCED_FACE ( 'NONE', ( #227 ), #5912, .T. ) ;
#22226 = ORIENTED_EDGE ( 'NONE', *, *, #4340, .F. ) ;
#22227 = LINE ( 'NONE', #4338, #11357 ) ;
#22228 = FACE_OUTER_BOUND ( 'NONE', #12069, .T. ) ;
#22229 = CARTESIAN_POINT ( 'NONE',  ( 22.92250000000000298, 2.378061970571979433, -1.291182301015470824 ) ) ;
#22230 = CARTESIAN_POINT ( 'NONE',  ( 0.1996956927336154264, -7.570410372035627944, -1.774174135624665638 ) ) ;
#22232 = ORIENTED_EDGE ( 'NONE', *, *, #30021, .F. ) ;
#22231 = CARTESIAN_POINT ( 'NONE',  ( 109.3993806922052698, 20.31298924473501444, 2.334455007174201402 ) ) ;
#22233 = CARTESIAN_POINT ( 'NONE',  ( -2.737550801365594477, -3.368539882008727115, -1.828967928396028064 ) ) ;
#22234 = DIRECTION ( 'NONE',  ( -0.08910563629484158366, -0.9960221812693186294, 0.000000000000000000 ) ) ;
#22235 = CARTESIAN_POINT ( 'NONE',  ( 7.249760686538667009, 0.000000000000000000, 0.000000000000000000 ) ) ;
#22237 = EDGE_CURVE ( 'NONE', #30215, #24312, #20551, .T. ) ;
#22236 = CARTESIAN_POINT ( 'NONE',  ( 17.33093461831546378, -21.43932300456649642, -1.950000000000000178 ) ) ;
#22238 = VERTEX_POINT ( 'NONE', #10401 ) ;
#22240 = ORIENTED_EDGE ( 'NONE', *, *, #2235, .T. ) ;
#22239 = CARTESIAN_POINT ( 'NONE',  ( 3.744708216408842549, 0.000000000000000000, 1.000000000000000000 ) ) ;
#22241 = EDGE_CURVE ( 'NONE', #25155, #16376, #31678, .T. ) ;
#22242 = CARTESIAN_POINT ( 'NONE',  ( 18.77228938565977145, 14.95012848542240746, 1.500000000000000666 ) ) ;
#22243 = LINE ( 'NONE', #27082, #31241 ) ;
#22244 = EDGE_CURVE ( 'NONE', #2486, #1971, #12820, .T. ) ;
#22245 = CARTESIAN_POINT ( 'NONE',  ( 24.79750000136559507, 2.363507492473148286, 1.913930629741525058 ) ) ;
#22246 = CARTESIAN_POINT ( 'NONE',  ( -28.96127135574216638, 15.72250979567477636, 1.500000000000000000 ) ) ;
#22247 = CARTESIAN_POINT ( 'NONE',  ( 6.070010019446702820, -18.63414725979056641, -1.500000000000000444 ) ) ;
#22248 = CARTESIAN_POINT ( 'NONE',  ( 25.75999999999999801, -2.208672634433321348E-15, 0.000000000000000000 ) ) ;
#22249 = CARTESIAN_POINT ( 'NONE',  ( 18.97818541979132334, -3.421065958672417473, 1.873789191073851335 ) ) ;
#22250 = CARTESIAN_POINT ( 'NONE',  ( -3.537550801365593411, -3.368539882008727115, -1.828967928396028064 ) ) ;
#22251 = ORIENTED_EDGE ( 'NONE', *, *, #32998, .T. ) ;
#22252 = FACE_OUTER_BOUND ( 'NONE', #27519, .T. ) ;
#22253 = EDGE_LOOP ( 'NONE', ( #17695, #16984, #787, #23449 ) ) ;
#22254 = EDGE_CURVE ( 'NONE', #25766, #8558, #15893, .T. ) ;
#22255 = LINE ( 'NONE', #25072, #9248 ) ;
#22256 = DIRECTION ( 'NONE',  ( 1.000000000000000000, 0.000000000000000000, 0.000000000000000000 ) ) ;
#22257 = DIRECTION ( 'NONE',  ( -1.000000000000000000, -0.000000000000000000, 0.000000000000000000 ) ) ;
#22258 = CARTESIAN_POINT ( 'NONE',  ( -41.54004718934325524, -10.96999999999998643, 9.000000000000000000 ) ) ;
#22259 = ORIENTED_EDGE ( 'NONE', *, *, #7592, .F. ) ;
#22260 = CARTESIAN_POINT ( 'NONE',  ( 10.00000000000000000, 1.115095498423308129, 4.884328206559840346 ) ) ;
#22261 = ORIENTED_EDGE ( 'NONE', *, *, #21738, .T. ) ;
#22262 = DIRECTION ( 'NONE',  ( 1.000000000000000000, -0.000000000000000000, -0.000000000000000000 ) ) ;
#22264 = ORIENTED_EDGE ( 'NONE', *, *, #21629, .F. ) ;
#22263 = CARTESIAN_POINT ( 'NONE',  ( 28.69355920165661900, -5.617338241167577628, -3.995970707775803987 ) ) ;
#22265 = EDGE_LOOP ( 'NONE', ( #5231, #18597, #9537, #4777 ) ) ;
#22266 = CARTESIAN_POINT ( 'NONE',  ( 56.97280603064898941, -277.2763395528616002, 2.334455007174208507 ) ) ;
#22267 = CARTESIAN_POINT ( 'NONE',  ( 102.5484925806840977, -0.3622080806379257556, 1.915219082070892531 ) ) ;
#22269 = ORIENTED_EDGE ( 'NONE', *, *, #743, .F. ) ;
#22268 = CARTESIAN_POINT ( 'NONE',  ( 107.4094642854696104, -16.77596786109937099, 3.324293658051870715 ) ) ;
#22270 = DIRECTION ( 'NONE',  ( 1.000000000000000000, 0.000000000000000000, 0.000000000000000000 ) ) ;
#22271 = CARTESIAN_POINT ( 'NONE',  ( 9.174708406371143710, 0.09531162291655657925, -1.030456265918283654 ) ) ;
#22272 = DIRECTION ( 'NONE',  ( -1.000000000000000000, -0.000000000000000000, -0.000000000000000000 ) ) ;
#22273 = EDGE_CURVE ( 'NONE', #9461, #24987, #14969, .T. ) ;
#22274 = CARTESIAN_POINT ( 'NONE',  ( 8.845957756505633540, -0.9823800962674188453, -1.000000000000000000 ) ) ;
#22276 = ORIENTED_EDGE ( 'NONE', *, *, #29625, .F. ) ;
#22275 = CARTESIAN_POINT ( 'NONE',  ( 107.5220891496032891, -18.40716237041415937, -5.108771864772584159 ) ) ;
#22277 = EDGE_CURVE ( 'NONE', #4152, #19569, #26211, .T. ) ;
#22278 = CARTESIAN_POINT ( 'NONE',  ( 3.020080256212050784, -6.926136578642532626, 5.680439424464613474 ) ) ;
#22279 = PLANE ( 'NONE',  #15554 ) ;
#22280 = CARTESIAN_POINT ( 'NONE',  ( 25.79750000136559507, 0.3178988483021036315, 3.024605502323848949 ) ) ;
#22281 = DIRECTION ( 'NONE',  ( 1.000000000000000000, 0.000000000000000000, 0.000000000000000000 ) ) ;
#22282 = CARTESIAN_POINT ( 'NONE',  ( 3.499999999999999556, 0.000000000000000000, 0.000000000000000000 ) ) ;
#22283 = DIRECTION ( 'NONE',  ( -1.000000000000000000, 0.000000000000000000, 0.000000000000000000 ) ) ;
#22284 = EDGE_LOOP ( 'NONE', ( #6627, #27829, #14290, #30827, #15373 ) ) ;
#22285 = CARTESIAN_POINT ( 'NONE',  ( 5.887530180601101115, -4.515817126386058256, 7.076866030741298275 ) ) ;
#22286 = DIRECTION ( 'NONE',  ( -1.000000000000000000, -0.000000000000000000, -0.000000000000000000 ) ) ;
#22287 = CARTESIAN_POINT ( 'NONE',  ( -7.887550801365593500, 2.228590825266444142, 2.752080473201636845 ) ) ;
#22288 = ORIENTED_EDGE ( 'NONE', *, *, #23807, .T. ) ;
#22289 = EDGE_CURVE ( 'NONE', #9958, #28295, #11200, .T. ) ;
#22290 = CC_DESIGN_PERSON_AND_ORGANIZATION_ASSIGNMENT ( #15189, #5319, ( #27439 ) ) ;
#22291 = DIRECTION ( 'NONE',  ( 1.000000000000000000, 0.000000000000000000, 0.000000000000000000 ) ) ;
#22292 = CARTESIAN_POINT ( 'NONE',  ( 16.70660563659856734, -16.26387199941004624, -0.9788672205888330202 ) ) ;
#22293 = EDGE_LOOP ( 'NONE', ( #25630, #9950, #6362, #13961 ) ) ;
#22294 = LINE ( 'NONE', #6589, #15569 ) ;
#22295 = VERTEX_POINT ( 'NONE', #3206 ) ;
#22296 = ORIENTED_EDGE ( 'NONE', *, *, #17900, .F. ) ;
#22297 = LINE ( 'NONE', #27802, #10246 ) ;
#22298 = PRODUCT_DEFINITION_SHAPE ( 'NONE', 'NONE',  #28213 ) ;
#22300 = VERTEX_POINT ( 'NONE', #3060 ) ;
#22299 = CARTESIAN_POINT ( 'NONE',  ( -10.00000000000000000, 0.000000000000000000, 0.000000000000000000 ) ) ;
#22301 = ORIENTED_EDGE ( 'NONE', *, *, #1635, .F. ) ;
#22302 = CARTESIAN_POINT ( 'NONE',  ( 22.61000000136559507, 3.156283516753366047, 0.9349337715887203748 ) ) ;
#22303 = EDGE_CURVE ( 'NONE', #32838, #2837, #16055, .T. ) ;
#22304 = ORIENTED_EDGE ( 'NONE', *, *, #551, .T. ) ;
#22305 = FACE_OUTER_BOUND ( 'NONE', #30923, .T. ) ;
#22307 = VERTEX_POINT ( 'NONE', #6198 ) ;
#22306 = CARTESIAN_POINT ( 'NONE',  ( -50.60000000000000142, -10.96966150227468972, 7.500000000000000000 ) ) ;
#22308 = CARTESIAN_POINT ( 'NONE',  ( -56.34447759643617815, 0.004136860324227145148, -1.003319227365814470 ) ) ;
#22309 = CARTESIAN_POINT ( 'NONE',  ( 18.58227844715246135, -7.846511338401735536, 2.713652344655542503 ) ) ;
#22310 = CARTESIAN_POINT ( 'NONE',  ( 22.48500000136559507, 2.892927487894327410, -1.570731468192931635 ) ) ;
#22311 = DIRECTION ( 'NONE',  ( 0.000000000000000000, 0.000000000000000000, 1.000000000000000000 ) ) ;
#22312 = CARTESIAN_POINT ( 'NONE',  ( -0.5220033361344396106, 0.000000000000000000, -5.485967528433938867 ) ) ;
#22313 = CARTESIAN_POINT ( 'NONE',  ( 107.9151932993304968, -16.84816672442089569, -3.542199815890097359 ) ) ;
#22314 = DIRECTION ( 'NONE',  ( 1.000000000000000000, 0.000000000000000000, 0.000000000000000000 ) ) ;
#22315 = CARTESIAN_POINT ( 'NONE',  ( -29.65619690862280677, -28.43932300454937590, 11.00000000000000000 ) ) ;
#22316 = CARTESIAN_POINT ( 'NONE',  ( -1.921189184902825975, -10.44034746380417822, 4.522129901861159595 ) ) ;
#22317 = DIRECTION ( 'NONE',  ( 1.000000000000000000, -8.574039729943018344E-17, -0.000000000000000000 ) ) ;
#22318 = CARTESIAN_POINT ( 'NONE',  ( 23.84714171513466141, -3.444070612163573575, 0.07017451550800275772 ) ) ;
#22319 = CARTESIAN_POINT ( 'NONE',  ( 34.99999999999999289, 0.000000000000000000, 0.9987809114025958390 ) ) ;
#22320 = ADVANCED_FACE ( 'NONE', ( #28764 ), #3774, .F. ) ;
#22321 = CARTESIAN_POINT ( 'NONE',  ( -4.750050802731187183, -2.983565686104819648, -0.3135853898029605791 ) ) ;
#22322 = EDGE_LOOP ( 'NONE', ( #8212, #32474, #6219, #1367 ) ) ;
#22323 = CARTESIAN_POINT ( 'NONE',  ( -2.850050800000000439, 1.549418761218566143, -2.853674364686379583 ) ) ;
#22324 = PLANE ( 'NONE',  #31686 ) ;
#22325 = CARTESIAN_POINT ( 'NONE',  ( -4.156376981307135843, -0.1572233378491262878, 2.999999999999999556 ) ) ;
#22326 = ORIENTED_EDGE ( 'NONE', *, *, #201, .T. ) ;
#22327 = CARTESIAN_POINT ( 'NONE',  ( 3.499999999999999556, 0.000000000000000000, 0.000000000000000000 ) ) ;
#22328 = CARTESIAN_POINT ( 'NONE',  ( 6.880159329304570193, -6.122988934091237567, -6.224287131858866395 ) ) ;
#22329 = VERTEX_POINT ( 'NONE', #31616 ) ;
#22330 = CARTESIAN_POINT ( 'NONE',  ( 2.558140769686992222, 8.984438712799688531, 5.239665997526921970 ) ) ;
#22331 = APPLICATION_PROTOCOL_DEFINITION ( 'international standard', 'config_control_design', 1994, #7986 ) ;
#22332 = CARTESIAN_POINT ( 'NONE',  ( -2.600050800000000883, 1.887961173149511618, 2.331437884370912705 ) ) ;
#22333 = ORIENTED_EDGE ( 'NONE', *, *, #17594, .T. ) ;
#22334 = CARTESIAN_POINT ( 'NONE',  ( -7.077711312404582636E-17, -0.8254815157535566605, 4.681538312723514395 ) ) ;
#22335 = EDGE_CURVE ( 'NONE', #8396, #10028, #11778, .T. ) ;
#22336 = EDGE_CURVE ( 'NONE', #14852, #17282, #17652, .T. ) ;
#22337 = ORIENTED_EDGE ( 'NONE', *, *, #26381, .T. ) ;
#22338 = LINE ( 'NONE', #7140, #20314 ) ;
#22339 = CARTESIAN_POINT ( 'NONE',  ( 40.88371753250735452, -6.846020710327327841, -4.074609548160287531 ) ) ;
#22340 = CYLINDRICAL_SURFACE ( 'NONE', #26748, 8.749000000000002331 ) ;
#22341 = DIRECTION ( 'NONE',  ( 0.000000000000000000, 0.4226182617406901154, 0.9063077870366543776 ) ) ;
#22342 = ADVANCED_FACE ( 'NONE', ( #704 ), #16381, .F. ) ;
#22343 = ORIENTED_EDGE ( 'NONE', *, *, #25349, .F. ) ;
#22344 = CARTESIAN_POINT ( 'NONE',  ( 21.45958739454658115, -21.75417579598725126, -1.461374457712235175 ) ) ;
#22345 = DIRECTION ( 'NONE',  ( -1.000000000000000000, 0.000000000000000000, 0.000000000000000000 ) ) ;
#22347 = VERTEX_POINT ( 'NONE', #31303 ) ;
#22346 = DIRECTION ( 'NONE',  ( -1.000000000000000000, 0.000000000000000000, 0.000000000000000000 ) ) ;
#22348 = DIRECTION ( 'NONE',  ( -1.000000000000000000, 0.000000000000000000, 0.000000000000000000 ) ) ;
#22349 = PLANE ( 'NONE',  #18709 ) ;
#22350 = CARTESIAN_POINT ( 'NONE',  ( -38.14293509397970183, 21.49000000000000199, -1.050000000000000044 ) ) ;
#22351 = DIRECTION ( 'NONE',  ( -0.9993908270190956511, 0.03489949670250350189, -1.734723475976808475E-15 ) ) ;
#22352 = CARTESIAN_POINT ( 'NONE',  ( 69.13057415542957074, -2.987362752442195291, -2.713652344655540727 ) ) ;
#22353 = CARTESIAN_POINT ( 'NONE',  ( -8.000050800000000351, 3.273954799371778801, 1.157949676854548526 ) ) ;
#22354 = CARTESIAN_POINT ( 'NONE',  ( 5.887530252753765403, -6.185189124321781584, -5.676096663009868593 ) ) ;
#22355 = CARTESIAN_POINT ( 'NONE',  ( -31.57659242536668032, -21.93932300455408324, -1.000000000000000000 ) ) ;
#22356 = CARTESIAN_POINT ( 'NONE',  ( 23.27353193731607206, -21.94187811905322505, 1.045377498471069089 ) ) ;
#22357 = VERTEX_POINT ( 'NONE', #8702 ) ;
#22358 = CARTESIAN_POINT ( 'NONE',  ( 20.55656763645045260, -0.8852964313267484009, 2.499999999999997780 ) ) ;
#22359 = ORIENTED_EDGE ( 'NONE', *, *, #17871, .F. ) ;
#22360 = CARTESIAN_POINT ( 'NONE',  ( -5.254531657079158258, 1.545410377633947174, -2.846291840500173365 ) ) ;
#22361 = CARTESIAN_POINT ( 'NONE',  ( 24.92250000136559507, 0.3178988483021036315, 3.024605502323848949 ) ) ;
#22362 = DIRECTION ( 'NONE',  ( 0.000000000000000000, 0.000000000000000000, -1.000000000000000000 ) ) ;
#22363 = DIRECTION ( 'NONE',  ( 0.1908089953765420843, -0.000000000000000000, -0.9816271834476646418 ) ) ;
#22364 = DIRECTION ( 'NONE',  ( 0.000000000000000000, -0.000000000000000000, -1.000000000000000000 ) ) ;
#22365 = ORIENTED_EDGE ( 'NONE', *, *, #29176, .T. ) ;
#22366 = DIRECTION ( 'NONE',  ( -1.000000000000000000, -0.000000000000000000, -0.000000000000000000 ) ) ;
#22367 = ADVANCED_FACE ( 'NONE', ( #18918 ), #31143, .T. ) ;
#22368 = ORIENTED_EDGE ( 'NONE', *, *, #20764, .T. ) ;
#22369 = APPLICATION_PROTOCOL_DEFINITION ( 'international standard', 'config_control_design', 1994, #520 ) ;
#22370 = CARTESIAN_POINT ( 'NONE',  ( 54.97709061282851195, -6.501732682086259096, 4.001040679971932690 ) ) ;
#22371 = EDGE_CURVE ( 'NONE', #5198, #16296, #11384, .T. ) ;
#22372 = EDGE_CURVE ( 'NONE', #17732, #10281, #18881, .T. ) ;
#22373 = EDGE_CURVE ( 'NONE', #28214, #30338, #9560, .T. ) ;
#22374 = DIRECTION ( 'NONE',  ( 1.000000000000000000, 0.000000000000000000, 0.000000000000000000 ) ) ;
#22376 = CARTESIAN_POINT ( 'NONE',  ( 25.56220348721820201, -1.341958225229829886E-11, -2.827203487218203914 ) ) ;
#22375 = DIRECTION ( 'NONE',  ( -1.000000000000000000, 0.000000000000000000, 0.000000000000000000 ) ) ;
#22377 = ORIENTED_EDGE ( 'NONE', *, *, #19914, .F. ) ;
#22378 = CARTESIAN_POINT ( 'NONE',  ( 4.749760686538667009, -2.741043480754977946, 7.530955069117504230 ) ) ;
#22379 = CARTESIAN_POINT ( 'NONE',  ( 6.524595551582240915, -7.790581746767706761, -3.779376390944553243 ) ) ;
#22380 = CARTESIAN_POINT ( 'NONE',  ( 25.67250000136559507, 3.024605502323846729, -0.3178988483021056854 ) ) ;
#22381 = CARTESIAN_POINT ( 'NONE',  ( 0.6389947482386004740, -7.663676466994388647, -1.499999999999999556 ) ) ;
#22383 = ORIENTED_EDGE ( 'NONE', *, *, #29524, .T. ) ;
#22382 = CARTESIAN_POINT ( 'NONE',  ( 107.5965811620429093, 18.76554845876667343, 5.148257179709845310 ) ) ;
#22384 = CARTESIAN_POINT ( 'NONE',  ( -4.737550801365593145, 3.368539882008727115, 1.828967928396026954 ) ) ;
#22385 = CARTESIAN_POINT ( 'NONE',  ( 107.7536796087345294, 16.80655079293032017, -1.379243061950440108 ) ) ;
#22386 = FACE_OUTER_BOUND ( 'NONE', #5066, .T. ) ;
#22387 = CARTESIAN_POINT ( 'NONE',  ( 7.249760686538667009, 5.151476664237558900, -6.139290821770204687 ) ) ;
#22388 = ORIENTED_EDGE ( 'NONE', *, *, #4583, .T. ) ;
#22390 = ORIENTED_EDGE ( 'NONE', *, *, #29581, .T. ) ;
#22389 = DIRECTION ( 'NONE',  ( 0.000000000000000000, -0.08715574274766618723, 0.9961946980917448791 ) ) ;
#22391 = CIRCLE ( 'NONE', #26148, 3.000000000000000444 ) ;
#22392 = DIRECTION ( 'NONE',  ( 0.000000000000000000, 0.000000000000000000, 1.000000000000000000 ) ) ;
#22393 =( BOUNDED_CURVE ( )  B_SPLINE_CURVE ( 2, ( #19332, #30323, #27017, #6436, #4120, #16640, #27167, #14287, #17587, #11791, #12586 ),
 .UNSPECIFIED., .F., .F. ) 
 B_SPLINE_CURVE_WITH_KNOTS ( ( 3, 2, 2, 2, 2, 3 ),
 ( 0.3103822619934377136, 0.3125000000000000000, 0.3281250000000000000, 0.3437500000000000000, 0.3593750000000000000, 0.3728822619934377136 ),
 .UNSPECIFIED. ) 
 CURVE ( )  GEOMETRIC_REPRESENTATION_ITEM ( )  RATIONAL_B_SPLINE_CURVE ( ( 0.9821626249036857770, 0.9896829947469991673, 1.000000000000000000, 0.9238795325112867385, 1.000000000000000000, 0.9238795325112867385, 1.000000000000000000, 0.9238795325112867385, 1.000000000000000000, 0.9341965377642874602, 0.9821626249036857770 ) ) 
 REPRESENTATION_ITEM ( '' )  );
#22394 = CARTESIAN_POINT ( 'NONE',  ( -23.54713438637982748, 18.90773822806172433, 1.500000000000000000 ) ) ;
#22395 = CARTESIAN_POINT ( 'NONE',  ( 25.67250000136559507, 3.024605502323846729, -0.3178988483021056854 ) ) ;
#22396 = CYLINDRICAL_SURFACE ( 'NONE', #18255, 12.49867430706171767 ) ;
#22397 = CARTESIAN_POINT ( 'NONE',  ( 7.581061048149257964, -18.74603139903822324, -1.749278969417850549 ) ) ;
#22398 = CARTESIAN_POINT ( 'NONE',  ( 0.000000000000000000, 2.429606751577043422, 5.757344182232919216 ) ) ;
#22399 = EDGE_CURVE ( 'NONE', #33011, #4959, #19278, .T. ) ;
#22400 = CARTESIAN_POINT ( 'NONE',  ( 23.86731473547942173, -3.600650094301432791, 1.169950778993111173 ) ) ;
#22401 = CARTESIAN_POINT ( 'NONE',  ( 0.7212198416586409477, 6.922088825865693629, 5.676697589981143821 ) ) ;
#22402 = ORIENTED_EDGE ( 'NONE', *, *, #1597, .F. ) ;
#22403 = CARTESIAN_POINT ( 'NONE',  ( 34.98223484310472031, 0.5000000000000000000, -2.999999999999995559 ) ) ;
#22404 = ORIENTED_EDGE ( 'NONE', *, *, #10179, .F. ) ;
#22405 = AXIS2_PLACEMENT_3D ( 'NONE', #10727, #13382, #25969 ) ;
#22406 = ADVANCED_FACE ( 'NONE', ( #29423 ), #9509, .F. ) ;
#22407 = AXIS2_PLACEMENT_3D ( 'NONE', #18322, #21480, #10615 ) ;
#22408 = CARTESIAN_POINT ( 'NONE',  ( 25.75999999999999801, -2.208672634433321348E-15, 0.000000000000000000 ) ) ;
#22409 = B_SPLINE_CURVE_WITH_KNOTS ( 'NONE', 3,
 ( #22116, #32329, #29798, #29287 ),
 .UNSPECIFIED., .F., .F.,
 ( 4, 4 ),
 ( 1.353369231834851200E-16, 0.0001748182243391414533 ),
 .UNSPECIFIED. ) ;
#22410 = EDGE_CURVE ( 'NONE', #13368, #3046, #1867, .T. ) ;
#22411 = DIRECTION ( 'NONE',  ( 0.9816271834476637537, 0.000000000000000000, 0.1908089953765453872 ) ) ;
#22412 = ADVANCED_FACE ( 'NONE', ( #24904 ), #2017, .F. ) ;
#22413 = ORIENTED_EDGE ( 'NONE', *, *, #18173, .F. ) ;
#22414 = CIRCLE ( 'NONE', #26173, 3.499999999999999556 ) ;
#22415 = CARTESIAN_POINT ( 'NONE',  ( 0.000000000000000000, -5.233522515400055752, -4.720195129223329289 ) ) ;
#22416 = ORIENTED_EDGE ( 'NONE', *, *, #5727, .F. ) ;
#22417 = CARTESIAN_POINT ( 'NONE',  ( 2.440333456264102363, -10.60697035672505706, 1.206185435479571133 ) ) ;
#22419 = ORIENTED_EDGE ( 'NONE', *, *, #13829, .F. ) ;
#22418 = CARTESIAN_POINT ( 'NONE',  ( 84.96617506415587684, -4.068705388295901670, -4.008636570259113796 ) ) ;
#22420 = EDGE_CURVE ( 'NONE', #9958, #5198, #11873, .T. ) ;
#22421 = EDGE_LOOP ( 'NONE', ( #10035, #9766, #30365, #23404 ) ) ;
#22422 = CARTESIAN_POINT ( 'NONE',  ( 0.000000000000000000, 0.000000000000000000, -1.500000000000000000 ) ) ;
#22424 = ORIENTED_EDGE ( 'NONE', *, *, #21152, .T. ) ;
#22423 = CARTESIAN_POINT ( 'NONE',  ( -28.35000000000000497, -10.96966150227469505, 4.000000000000000000 ) ) ;
#22425 = CARTESIAN_POINT ( 'NONE',  ( 6.037141869538512395, 4.619542287584905260, 7.104659103919362728 ) ) ;
#22426 = CARTESIAN_POINT ( 'NONE',  ( 8.870145747188287189, 0.000000000000000000, -1.000000000000001332 ) ) ;
#22427 = ADVANCED_FACE ( 'NONE', ( #12043 ), #11693, .T. ) ;
#22428 = DIRECTION ( 'NONE',  ( -1.000000000000000000, -0.000000000000000000, -0.000000000000000000 ) ) ;
#22430 = ORIENTED_EDGE ( 'NONE', *, *, #13399, .T. ) ;
#22429 = CARTESIAN_POINT ( 'NONE',  ( 107.9813876837010156, -17.80134939207562184, -4.369343856298157469 ) ) ;
#22431 = CYLINDRICAL_SURFACE ( 'NONE', #13544, 5.010000000000000675 ) ;
#22432 = EDGE_CURVE ( 'NONE', #8954, #1225, #20342, .T. ) ;
#22433 = AXIS2_PLACEMENT_3D ( 'NONE', #19852, #22196, #29876 ) ;
#22434 = VECTOR ( 'NONE', #26356, 1000.000000000000000 ) ;
#22435 = CARTESIAN_POINT ( 'NONE',  ( 23.00111451137534502, -1.283275288181523244E-15, -2.499999999999998668 ) ) ;
#22436 = CARTESIAN_POINT ( 'NONE',  ( 23.79750000136559507, 0.3178988483021036315, 3.024605502323848949 ) ) ;
#22437 = EDGE_CURVE ( 'NONE', #6440, #29313, #6473, .T. ) ;
#22438 = CARTESIAN_POINT ( 'NONE',  ( 107.4685836152551417, 18.03047445837466256, -4.889869265036825396 ) ) ;
#22439 = CARTESIAN_POINT ( 'NONE',  ( 24.44878497425310826, -17.43662272166809046, -1.459033525497872796 ) ) ;
#22440 = CARTESIAN_POINT ( 'NONE',  ( -17.04380309137718541, -27.93932300454937590, 11.50000000000000000 ) ) ;
#22441 = AXIS2_PLACEMENT_3D ( 'NONE', #30741, #20347, #7645 ) ;
#22442 = ORIENTED_EDGE ( 'NONE', *, *, #18359, .F. ) ;
#22443 = LINE ( 'NONE', #4732, #3366 ) ;
#22444 = ADVANCED_FACE ( 'NONE', ( #24248 ), #19840, .F. ) ;
#22445 = DIRECTION ( 'NONE',  ( 1.000000000000000000, 0.000000000000000000, 0.000000000000000000 ) ) ;
#22446 = CARTESIAN_POINT ( 'NONE',  ( -5.637550801365594388, 3.675193018007246959, -1.088641768524161391 ) ) ;
#22447 = ORIENTED_EDGE ( 'NONE', *, *, #32311, .F. ) ;
#22448 = AXIS2_PLACEMENT_3D ( 'NONE', #25047, #20073, #12349 ) ;
#22449 = CARTESIAN_POINT ( 'NONE',  ( 7.249760686538667009, 0.000000000000000000, 0.000000000000000000 ) ) ;
#22450 = EDGE_CURVE ( 'NONE', #8590, #4825, #10181, .T. ) ;
#22451 = DIRECTION ( 'NONE',  ( -1.000000000000000000, 0.000000000000000000, -0.000000000000000000 ) ) ;
#22452 = ORIENTED_EDGE ( 'NONE', *, *, #1242, .T. ) ;
#22453 = FACE_OUTER_BOUND ( 'NONE', #8352, .T. ) ;
#22454 = EDGE_CURVE ( 'NONE', #1352, #9705, #23524, .T. ) ;
#22455 = VERTEX_POINT ( 'NONE', #30424 ) ;
#22456 = AXIS2_PLACEMENT_3D ( 'NONE', #3863, #19724, #6844 ) ;
#22457 = AXIS2_PLACEMENT_3D ( 'NONE', #27999, #12751, #7587 ) ;
#22458 = ORIENTED_EDGE ( 'NONE', *, *, #9139, .F. ) ;
#22459 = CARTESIAN_POINT ( 'NONE',  ( 3.249999999999999556, -1.699438267350438014, 9.241976615262153416 ) ) ;
#22461 = ORIENTED_EDGE ( 'NONE', *, *, #17368, .T. ) ;
#22460 = CARTESIAN_POINT ( 'NONE',  ( -3.135269660805080516, -0.5000000000000000000, 1.500000000000000000 ) ) ;
#22462 = VERTEX_POINT ( 'NONE', #7502 ) ;
#22463 = CARTESIAN_POINT ( 'NONE',  ( 23.42250000136559862, 1.913930629741522838, -2.363507492473150062 ) ) ;
#22464 = EDGE_CURVE ( 'NONE', #28731, #12480, #14451, .T. ) ;
#22465 = VERTEX_POINT ( 'NONE', #19909 ) ;
#22467 = AXIS2_PLACEMENT_3D ( 'NONE', #9530, #21915, #24270 ) ;
#22466 = CARTESIAN_POINT ( 'NONE',  ( 0.6791198108364584485, 8.522429291907643645, -3.345077512921565521 ) ) ;
#22469 = ORIENTED_EDGE ( 'NONE', *, *, #30040, .T. ) ;
#22468 = CARTESIAN_POINT ( 'NONE',  ( 18.96091535641603443, -3.614110606600299924, -2.184956778830001500 ) ) ;
#22470 = DIRECTION ( 'NONE',  ( 0.000000000000000000, 0.000000000000000000, 1.000000000000000000 ) ) ;
#22471 = CARTESIAN_POINT ( 'NONE',  ( 23.84310522038038727, -4.329614468550014195, -4.522129901861162260 ) ) ;
#22472 = CARTESIAN_POINT ( 'NONE',  ( 25.11000000136559507, -3.156283516753370044, -0.9349337715887220401 ) ) ;
#22473 = DIRECTION ( 'NONE',  ( 0.000000000000000000, 0.7071067811865455743, 0.7071067811865495711 ) ) ;
#22474 = EDGE_CURVE ( 'NONE', #974, #425, #8321, .T. ) ;
#22475 = PRODUCT_RELATED_PRODUCT_CATEGORY ( 'detail', '', ( #4694 ) ) ;
#22476 = AXIS2_PLACEMENT_3D ( 'NONE', #16306, #11291, #1436 ) ;
#22477 = CARTESIAN_POINT ( 'NONE',  ( 109.0524412912905774, 20.62920084672733267, -1.491740999229417941 ) ) ;
#22478 = CARTESIAN_POINT ( 'NONE',  ( -56.27770248097862549, 0.4996615022747108448, 1.500000000000000000 ) ) ;
#22479 = CARTESIAN_POINT ( 'NONE',  ( 0.7632845268398871230, 6.772677083992467928, -5.538577986808824960 ) ) ;
#22480 = AXIS2_PLACEMENT_3D ( 'NONE', #28343, #3609, #26996 ) ;
#22481 = VECTOR ( 'NONE', #12493, 1000.000000000000000 ) ;
#22482 = AXIS2_PLACEMENT_3D ( 'NONE', #32255, #16344, #19686 ) ;
#22483 = DIRECTION ( 'NONE',  ( -1.000000000000000000, -0.000000000000000000, 0.000000000000000000 ) ) ;
#22484 = CARTESIAN_POINT ( 'NONE',  ( 101.9216173105994159, -5.769792427975438898, 0.02339150517593241788 ) ) ;
#22485 = CARTESIAN_POINT ( 'NONE',  ( 10.00000000000000000, -4.787500056513357194, -1.476463073999686459 ) ) ;
#22486 = CARTESIAN_POINT ( 'NONE',  ( 3.063284526839887167, 0.000000000000000000, 0.000000000000000000 ) ) ;
#22487 = CONICAL_SURFACE ( 'NONE', #30494, 2.099999999999997868, 1.029744258676653867 ) ;
#22488 = CARTESIAN_POINT ( 'NONE',  ( 0.5032039771567776709, -2.299586922889600871, -9.456648240388242144 ) ) ;
#22489 = EDGE_CURVE ( 'NONE', #26613, #26504, #4902, .T. ) ;
#22490 = CARTESIAN_POINT ( 'NONE',  ( -3.500050802731187627, 2.853674364686379583, 1.549418761218565921 ) ) ;
#22491 = ORIENTED_EDGE ( 'NONE', *, *, #2022, .F. ) ;
#22492 = CARTESIAN_POINT ( 'NONE',  ( -3.550050800000000173, 3.113457007523260156, -0.9222479816126439855 ) ) ;
#22493 = VECTOR ( 'NONE', #5776, 1000.000000000000000 ) ;
#22494 = CARTESIAN_POINT ( 'NONE',  ( 56.97280603064898941, -277.2763395528616002, -1.500000000000000000 ) ) ;
#22495 = EDGE_CURVE ( 'NONE', #9325, #2615, #18731, .T. ) ;
#22496 = CARTESIAN_POINT ( 'NONE',  ( -4.350050800000000883, 3.113457007523260156, -0.9222479816126439855 ) ) ;
#22497 = ORIENTED_EDGE ( 'NONE', *, *, #14657, .F. ) ;
#22498 = DIRECTION ( 'NONE',  ( 0.000000000000000000, 0.7431448254773954654, -0.6691306063588569053 ) ) ;
#22499 = ORIENTED_EDGE ( 'NONE', *, *, #12186, .T. ) ;
#22500 = CARTESIAN_POINT ( 'NONE',  ( 15.94400161454247389, -16.27119544232739656, 1.500000000000836664 ) ) ;
#22501 = COORDINATED_UNIVERSAL_TIME_OFFSET ( 0, 0, .AHEAD. ) ;
#22502 = CIRCLE ( 'NONE', #30513, 8.749000000000002331 ) ;
#22503 = CARTESIAN_POINT ( 'NONE',  ( 7.249760686538667009, 7.906491560603665647, 3.748318449932320107 ) ) ;
#22504 = ORIENTED_EDGE ( 'NONE', *, *, #17263, .F. ) ;
#22505 = CARTESIAN_POINT ( 'NONE',  ( -3.686605011514858088, -10.77444884474583908, 1.500000000000001110 ) ) ;
#22506 = VECTOR ( 'NONE', #17615, 1000.000000000000000 ) ;
#22507 = EDGE_LOOP ( 'NONE', ( #9077, #17221, #20468 ) ) ;
#22508 = CARTESIAN_POINT ( 'NONE',  ( 3.499999999999999556, -3.573533178329542537, -5.126388750707260300 ) ) ;
#22509 = CARTESIAN_POINT ( 'NONE',  ( 18.76949126134281087, -5.753847806405374854, -4.155404940063082364 ) ) ;
#22510 = AXIS2_PLACEMENT_3D ( 'NONE', #18378, #28574, #16338 ) ;
#22511 = CARTESIAN_POINT ( 'NONE',  ( 0.000000000000000000, 8.475820894093034852, -4.057423117305301474 ) ) ;
#22512 = CARTESIAN_POINT ( 'NONE',  ( -10.00000000000000000, 0.000000000000000000, 0.000000000000000000 ) ) ;
#22513 = DIRECTION ( 'NONE',  ( -1.000000000000000000, 2.473959037481237219E-13, 0.000000000000000000 ) ) ;
#22514 = VECTOR ( 'NONE', #26055, 1000.000000000000114 ) ;
#22515 = CARTESIAN_POINT ( 'NONE',  ( 21.37037762942230046, -21.76140461385139702, -1.424884447122514164 ) ) ;
#22516 = DIRECTION ( 'NONE',  ( 4.917867153432985471E-17, 0.5735764363510441610, 0.8191520442889931308 ) ) ;
#22517 = VECTOR ( 'NONE', #21424, 1000.000000000000000 ) ;
#22518 = EDGE_CURVE ( 'NONE', #19457, #14763, #4327, .T. ) ;
#22519 = VECTOR ( 'NONE', #21532, 999.9999999999998863 ) ;
#22521 = VERTEX_POINT ( 'NONE', #29546 ) ;
#22520 = CARTESIAN_POINT ( 'NONE',  ( -3.362942409646513031, -5.022711880624455567E-15, 2.999999999999999556 ) ) ;
#22522 = CC_DESIGN_DATE_AND_TIME_ASSIGNMENT ( #28426, #30940, ( #6052 ) ) ;
#22523 = FACE_BOUND ( 'NONE', #27254, .T. ) ;
#22524 = CARTESIAN_POINT ( 'NONE',  ( -50.81000000000000227, -10.96999999999998643, 5.700000000000000178 ) ) ;
#22525 = CARTESIAN_POINT ( 'NONE',  ( 0.7212197595562634955, 0.5238431420063290878, -8.936767016196004221 ) ) ;
#22526 = CARTESIAN_POINT ( 'NONE',  ( -4.013969549054187630E-16, -4.681538312723522388, 0.8254815157535098091 ) ) ;
#22527 = CARTESIAN_POINT ( 'NONE',  ( -8.000050800000055418, 2.257600361463367289, 2.491616663310649127 ) ) ;
#22528 = DIRECTION ( 'NONE',  ( 1.000000000000000000, -0.000000000000000000, -0.000000000000000000 ) ) ;
#22529 = CARTESIAN_POINT ( 'NONE',  ( -56.32709181765920903, 0.0003929015865020345178, -1.038420530835418853 ) ) ;
#22530 = CARTESIAN_POINT ( 'NONE',  ( -34.48223484310472031, 0.5000000000000000000, -2.482234843104710986 ) ) ;
#22531 = ORIENTED_EDGE ( 'NONE', *, *, #20640, .T. ) ;
#22532 = VECTOR ( 'NONE', #29043, 1000.000000000000000 ) ;
#22533 = CARTESIAN_POINT ( 'NONE',  ( -7.962550801365594566, 2.752080473201636845, -2.228590825266444142 ) ) ;
#22534 = VERTEX_POINT ( 'NONE', #27026 ) ;
#22535 = EDGE_CURVE ( 'NONE', #1082, #7709, #29931, .T. ) ;
#22536 = AXIS2_PLACEMENT_3D ( 'NONE', #7161, #14485, #27547 ) ;
#22537 = CIRCLE ( 'NONE', #25737, 5.010000000000000675 ) ;
#22538 = CARTESIAN_POINT ( 'NONE',  ( -7.204531657079157547, -2.325406398514293205, 1.883076972206379818 ) ) ;
#22539 = LINE ( 'NONE', #19381, #7675 ) ;
#22540 = CIRCLE ( 'NONE', #19872, 1.800000000000017142 ) ;
#22541 = ADVANCED_FACE ( 'NONE', ( #32722 ), #31018, .T. ) ;
#22542 = CARTESIAN_POINT ( 'NONE',  ( 102.8580990270160385, -4.820463887425400884, -4.522129901861164036 ) ) ;
#22543 = CARTESIAN_POINT ( 'NONE',  ( 5.133822020161873390, -13.02681593462403242, 1.756567112590995183 ) ) ;
#22544 = LINE ( 'NONE', #25385, #4460 ) ;
#22545 = VECTOR ( 'NONE', #12679, 1000.000000000000227 ) ;
#22546 = ORIENTED_EDGE ( 'NONE', *, *, #15469, .F. ) ;
#22547 = CARTESIAN_POINT ( 'NONE',  ( 3.063284526839887167, 0.000000000000000000, 0.000000000000000000 ) ) ;
#22548 = AXIS2_PLACEMENT_3D ( 'NONE', #22459, #24809, #14608 ) ;
#22549 = VERTEX_POINT ( 'NONE', #1798 ) ;
#22550 = CARTESIAN_POINT ( 'NONE',  ( -3.712942406915326288, 4.884725290497410777E-15, -2.999999999999999556 ) ) ;
#22551 = MECHANICAL_CONTEXT ( 'NONE', #9686, 'mechanical' ) ;
#22552 = CARTESIAN_POINT ( 'NONE',  ( 54.97713542672909171, -6.503351899782645162, 3.998506278707449457 ) ) ;
#22553 = LINE ( 'NONE', #25220, #11747 ) ;
#22554 = CIRCLE ( 'NONE', #2277, 7.482234843104714983 ) ;
#22556 = DIRECTION ( 'NONE',  ( 1.000000000000000000, -0.000000000000000000, -0.000000000000000000 ) ) ;
#22555 = CARTESIAN_POINT ( 'NONE',  ( 108.9281229201717736, 17.68884002061582450, -5.233955718285084657 ) ) ;
#22557 = CIRCLE ( 'NONE', #20934, 296.4345239564032113 ) ;
#22558 = ORIENTED_EDGE ( 'NONE', *, *, #30763, .F. ) ;
#22559 = CIRCLE ( 'NONE', #12931, 2.999999999999999112 ) ;
#22560 = CARTESIAN_POINT ( 'NONE',  ( -8.000050800000002127, -2.133806103461856729, -2.113321545700467041 ) ) ;
#22561 = CARTESIAN_POINT ( 'NONE',  ( -3.529825581556942343E-16, -4.116875700062099241, 2.376879293651050329 ) ) ;
#22562 = AXIS2_PLACEMENT_3D ( 'NONE', #24115, #11930, #29812 ) ;
#22563 = CARTESIAN_POINT ( 'NONE',  ( 24.98500000136559507, -0.9349337715887248157, 3.156283516753367824 ) ) ;
#22564 = AXIS2_PLACEMENT_3D ( 'NONE', #25840, #15626, #28163 ) ;
#22565 = CARTESIAN_POINT ( 'NONE',  ( 5.414747269551301478, -13.03415141497022489, -1.499999999999435785 ) ) ;
#22567 = ORIENTED_EDGE ( 'NONE', *, *, #28904, .T. ) ;
#22566 = CARTESIAN_POINT ( 'NONE',  ( 107.6996442589674103, 19.35565155597529596, 4.629213727441584325 ) ) ;
#22568 = CARTESIAN_POINT ( 'NONE',  ( -8.012550801365593500, 1.828967928396027176, -3.368539882008727115 ) ) ;
#22569 = FACE_OUTER_BOUND ( 'NONE', #5153, .T. ) ;
#22570 = AXIS2_PLACEMENT_3D ( 'NONE', #2047, #17261, #30301 ) ;
#22571 = CARTESIAN_POINT ( 'NONE',  ( -50.81000000000000227, -10.96999999999998643, 1.500000000000000000 ) ) ;
#22572 = DIRECTION ( 'NONE',  ( 0.000000000000000000, -0.9063077870366467170, -0.4226182617407064912 ) ) ;
#22573 = CIRCLE ( 'NONE', #13454, 8.500000000000000000 ) ;
#22574 = VERTEX_POINT ( 'NONE', #4624 ) ;
#22576 = ORIENTED_EDGE ( 'NONE', *, *, #41, .F. ) ;
#22575 = CARTESIAN_POINT ( 'NONE',  ( 23.03407491561165443, -17.39674082715752945, 1.686926596850292670 ) ) ;
#22577 = CIRCLE ( 'NONE', #19912, 0.9999999999999991118 ) ;
#22578 = DIRECTION ( 'NONE',  ( 0.000000000000000000, 0.000000000000000000, -1.000000000000000000 ) ) ;
#22579 = DIRECTION ( 'NONE',  ( 0.000000000000000000, 1.000000000000000000, 0.000000000000000000 ) ) ;
#22580 = CARTESIAN_POINT ( 'NONE',  ( -47.25352234179201361, 16.22999999999998266, 1.050000000000000044 ) ) ;
#22581 = EDGE_CURVE ( 'NONE', #8190, #21952, #9091, .T. ) ;
#22582 = CARTESIAN_POINT ( 'NONE',  ( -22.65704777669159498, 18.60133783399176011, 1.500000000000506040 ) ) ;
#22583 = ADVANCED_FACE ( 'NONE', ( #24997 ), #19343, .T. ) ;
#22584 = CARTESIAN_POINT ( 'NONE',  ( 102.2656009641822692, -1.731193774301682531, 2.184956770134436788 ) ) ;
#22585 = CARTESIAN_POINT ( 'NONE',  ( -2.351824853402081583, -12.55082504084320227, -1.499999999999879430 ) ) ;
#22586 = AXIS2_PLACEMENT_3D ( 'NONE', #10799, #28689, #2802 ) ;
#22587 = CARTESIAN_POINT ( 'NONE',  ( 24.98499999999999943, 2.486304738420679783, -0.2613211581691337604 ) ) ;
#22588 = VECTOR ( 'NONE', #720, 1000.000000000000000 ) ;
#22589 = AXIS2_PLACEMENT_3D ( 'NONE', #32454, #32798, #24752 ) ;
#22590 = CARTESIAN_POINT ( 'NONE',  ( 35.34214449211034292, -3.792788106923193236, 0.4367666027768959958 ) ) ;
#22591 = CARTESIAN_POINT ( 'NONE',  ( 107.4168514414663491, -16.88233545631764798, 3.542414872601526543 ) ) ;
#22592 = ORIENTED_EDGE ( 'NONE', *, *, #27003, .T. ) ;
#22593 = CARTESIAN_POINT ( 'NONE',  ( 3.499999999999999556, 0.000000000000000000, 0.000000000000000000 ) ) ;
#22594 = CIRCLE ( 'NONE', #10814, 7.318435636271054534 ) ;
#22595 = CIRCLE ( 'NONE', #1237, 0.4499999999999997335 ) ;
#22596 = PERSON_AND_ORGANIZATION ( #6766, #25292 ) ;
#22598 = CARTESIAN_POINT ( 'NONE',  ( 2.589202944057212186, 6.846250362091623742, -7.715757980413485484 ) ) ;
#22597 = CIRCLE ( 'NONE', #14559, 10.94895958125474245 ) ;
#22599 = ORIENTED_EDGE ( 'NONE', *, *, #1843, .F. ) ;
#22600 = CARTESIAN_POINT ( 'NONE',  ( 107.9956158609837047, 18.15374730895081257, -5.039121240573448013 ) ) ;
#22601 = VERTEX_POINT ( 'NONE', #32545 ) ;
#22602 = CARTESIAN_POINT ( 'NONE',  ( 2.274274201625327230, -1.975651141462315907, 10.82112760146735475 ) ) ;
#22604 = VERTEX_POINT ( 'NONE', #27175 ) ;
#22603 = CARTESIAN_POINT ( 'NONE',  ( 40.87784222422364877, -5.768774535592546826, -4.023789691760647713 ) ) ;
#22605 = ORIENTED_EDGE ( 'NONE', *, *, #4072, .F. ) ;
#22606 = CYLINDRICAL_SURFACE ( 'NONE', #31120, 0.5000000000000002220 ) ;
#22607 = CARTESIAN_POINT ( 'NONE',  ( 85.13613392229180477, -2.069934983084473767, 2.713652344655541615 ) ) ;
#22609 = VERTEX_POINT ( 'NONE', #14148 ) ;
#22608 = CARTESIAN_POINT ( 'NONE',  ( 22.48500000273118715, 0.2613211581691317065, 2.486304738420681559 ) ) ;
#22610 = VECTOR ( 'NONE', #7105, 1000.000000000000000 ) ;
#22611 = CARTESIAN_POINT ( 'NONE',  ( 21.09752163291441818, 16.24116299994017609, -1.050000000000000044 ) ) ;
#22612 = CARTESIAN_POINT ( 'NONE',  ( 0.1610798642962855409, -10.72944008624798506, 4.522129901861156931 ) ) ;
#22613 =( BOUNDED_CURVE ( )  B_SPLINE_CURVE ( 2, ( #8455, #21020, #18009, #12988, #8307, #28845, #23202, #3295, #13462, #611, #18648 ),
 .UNSPECIFIED., .F., .F. ) 
 B_SPLINE_CURVE_WITH_KNOTS ( ( 3, 2, 2, 2, 2, 3 ),
 ( 0.1228822619934377414, 0.1250000000000000000, 0.1406250000000000000, 0.1562500000000000000, 0.1718750000000000000, 0.1853822619934377414 ),
 .UNSPECIFIED. ) 
 CURVE ( )  GEOMETRIC_REPRESENTATION_ITEM ( )  RATIONAL_B_SPLINE_CURVE ( ( 0.9821626249036861100, 0.9896829947469993893, 1.000000000000000000, 0.9238795325112867385, 1.000000000000000000, 0.9238795325112867385, 1.000000000000000000, 0.9238795325112867385, 1.000000000000000000, 0.9341965377642873491, 0.9821626249036861100 ) ) 
 REPRESENTATION_ITEM ( '' )  );
#22614 = VECTOR ( 'NONE', #28559, 1000.000000000000000 ) ;
#22615 = DIRECTION ( 'NONE',  ( 0.000000000000000000, 0.000000000000000000, -1.000000000000000000 ) ) ;
#22616 = CARTESIAN_POINT ( 'NONE',  ( 8.706508905304815471, -1.271749511658105902, -1.000000000000000000 ) ) ;
#22618 = VERTEX_POINT ( 'NONE', #9613 ) ;
#22617 = CARTESIAN_POINT ( 'NONE',  ( 107.5625329803365702, -18.99455126352175682, -4.492206011592212889 ) ) ;
#22619 = LINE ( 'NONE', #32157, #18365 ) ;
#22620 = AXIS2_PLACEMENT_3D ( 'NONE', #31922, #29741, #19384 ) ;
#22621 = CIRCLE ( 'NONE', #8203, 0.4999999999999996669 ) ;
#22622 = EDGE_CURVE ( 'NONE', #3542, #12771, #32232, .T. ) ;
#22623 = FACE_OUTER_BOUND ( 'NONE', #19177, .T. ) ;
#22624 = CARTESIAN_POINT ( 'NONE',  ( 24.04750000136559507, -3.024605502323851169, 0.3178988483021052969 ) ) ;
#22625 = CC_DESIGN_APPROVAL ( #17193, ( #23132 ) ) ;
#22626 = CARTESIAN_POINT ( 'NONE',  ( 107.5416032035946898, 18.44933160811492101, -5.131841438779300546 ) ) ;
#22627 = CYLINDRICAL_SURFACE ( 'NONE', #2225, 2.999999999999999112 ) ;
#22628 = CARTESIAN_POINT ( 'NONE',  ( 8.930755659325139817, 0.4999999999999982792, -1.050000000000000044 ) ) ;
#22629 = ORIENTED_EDGE ( 'NONE', *, *, #17868, .T. ) ;
#22630 = CARTESIAN_POINT ( 'NONE',  ( -1.444447458290426890E-30, -1.659765939693074585E-14, 4.753758587302147731 ) ) ;
#22631 = ADVANCED_FACE ( 'NONE', ( #19514 ), #22182, .F. ) ;
#22632 = CARTESIAN_POINT ( 'NONE',  ( 101.6022419886208610, -1.170867242066747860, -0.07017451552781628354 ) ) ;
#22633 = CARTESIAN_POINT ( 'NONE',  ( -7.187550801365593323, 3.521866450007987037, 0.3701630799359328372 ) ) ;
#22634 = VERTEX_POINT ( 'NONE', #22503 ) ;
#22635 = AXIS2_PLACEMENT_3D ( 'NONE', #24509, #32256, #13989 ) ;
#22636 = AXIS2_PLACEMENT_3D ( 'NONE', #477, #10659, #21054 ) ;
#22637 = PLANE ( 'NONE',  #26868 ) ;
#22638 = DIRECTION ( 'NONE',  ( 0.000000000000000000, 0.000000000000000000, 1.000000000000000000 ) ) ;
#22639 = EDGE_CURVE ( 'NONE', #23130, #12973, #5939, .T. ) ;
#22640 = DIRECTION ( 'NONE',  ( 1.000000000000000000, -0.000000000000000000, -0.000000000000000000 ) ) ;
#22642 = ORIENTED_EDGE ( 'NONE', *, *, #32853, .T. ) ;
#22641 = AXIS2_PLACEMENT_3D ( 'NONE', #16427, #3743, #21634 ) ;
#22643 = PLANE ( 'NONE',  #3321 ) ;
#22644 = ORIENTED_EDGE ( 'NONE', *, *, #32340, .T. ) ;
#22645 = AXIS2_PLACEMENT_3D ( 'NONE', #13603, #11440, #31841 ) ;
#22646 = CARTESIAN_POINT ( 'NONE',  ( 5.865515302491369987, 15.00000000000000178, 1.508259000770582059 ) ) ;
#22647 = ORIENTED_EDGE ( 'NONE', *, *, #11439, .T. ) ;
#22648 = CARTESIAN_POINT ( 'NONE',  ( -3.135269660805080516, -0.4999999999999993339, 1.500000000000000000 ) ) ;
#22650 = ORIENTED_EDGE ( 'NONE', *, *, #24287, .F. ) ;
#22649 = LINE ( 'NONE', #23139, #17045 ) ;
#22651 = EDGE_CURVE ( 'NONE', #4862, #19637, #1362, .T. ) ;
#22652 = VERTEX_POINT ( 'NONE', #10171 ) ;
#22653 = DIRECTION ( 'NONE',  ( -1.000000000000000000, 8.574039729943018344E-17, -0.000000000000000000 ) ) ;
#22654 = APPROVAL_PERSON_ORGANIZATION ( #24845, #30093, #9450 ) ;
#22655 = ORIENTED_EDGE ( 'NONE', *, *, #29337, .F. ) ;
#22656 = DIRECTION ( 'NONE',  ( 1.000000000000000000, -0.000000000000000000, -0.000000000000000000 ) ) ;
#22658 = EDGE_LOOP ( 'NONE', ( #11649, #22989, #1350, #18625, #10537 ) ) ;
#22657 = CARTESIAN_POINT ( 'NONE',  ( 0.2678094507063553675, -7.640026513854723866, 1.500000000000000000 ) ) ;
#22659 = CARTESIAN_POINT ( 'NONE',  ( -3.122314033877883927E-16, -3.641590349731949505, 3.055657119358789142 ) ) ;
#22660 = EDGE_CURVE ( 'NONE', #10072, #481, #20572, .T. ) ;
#22661 = LINE ( 'NONE', #7103, #19744 ) ;
#22662 = DIRECTION ( 'NONE',  ( -0.000000000000000000, -0.000000000000000000, 1.000000000000000000 ) ) ;
#22663 = CIRCLE ( 'NONE', #7191, 8.500000000000000000 ) ;
#22664 = CARTESIAN_POINT ( 'NONE',  ( 56.97280603064898941, -277.2763395528616002, 4.621439243524390506 ) ) ;
#22665 = DIRECTION ( 'NONE',  ( -0.9896144216807905014, -0.000000000000000000, -0.1437473352845004826 ) ) ;
#22666 = CARTESIAN_POINT ( 'NONE',  ( 24.57728726453536439, -17.46986644505820152, 1.411007141444847512 ) ) ;
#22667 = EDGE_CURVE ( 'NONE', #24091, #8502, #18206, .T. ) ;
#22668 = ADVANCED_FACE ( 'NONE', ( #20392 ), #2167, .F. ) ;
#22669 = CARTESIAN_POINT ( 'NONE',  ( 2.866494652514124830, 9.241976615262203154, 2.300561732649596181 ) ) ;
#22670 = DIRECTION ( 'NONE',  ( -1.000000000000000000, 0.000000000000000000, -0.000000000000000000 ) ) ;
#22671 = DIRECTION ( 'NONE',  ( -1.000000000000000000, 0.000000000000000000, 0.000000000000000000 ) ) ;
#22672 = CARTESIAN_POINT ( 'NONE',  ( 20.48500000273118715, 0.2613211581691317065, 2.486304738420681559 ) ) ;
#22673 = CC_DESIGN_SECURITY_CLASSIFICATION ( #25875, ( #33104 ) ) ;
#22674 = DIRECTION ( 'NONE',  ( 0.000000000000000000, 0.000000000000000000, -1.000000000000000000 ) ) ;
#22675 = CARTESIAN_POINT ( 'NONE',  ( -3.350050802731187272, -0.3135853898029607456, 2.983565686104819648 ) ) ;
#22676 = ORIENTED_EDGE ( 'NONE', *, *, #12498, .F. ) ;
#22677 = CARTESIAN_POINT ( 'NONE',  ( -4.050050800000001061, -1.549418761218565477, 2.853674364686380471 ) ) ;
#22678 = LINE ( 'NONE', #15135, #9251 ) ;
#22679 = DIRECTION ( 'NONE',  ( 0.000000000000000000, 0.000000000000000000, -1.000000000000000000 ) ) ;
#22680 = ORIENTED_EDGE ( 'NONE', *, *, #12830, .T. ) ;
#22681 = DIRECTION ( 'NONE',  ( 0.000000000000000000, -0.000000000000000000, -1.000000000000000000 ) ) ;
#22682 = CARTESIAN_POINT ( 'NONE',  ( 7.249760686538667009, 7.530955069117513112, 2.741043480754951744 ) ) ;
#22683 = CARTESIAN_POINT ( 'NONE',  ( 107.9829200570041507, -17.82341518643319489, 4.417814765846281411 ) ) ;
#22684 = ADVANCED_FACE ( 'NONE', ( #27728 ), #7850, .T. ) ;
#22685 = ORIENTED_EDGE ( 'NONE', *, *, #12617, .T. ) ;
#22686 = CARTESIAN_POINT ( 'NONE',  ( 21.08401840680260264, -16.78474387324011374, 1.500000000000000666 ) ) ;
#22687 = APPROVAL_DATE_TIME ( #25167, #15523 ) ;
#22688 = CARTESIAN_POINT ( 'NONE',  ( 17.97422212134408781, -19.86246923125032282, -4.522129901861166701 ) ) ;
#22689 = ORIENTED_EDGE ( 'NONE', *, *, #31794, .F. ) ;
#22690 = CARTESIAN_POINT ( 'NONE',  ( -4.555596785357748146, -6.492743774806009505, 1.500000000000000000 ) ) ;
#22691 = VERTEX_POINT ( 'NONE', #15017 ) ;
#22692 = CARTESIAN_POINT ( 'NONE',  ( 108.0241601323609615, -18.41726201233227300, -4.475732320008884102 ) ) ;
#22694 = EDGE_LOOP ( 'NONE', ( #7879, #7254, #9163, #19792, #13596 ) ) ;
#22693 = FACE_OUTER_BOUND ( 'NONE', #24249, .T. ) ;
#22695 = CARTESIAN_POINT ( 'NONE',  ( 6.883866482134012976, -2.190971798910002377, 8.452201317944597392 ) ) ;
#22696 = DIRECTION ( 'NONE',  ( 0.000000000000000000, 0.000000000000000000, 1.000000000000000000 ) ) ;
#22697 = EDGE_CURVE ( 'NONE', #17091, #4235, #20075, .T. ) ;
#22698 = CARTESIAN_POINT ( 'NONE',  ( 21.38916691622168997, -21.75742400528990927, -1.437540121018670902 ) ) ;
#22699 = DIRECTION ( 'NONE',  ( -4.917867153432941097E-17, -0.5735764363510392760, -0.8191520442889965725 ) ) ;
#22700 = EDGE_LOOP ( 'NONE', ( #11846, #25893, #16063, #19659 ) ) ;
#22701 = DIRECTION ( 'NONE',  ( -0.8616149568369075862, 0.5075624751249188105, 0.000000000000000000 ) ) ;
#22702 = CARTESIAN_POINT ( 'NONE',  ( 107.3084118612033677, 16.37966538140715400, -1.491489915294727187 ) ) ;
#22703 = DIRECTION ( 'NONE',  ( 1.000000000000000000, 0.000000000000000000, -0.000000000000000000 ) ) ;
#22704 = CARTESIAN_POINT ( 'NONE',  ( 0.000000000000000000, 19.51744974835125035, 0.000000000000000000 ) ) ;
#22705 = EDGE_CURVE ( 'NONE', #22534, #14366, #25203, .T. ) ;
#22706 = EDGE_CURVE ( 'NONE', #25887, #31320, #2669, .T. ) ;
#22707 = DIRECTION ( 'NONE',  ( 1.000000000000000000, 0.000000000000000000, 0.000000000000000000 ) ) ;
#22708 = CARTESIAN_POINT ( 'NONE',  ( -7.350050802731187716, -0.3135853898029607456, 2.983565686104819648 ) ) ;
#22709 = CARTESIAN_POINT ( 'NONE',  ( -56.55463451115983986, 0.05299951999074122705, -1.274799463869835447 ) ) ;
#22710 = CARTESIAN_POINT ( 'NONE',  ( 34.50091246256899780, -0.01740729335041252962, 3.000607876078799752 ) ) ;
#22711 = ORIENTED_EDGE ( 'NONE', *, *, #19200, .F. ) ;
#22712 = CARTESIAN_POINT ( 'NONE',  ( -6.412550801365592967, 1.828967928396027176, -3.368539882008727115 ) ) ;
#22713 = ORIENTED_EDGE ( 'NONE', *, *, #14313, .F. ) ;
#22714 = CARTESIAN_POINT ( 'NONE',  ( -6.754531657079159146, 3.105402419394639235, -0.9198621039125850496 ) ) ;
#22715 = CARTESIAN_POINT ( 'NONE',  ( 25.29750000136559507, -2.363507492473152283, -1.913930629741525280 ) ) ;
#22716 = CARTESIAN_POINT ( 'NONE',  ( -10.00000000000000000, 0.000000000000000000, 0.000000000000000000 ) ) ;
#22717 = ORIENTED_EDGE ( 'NONE', *, *, #29044, .T. ) ;
#22718 = LINE ( 'NONE', #32923, #25767 ) ;
#22719 = EDGE_CURVE ( 'NONE', #1670, #19072, #2517, .T. ) ;
#22720 = CC_DESIGN_DATE_AND_TIME_ASSIGNMENT ( #23366, #13490, ( #25774 ) ) ;
#22721 = B_SPLINE_CURVE_WITH_KNOTS ( 'NONE', 3,
 ( #22460, #2580, #32677, #25125, #7581, #10424, #15101, #18101, #27643, #17954 ),
 .UNSPECIFIED., .F., .F.,
 ( 4, 2, 2, 2, 4 ),
 ( 0.000000000000000000, 0.0002246264387293540486, 0.0004492528774587080972, 0.0006738793161880621187, 0.0008985057549174161945 ),
 .UNSPECIFIED. ) ;
#22722 = ORIENTED_EDGE ( 'NONE', *, *, #25340, .F. ) ;
#22723 = CARTESIAN_POINT ( 'NONE',  ( 3.063284526839890720, 5.538577986808988385, -6.772677083992317826 ) ) ;
#22724 = PERSON_AND_ORGANIZATION_ROLE ( 'creator' ) ;
#22725 = CARTESIAN_POINT ( 'NONE',  ( 69.07025633558752986, -6.112492629244566267, 3.999774175338361104 ) ) ;
#22726 = CARTESIAN_POINT ( 'NONE',  ( 10.55147673363119232, -2.718385644597145046, -4.208382051008221048 ) ) ;
#22728 = CARTESIAN_POINT ( 'NONE',  ( 4.749760686538667009, 7.892520144992453801, -1.391664247347147443 ) ) ;
#22727 = CARTESIAN_POINT ( 'NONE',  ( 108.9099939952607627, 17.58789101337935179, -5.127064440218127572 ) ) ;
#22729 = VERTEX_POINT ( 'NONE', #25407 ) ;
#22730 = CARTESIAN_POINT ( 'NONE',  ( -7.650050802731187538, 2.331437884370912705, -1.887961173149511618 ) ) ;
#22731 = DIRECTION ( 'NONE',  ( -0.000000000000000000, -0.000000000000000000, -1.000000000000000000 ) ) ;
#22732 = EDGE_CURVE ( 'NONE', #29863, #26510, #30609, .T. ) ;
#22733 = CARTESIAN_POINT ( 'NONE',  ( 23.17250000136559862, -3.024605502323851169, 0.3178988483021052969 ) ) ;
#22734 = CARTESIAN_POINT ( 'NONE',  ( 4.749760686538667009, -7.892520144992443143, 1.391664247347202288 ) ) ;
#22736 = VERTEX_POINT ( 'NONE', #12188 ) ;
#22735 = CARTESIAN_POINT ( 'NONE',  ( 0.9306419922191575544, -8.901511148765193226, 0.9788672205888330202 ) ) ;
#22737 = CARTESIAN_POINT ( 'NONE',  ( -6.212550801365593678, 3.368539882008727115, 1.828967928396026954 ) ) ;
#22738 = DIRECTION ( 'NONE',  ( 0.000000000000000000, -0.2588190451025310090, 0.9659258262890655367 ) ) ;
#22739 = CARTESIAN_POINT ( 'NONE',  ( -53.79666904180695042, 5.504338532704765363, 1.390325731058407399 ) ) ;
#22740 = CARTESIAN_POINT ( 'NONE',  ( 22.17250000000000298, 1.291182301015469047, 2.378061970571981654 ) ) ;
#22741 = ORIENTED_EDGE ( 'NONE', *, *, #15093, .F. ) ;
#22743 = ORIENTED_EDGE ( 'NONE', *, *, #20292, .F. ) ;
#22742 = CARTESIAN_POINT ( 'NONE',  ( 23.88966202700896702, -17.43474874481661985, 1.573876621502935613 ) ) ;
#22744 = CARTESIAN_POINT ( 'NONE',  ( -2.124956573341760357, 1.323625320507108460, 3.284597389080124774 ) ) ;
#22745 = CARTESIAN_POINT ( 'NONE',  ( 3.020080166740162664, -8.666653390676570368, -2.264483761671786333 ) ) ;
#22746 = CARTESIAN_POINT ( 'NONE',  ( 10.52034268205830259, 3.641590349731929077, 3.055657119358814011 ) ) ;
#22747 = CARTESIAN_POINT ( 'NONE',  ( 68.95673039201351173, -3.844717801506668753, 2.184957270214452407 ) ) ;
#22748 = CARTESIAN_POINT ( 'NONE',  ( 0.4357215767673975892, -15.33303754249009287, -1.500000000000119238 ) ) ;
#22749 = LINE ( 'NONE', #12545, #14018 ) ;
#22750 = CARTESIAN_POINT ( 'NONE',  ( 1.624999999999999778, -5.222868219166924675, 9.680994141368755024 ) ) ;
#22751 = CARTESIAN_POINT ( 'NONE',  ( 23.61632761762314203, -8.296864917633476111, 2.713652344655544724 ) ) ;
#22752 = VERTEX_POINT ( 'NONE', #19905 ) ;
#22753 = CARTESIAN_POINT ( 'NONE',  ( 25.23500000000000654, 2.486304733690583912, -0.2613212031729839624 ) ) ;
#22754 = ADVANCED_FACE ( 'NONE', ( #7195, #4837, #32944, #30422 ), #17890, .F. ) ;
#22755 = CARTESIAN_POINT ( 'NONE',  ( 2.274274201625327230, -10.82112760146734765, -1.975651141462354543 ) ) ;
#22756 = ORIENTED_EDGE ( 'NONE', *, *, #8415, .F. ) ;
#22757 = CARTESIAN_POINT ( 'NONE',  ( 107.5053003840741184, 18.24082670017404340, -5.040895989151252365 ) ) ;
#22758 = ORIENTED_EDGE ( 'NONE', *, *, #17710, .T. ) ;
#22759 = CARTESIAN_POINT ( 'NONE',  ( -18.19731407151451918, 15.53049510967715463, 1.844195982360324226 ) ) ;
#22761 = ORIENTED_EDGE ( 'NONE', *, *, #21253, .F. ) ;
#22760 = CARTESIAN_POINT ( 'NONE',  ( 28.69347568615663491, -5.620564795450311735, -4.001040682695108153 ) ) ;
#22762 = VERTEX_POINT ( 'NONE', #7499 ) ;
#22763 = ADVANCED_FACE ( 'NONE', ( #28082 ), #8917, .F. ) ;
#22764 = CARTESIAN_POINT ( 'NONE',  ( -2.600000000000000089, 0.000000000000000000, 1.500000000000000000 ) ) ;
#22765 = CARTESIAN_POINT ( 'NONE',  ( -7.062550801365593323, 3.521866450007987037, 0.3701630799359328372 ) ) ;
#22766 = EDGE_CURVE ( 'NONE', #12596, #25887, #31264, .T. ) ;
#22767 = CARTESIAN_POINT ( 'NONE',  ( -34.71233008869360503, 0.000000000000000000, 1.019564728980889567 ) ) ;
#22768 = CARTESIAN_POINT ( 'NONE',  ( 107.5617944031221640, -18.98359742639815551, -4.522129901861166701 ) ) ;
#22770 = ORIENTED_EDGE ( 'NONE', *, *, #30617, .F. ) ;
#22769 = DIRECTION ( 'NONE',  ( -1.000000000000000000, 0.000000000000000000, 0.000000000000000000 ) ) ;
#22771 = CARTESIAN_POINT ( 'NONE',  ( 22.66400097956248061, 17.80079245417792322, -1.500000000000000000 ) ) ;
#22772 = CARTESIAN_POINT ( 'NONE',  ( -1.047937531484013585, -4.989690239015236450, 4.522129901861156931 ) ) ;
#22773 = EDGE_CURVE ( 'NONE', #2513, #10376, #31570, .T. ) ;
#22774 = CARTESIAN_POINT ( 'NONE',  ( -3.000233502159942667, -11.27265617876589054, 1.743644579621235202 ) ) ;
#22775 = CARTESIAN_POINT ( 'NONE',  ( 8.706508904963998319, -1.271749511501821583, -1.500000000000000000 ) ) ;
#22777 = VERTEX_POINT ( 'NONE', #8003 ) ;
#22776 = CARTESIAN_POINT ( 'NONE',  ( -12.44989959798873791, 18.00000000000000355, -12.99999999999999645 ) ) ;
#22778 = LINE ( 'NONE', #17752, #29053 ) ;
#22779 = B_SPLINE_CURVE_WITH_KNOTS ( 'NONE', 3,
 ( #23317, #26328, #1060, #8275, #419, #21143, #13419, #571, #18468, #16094 ),
 .UNSPECIFIED., .F., .F.,
 ( 4, 2, 2, 2, 4 ),
 ( 2.493548413911061648E-07, 0.0005478513795029415741, 0.001095453404164492160, 0.001643055428826042637, 0.002190657453487592898 ),
 .UNSPECIFIED. ) ;
#22780 = DIRECTION ( 'NONE',  ( 0.000000000000000000, -0.5735764363510496011, -0.8191520442889893561 ) ) ;
#22781 = CARTESIAN_POINT ( 'NONE',  ( 10.00000000000000178, -8.574039729943018837E-16, 0.000000000000000000 ) ) ;
#22782 = LINE ( 'NONE', #2220, #19308 ) ;
#22783 = CARTESIAN_POINT ( 'NONE',  ( -2.767073886773233848, -0.6621507858625382825, -1.748408842879326075 ) ) ;
#22784 = ORIENTED_EDGE ( 'NONE', *, *, #29343, .T. ) ;
#22785 = CARTESIAN_POINT ( 'NONE',  ( 109.0524412912905774, 20.62920084672733267, 1.508259000770582059 ) ) ;
#22786 = DIRECTION ( 'NONE',  ( -0.000000000000000000, -0.000000000000000000, -1.000000000000000000 ) ) ;
#22787 = CARTESIAN_POINT ( 'NONE',  ( -5.787550801365593856, 0.3701630799359330593, -3.521866450007987037 ) ) ;
#22788 = EDGE_LOOP ( 'NONE', ( #18061, #26718, #28968, #19172 ) ) ;
#22789 = CARTESIAN_POINT ( 'NONE',  ( 2.037945749704312686E-16, 2.376879293651064540, 4.116875700062091248 ) ) ;
#22790 = DIRECTION ( 'NONE',  ( 0.000000000000000000, -0.9945218953682744001, 0.1045284632676437286 ) ) ;
#22791 = CARTESIAN_POINT ( 'NONE',  ( 3.499999999999999556, -3.573533178329542537, -5.126388750707260300 ) ) ;
#22792 = ORIENTED_EDGE ( 'NONE', *, *, #26490, .T. ) ;
#22793 = CARTESIAN_POINT ( 'NONE',  ( -2.506063600758156262, 0.4999999999999998890, 1.500000000000000000 ) ) ;
#22794 = ORIENTED_EDGE ( 'NONE', *, *, #25534, .F. ) ;
#22795 = EDGE_CURVE ( 'NONE', #32499, #593, #14460, .T. ) ;
#22796 = CARTESIAN_POINT ( 'NONE',  ( 4.749760686538667009, 8.014274990069656823, -8.669741416787380218E-17 ) ) ;
#22797 = VERTEX_POINT ( 'NONE', #25733 ) ;
#22798 = CARTESIAN_POINT ( 'NONE',  ( -2.962625823238651979, -0.001292792641227542925, 0.8472062597617511237 ) ) ;
#22800 = ORIENTED_EDGE ( 'NONE', *, *, #18352, .F. ) ;
#22799 = DIRECTION ( 'NONE',  ( 0.000000000000000000, 0.000000000000000000, 1.000000000000000000 ) ) ;
#22801 = ORIENTED_EDGE ( 'NONE', *, *, #17139, .T. ) ;
#22802 = CARTESIAN_POINT ( 'NONE',  ( 6.524595551582241804, -4.857153507487898203, -7.168326838404991186 ) ) ;
#22803 = ORIENTED_EDGE ( 'NONE', *, *, #13979, .T. ) ;
#22804 = CARTESIAN_POINT ( 'NONE',  ( 0.000000000000000000, -1.999317321091575561, 10.76487093102064030 ) ) ;
#22806 = ORIENTED_EDGE ( 'NONE', *, *, #2575, .T. ) ;
#22805 = CARTESIAN_POINT ( 'NONE',  ( 2.600000000000000089, 0.000000000000000000, -1.500000000000000000 ) ) ;
#22807 = CARTESIAN_POINT ( 'NONE',  ( 1.630591573041451303, -1.447622518949628123, -1.758800530465949752 ) ) ;
#22808 = DIRECTION ( 'NONE',  ( 1.000000000000000000, 0.000000000000000000, 0.000000000000000000 ) ) ;
#22809 = CARTESIAN_POINT ( 'NONE',  ( 3.250000000000001332, 0.000000000000000000, 0.000000000000000000 ) ) ;
#22810 = FACE_OUTER_BOUND ( 'NONE', #30769, .T. ) ;
#22811 = CARTESIAN_POINT ( 'NONE',  ( 78.40736801748178664, 24.56822898102832653, -4.612695725900422872 ) ) ;
#22812 = CARTESIAN_POINT ( 'NONE',  ( -23.35000000000000142, -10.96966150227469505, -11.50000000000000000 ) ) ;
#22813 = CARTESIAN_POINT ( 'NONE',  ( 24.40424503925473232, -17.45211869376779390, 1.605444122987317757 ) ) ;
#22814 = CARTESIAN_POINT ( 'NONE',  ( 6.691656545360866737, -18.99987508458162111, 0.9788672205877712029 ) ) ;
#22815 = CARTESIAN_POINT ( 'NONE',  ( 0.1610798642962855409, -10.72944008624798506, 4.522129901861156931 ) ) ;
#22816 = CARTESIAN_POINT ( 'NONE',  ( -23.54713438637982748, 10.38166835460962645, 8.992620707982547756 ) ) ;
#22817 = CARTESIAN_POINT ( 'NONE',  ( 101.6022419886208610, -1.170867242066748304, -0.07017451552781628354 ) ) ;
#22818 = DIRECTION ( 'NONE',  ( -1.000000000000000000, 8.574039729943019576E-17, 0.000000000000000000 ) ) ;
#22819 = EDGE_CURVE ( 'NONE', #19157, #8703, #26235, .T. ) ;
#22820 = CARTESIAN_POINT ( 'NONE',  ( -3.550050802731187005, 2.983565686104819648, 0.3135853898029609677 ) ) ;
#22821 = ORIENTED_EDGE ( 'NONE', *, *, #31868, .F. ) ;
#22822 = CARTESIAN_POINT ( 'NONE',  ( -4.587550801365592790, -0.3701630799359326152, 3.521866450007987037 ) ) ;
#22823 = B_SPLINE_CURVE_WITH_KNOTS ( 'NONE', 3,
 ( #32931, #5014, #4822, #13017, #30593, #17876, #30767, #5323 ),
 .UNSPECIFIED., .F., .F.,
 ( 4, 2, 2, 4 ),
 ( 2.049880227679525047E-07, 0.001227965543375835562, 0.001841845821052371431, 0.002455726098728907517 ),
 .UNSPECIFIED. ) ;
#22824 = EDGE_CURVE ( 'NONE', #24760, #4026, #18685, .T. ) ;
#22825 = CARTESIAN_POINT ( 'NONE',  ( -41.09688370048776562, -10.96999999999998643, 8.628141679950115162 ) ) ;
#22826 = DIRECTION ( 'NONE',  ( 0.000000000000000000, 1.000000000000000000, 0.000000000000000000 ) ) ;
#22827 = EDGE_LOOP ( 'NONE', ( #20584, #16974, #31269, #21000 ) ) ;
#22828 = CARTESIAN_POINT ( 'NONE',  ( 6.883866621640341243, -5.066432324612676119, -7.111352071735073110 ) ) ;
#22829 = DIRECTION ( 'NONE',  ( -1.000000000000000000, 0.000000000000000000, 0.000000000000000000 ) ) ;
#22830 = VERTEX_POINT ( 'NONE', #8655 ) ;
#22831 = B_SPLINE_CURVE_WITH_KNOTS ( 'NONE', 3,
 ( #26307, #11418, #20959, #18454, #16078, #13401, #8077, #23618, #31330, #8407 ),
 .UNSPECIFIED., .F., .F.,
 ( 4, 2, 2, 2, 4 ),
 ( 2.571685856657688708E-07, 0.0005478592107668808775, 0.001095461252948095893, 0.001643063295129310692, 0.002190665337310525058 ),
 .UNSPECIFIED. ) ;
#22832 = CARTESIAN_POINT ( 'NONE',  ( -3.449949199999996274, 0.000000000000000000, 0.000000000000000000 ) ) ;
#22833 = CALENDAR_DATE ( 2026, 6, 10 ) ;
#22835 = EDGE_LOOP ( 'NONE', ( #23219, #16422, #23954, #22261 ) ) ;
#22834 = CARTESIAN_POINT ( 'NONE',  ( 84.65816297383790356, -6.961284151106942097, 0.07017451552781733826 ) ) ;
#22837 = EDGE_CURVE ( 'NONE', #9508, #5926, #16065, .T. ) ;
#22836 = ORIENTED_EDGE ( 'NONE', *, *, #5410, .T. ) ;
#22838 = CARTESIAN_POINT ( 'NONE',  ( -8.000050800000000351, 0.000000000000000000, 0.000000000000000000 ) ) ;
#22839 = EDGE_LOOP ( 'NONE', ( #9830, #32654, #32904 ) ) ;
#22840 = DIRECTION ( 'NONE',  ( -0.8660254037844409281, 0.4999999999999960587, 0.000000000000000000 ) ) ;
#22842 = ORIENTED_EDGE ( 'NONE', *, *, #14697, .F. ) ;
#22841 = DIRECTION ( 'NONE',  ( -1.000000000000000000, 0.000000000000000000, -3.469446951953611033E-15 ) ) ;
#22843 = DIRECTION ( 'NONE',  ( -0.9896144216807899463, 0.000000000000000000, -0.1437473352845035635 ) ) ;
#22844 = LINE ( 'NONE', #2798, #15507 ) ;
#22845 = CARTESIAN_POINT ( 'NONE',  ( 21.36697425079191959, -21.76267261028177913, -1.421487723214910570 ) ) ;
#22846 = EDGE_CURVE ( 'NONE', #19569, #12106, #13909, .T. ) ;
#22847 = FACE_OUTER_BOUND ( 'NONE', #1907, .T. ) ;
#22848 = B_SPLINE_CURVE_WITH_KNOTS ( 'NONE', 3,
 ( #18715, #6024, #3049, #29099, #10882, #13694, #21090, #6333, #21395, #13203, #23896, #13841, #5701, #15881, #3194, #1005 ),
 .UNSPECIFIED., .F., .F.,
 ( 4, 2, 2, 2, 2, 2, 2, 4 ),
 ( 0.009305842773645304003, 0.5000000000000000000, 0.6250000000000000000, 0.7500000000000000000, 0.8125000000000000000, 0.8750000000000000000, 0.9375000000000000000, 1.000000000000000000 ),
 .UNSPECIFIED. ) ;
#22849 = EDGE_LOOP ( 'NONE', ( #8680, #3755, #29269, #7091, #30136, #30249, #20780, #3378, #1527, #18968, #24241, #31946, #3890, #23385, #10402, #22461, #28019, #26776, #20014, #32862, #15108, #29701, #11201, #1889, #24319, #8404, #4368, #644, #22907, #32495, #21059, #22469, #2038, #11492, #14144, #11092, #22567, #14066, #31894, #28711, #14373, #11227, #24991, #14294, #26466, #2537 ) ) ;
#22850 = DIRECTION ( 'NONE',  ( 0.000000000000000000, 1.000000000000000000, 0.000000000000000000 ) ) ;
#22851 = CARTESIAN_POINT ( 'NONE',  ( -32.42885140446504977, -0.0003384977252881313063, 1.500000000000000000 ) ) ;
#22852 = DIRECTION ( 'NONE',  ( 1.000000000000000000, 0.000000000000000000, 0.000000000000000000 ) ) ;
#22853 = CARTESIAN_POINT ( 'NONE',  ( -50.81000000000000227, -10.96999999999998643, 5.700000000000000178 ) ) ;
#22854 = EDGE_CURVE ( 'NONE', #7258, #2968, #15855, .T. ) ;
#22855 = CARTESIAN_POINT ( 'NONE',  ( 23.17076627986326542, -21.93622647232682965, 1.056592207990660670 ) ) ;
#22856 = FACE_OUTER_BOUND ( 'NONE', #12097, .T. ) ;
#22857 = SPHERICAL_SURFACE ( 'NONE', #8117, 0.5000000000000000000 ) ;
#22858 = ORIENTED_EDGE ( 'NONE', *, *, #13268, .F. ) ;
#22859 = CARTESIAN_POINT ( 'NONE',  ( -6.062550801365593323, -0.3701630799359326152, 3.521866450007987037 ) ) ;
#22860 = ORIENTED_EDGE ( 'NONE', *, *, #27574, .F. ) ;
#22861 = CARTESIAN_POINT ( 'NONE',  ( -2.904531657079157725, 0.3127741368606810068, -2.975847129947406522 ) ) ;
#22862 = CARTESIAN_POINT ( 'NONE',  ( 24.11000000136559862, -2.892927487894331406, 1.570731468192932301 ) ) ;
#22863 = CARTESIAN_POINT ( 'NONE',  ( 107.5518430304144886, 18.50822805398703252, 5.148363126710675530 ) ) ;
#22864 = CARTESIAN_POINT ( 'NONE',  ( 102.9361373302715918, -5.944196040818415128, -2.713652344655542947 ) ) ;
#22865 = CARTESIAN_POINT ( 'NONE',  ( 107.9622325421415212, 20.81773585569407459, -1.491740999229417941 ) ) ;
#22866 = VERTEX_POINT ( 'NONE', #8484 ) ;
#22867 = FACE_OUTER_BOUND ( 'NONE', #25110, .T. ) ;
#22868 = DIRECTION ( 'NONE',  ( -1.000000000000000000, 0.000000000000000000, -0.000000000000000000 ) ) ;
#22869 = ORIENTED_EDGE ( 'NONE', *, *, #16506, .F. ) ;
#22870 = CARTESIAN_POINT ( 'NONE',  ( 4.499760686538666121, 7.347880794884119736E-16, -6.000000000000000000 ) ) ;
#22871 = DATE_AND_TIME ( #20554, #11953 ) ;
#22872 = EDGE_CURVE ( 'NONE', #4298, #14600, #245, .T. ) ;
#22873 = CARTESIAN_POINT ( 'NONE',  ( 102.4214166294606230, -3.972718723526538209, 4.033870034877223176 ) ) ;
#22874 = EDGE_CURVE ( 'NONE', #15877, #24728, #8491, .T. ) ;
#22875 = FACE_OUTER_BOUND ( 'NONE', #9991, .T. ) ;
#22877 = LINE ( 'NONE', #33080, #21468 ) ;
#22876 = CARTESIAN_POINT ( 'NONE',  ( 109.1168901022274724, 18.73997017427486256, -5.234450360147447689 ) ) ;
#22878 = VERTEX_POINT ( 'NONE', #3997 ) ;
#22879 = ADVANCED_FACE ( 'NONE', ( #27041 ), #6653, .F. ) ;
#22880 = CARTESIAN_POINT ( 'NONE',  ( 0.000000000000000000, -1.425064293572261276, -10.85582367538895632 ) ) ;
#22881 = CARTESIAN_POINT ( 'NONE',  ( 2.970200390936398982, 0.5647484630023784646, 9.143933199846962623 ) ) ;
#22882 = CARTESIAN_POINT ( 'NONE',  ( 24.79750000136559507, 2.363507492473148286, 1.913930629741525058 ) ) ;
#22883 = DIRECTION ( 'NONE',  ( 1.000000000000000000, 0.000000000000000000, 0.000000000000000000 ) ) ;
#22885 = VERTEX_POINT ( 'NONE', #4144 ) ;
#22884 = CARTESIAN_POINT ( 'NONE',  ( -1.033057378353320788, -8.048844657541357250, 4.522129901861157819 ) ) ;
#22886 = CARTESIAN_POINT ( 'NONE',  ( -5.962550801365593678, -2.752080473201636845, 2.228590825266444586 ) ) ;
#22887 = CARTESIAN_POINT ( 'NONE',  ( 2.274274201625327230, 0.000000000000000000, 0.000000000000000000 ) ) ;
#22888 = CARTESIAN_POINT ( 'NONE',  ( 5.489321708267612898, -6.285661071314506465, 5.138670926724877575 ) ) ;
#22889 = CARTESIAN_POINT ( 'NONE',  ( 29.24242457239609294, -6.576397578955832657, -3.993433898511009605 ) ) ;
#22890 = EDGE_LOOP ( 'NONE', ( #14881, #31266, #23651, #7164 ) ) ;
#22892 = ORIENTED_EDGE ( 'NONE', *, *, #7592, .T. ) ;
#22891 = CARTESIAN_POINT ( 'NONE',  ( 0.5032040285356987885, 3.698073368193082189, -9.002252291012698748 ) ) ;
#22893 = EDGE_CURVE ( 'NONE', #17980, #32298, #32063, .T. ) ;
#22894 = CARTESIAN_POINT ( 'NONE',  ( 0.000000000000000000, 0.5174497483512174867, 0.000000000000000000 ) ) ;
#22895 = DIRECTION ( 'NONE',  ( 1.000000000000000000, -8.574039729943018344E-17, -0.000000000000000000 ) ) ;
#22896 = CARTESIAN_POINT ( 'NONE',  ( 21.61000000136559507, 2.892927487894327410, -1.570731468192931635 ) ) ;
#22897 = CARTESIAN_POINT ( 'NONE',  ( 108.3696618535068126, 20.23658298680886958, 0.4463807625373348298 ) ) ;
#22898 = CARTESIAN_POINT ( 'NONE',  ( 0.5107832276858312870, -15.23285467310830477, -1.745873400673900289 ) ) ;
#22899 = CARTESIAN_POINT ( 'NONE',  ( 84.37491783462779438, -2.359815117480509539, -0.07017451552781631130 ) ) ;
#22900 = CARTESIAN_POINT ( 'NONE',  ( 68.92628806523025276, -3.240579989648460835, 0.07017451552782741353 ) ) ;
#22901 = CARTESIAN_POINT ( 'NONE',  ( 23.68064580653238949, -7.171681651382474598, 4.522129901861162260 ) ) ;
#22902 = VERTEX_POINT ( 'NONE', #9316 ) ;
#22903 = CARTESIAN_POINT ( 'NONE',  ( 2.857988133321601509, 7.318787950824199307, -6.150950518050498417 ) ) ;
#22904 = APPROVAL_ROLE ( '' ) ;
#22905 = EDGE_CURVE ( 'NONE', #9377, #25215, #16492, .T. ) ;
#22906 = DIRECTION ( 'NONE',  ( 0.000000000000000000, 0.000000000000000000, 1.000000000000000000 ) ) ;
#22907 = ORIENTED_EDGE ( 'NONE', *, *, #31452, .T. ) ;
#22908 = LINE ( 'NONE', #7717, #11369 ) ;
#22909 = ORIENTED_EDGE ( 'NONE', *, *, #13809, .T. ) ;
#22910 = CARTESIAN_POINT ( 'NONE',  ( -20.11703670643211339, 17.43879752748101808, 1.797616734936172023 ) ) ;
#22912 = ORIENTED_EDGE ( 'NONE', *, *, #12000, .F. ) ;
#22911 = CARTESIAN_POINT ( 'NONE',  ( 102.3458556242839563, -2.881957098797790717, -4.033870034884523115 ) ) ;
#22913 = ORIENTED_EDGE ( 'NONE', *, *, #12048, .F. ) ;
#22914 = CARTESIAN_POINT ( 'NONE',  ( -1.738758153310166144, -0.3178988483021044087, 3.024605502323848949 ) ) ;
#22915 = CARTESIAN_POINT ( 'NONE',  ( -6.662550801365592967, -3.521866450007987037, -0.3701630799359323931 ) ) ;
#22916 = CARTESIAN_POINT ( 'NONE',  ( 7.249760686538667009, -8.437262856154180923, 2.318425219014200511 ) ) ;
#22917 = CARTESIAN_POINT ( 'NONE',  ( 41.45135008765517881, -9.497951668093163491, -0.07017451552783579571 ) ) ;
#22919 = ORIENTED_EDGE ( 'NONE', *, *, #6497, .T. ) ;
#22918 = LINE ( 'NONE', #30299, #27800 ) ;
#22920 = CARTESIAN_POINT ( 'NONE',  ( 107.6641948605100083, -20.45809826282308208, 1.500000000000000000 ) ) ;
#22921 = CARTESIAN_POINT ( 'NONE',  ( 71.38866214471497074, -19.82505015900708401, 4.522129901861156931 ) ) ;
#22922 = CARTESIAN_POINT ( 'NONE',  ( -3.308639368481777421, -10.63993487576245656, 1.743554625370035582 ) ) ;
#22923 = PLANE ( 'NONE',  #12287 ) ;
#22925 = ORIENTED_EDGE ( 'NONE', *, *, #30321, .T. ) ;
#22924 = CARTESIAN_POINT ( 'NONE',  ( 108.0288149916133733, -18.48429082758350717, -4.339956994117294187 ) ) ;
#22926 = DIRECTION ( 'NONE',  ( 0.06927878976713691683, -0.9975973382524638833, 0.000000000000000000 ) ) ;
#22927 = EDGE_CURVE ( 'NONE', #27353, #18851, #29881, .T. ) ;
#22928 = CARTESIAN_POINT ( 'NONE',  ( 23.92250000273118715, -1.291182301015472378, -2.378061970571982098 ) ) ;
#22929 = DIRECTION ( 'NONE',  ( 0.000000000000000000, 0.7071067811865520136, -0.7071067811865431318 ) ) ;
#22930 = LINE ( 'NONE', #30670, #7030 ) ;
#22931 = DIRECTION ( 'NONE',  ( 0.000000000000000000, 0.000000000000000000, -1.000000000000000000 ) ) ;
#22932 = EDGE_LOOP ( 'NONE', ( #14720, #14176 ) ) ;
#22933 = DIRECTION ( 'NONE',  ( -1.000000000000000000, -0.000000000000000000, -0.000000000000000000 ) ) ;
#22934 = VECTOR ( 'NONE', #33036, 1000.000000000000000 ) ;
#22935 = DIRECTION ( 'NONE',  ( 1.000000000000000000, -0.000000000000000000, -0.000000000000000000 ) ) ;
#22936 = CARTESIAN_POINT ( 'NONE',  ( -5.987550801365593145, -3.521866450007987037, -0.3701630799359323931 ) ) ;
#22937 = ORIENTED_EDGE ( 'NONE', *, *, #8345, .F. ) ;
#22938 = ADVANCED_FACE ( 'NONE', ( #29375 ), #24693, .F. ) ;
#22939 = VECTOR ( 'NONE', #16301, 1000.000000000000000 ) ;
#22940 = CARTESIAN_POINT ( 'NONE',  ( 0.000000000000000000, 0.000000000000000000, 0.000000000000000000 ) ) ;
#22941 = ADVANCED_FACE ( 'NONE', ( #4303 ), #24361, .T. ) ;
#22942 = PLANE ( 'NONE',  #23167 ) ;
#22943 = CARTESIAN_POINT ( 'NONE',  ( 109.5084093630373729, -17.21855534384546971, -4.522129901861164925 ) ) ;
#22944 = CARTESIAN_POINT ( 'NONE',  ( 17.08731201381446851, -15.08866305798481733, 1.000000000000000222 ) ) ;
#22945 = ORIENTED_EDGE ( 'NONE', *, *, #4036, .T. ) ;
#22946 = CARTESIAN_POINT ( 'NONE',  ( 0.08034253207418005915, -4.547003328334541017, -9.783802610459700233 ) ) ;
#22947 = VERTEX_POINT ( 'NONE', #1477 ) ;
#22948 = CARTESIAN_POINT ( 'NONE',  ( -3.162653373152863878, 0.0004983460144369277704, 1.055926639512883680 ) ) ;
#22950 = ORIENTED_EDGE ( 'NONE', *, *, #15032, .F. ) ;
#22949 = DIRECTION ( 'NONE',  ( 1.000000000000000000, 0.000000000000000000, 0.000000000000000000 ) ) ;
#22951 = ORIENTED_EDGE ( 'NONE', *, *, #32704, .F. ) ;
#22952 = CARTESIAN_POINT ( 'NONE',  ( 3.122314033877864698E-16, 3.641590349731929965, 3.055657119358814011 ) ) ;
#22954 = ORIENTED_EDGE ( 'NONE', *, *, #3151, .F. ) ;
#22953 = VECTOR ( 'NONE', #28501, 999.9999999999998863 ) ;
#22956 = ORIENTED_EDGE ( 'NONE', *, *, #4512, .F. ) ;
#22955 = CARTESIAN_POINT ( 'NONE',  ( 1.305960519821096844, -9.941484022874826465, -1.500000000000000000 ) ) ;
#22957 = CIRCLE ( 'NONE', #8, 5.010000000000000675 ) ;
#22958 = CARTESIAN_POINT ( 'NONE',  ( 4.523414449530823944, -12.69491784415721725, -1.757045753096131424 ) ) ;
#22959 = CARTESIAN_POINT ( 'NONE',  ( 18.75828436641558028, -5.879118399717575549, 3.993434336035622589 ) ) ;
#22960 = DIRECTION ( 'NONE',  ( 0.000000000000000000, 0.000000000000000000, -1.000000000000000000 ) ) ;
#22961 = CARTESIAN_POINT ( 'NONE',  ( 5.377543748152549874, 2.741043480754926875, 7.530955069117522882 ) ) ;
#22962 = CIRCLE ( 'NONE', #29916, 8.500000000000000000 ) ;
#22963 = CARTESIAN_POINT ( 'NONE',  ( 2.619932554246601438E-16, 3.055657119358849982, -3.641590349731898879 ) ) ;
#22964 = SPHERICAL_SURFACE ( 'NONE', #19312, 0.5000000000000000000 ) ;
#22965 = DIRECTION ( 'NONE',  ( -1.000000000000000000, 0.000000000000000000, 0.000000000000000000 ) ) ;
#22966 = CARTESIAN_POINT ( 'NONE',  ( 74.30107678963170770, -22.79527490385382649, 1.500000000000000000 ) ) ;
#22967 = CARTESIAN_POINT ( 'NONE',  ( 3.249999999999999556, 4.057423117305515525, -8.475820894092930047 ) ) ;
#22968 = CARTESIAN_POINT ( 'NONE',  ( 7.249760686538667009, 8.711672189281426171, 0.8180878109962165246 ) ) ;
#22969 = CARTESIAN_POINT ( 'NONE',  ( 68.56906952848913761, -3.255983411058663179, -0.07017451552781628354 ) ) ;
#22970 = CIRCLE ( 'NONE', #21375, 0.5000000000000003331 ) ;
#22971 = DIRECTION ( 'NONE',  ( -1.000000000000000000, 0.000000000000000000, -8.654346879536960414E-15 ) ) ;
#22972 = EDGE_CURVE ( 'NONE', #19201, #31304, #3706, .T. ) ;
#22973 = CARTESIAN_POINT ( 'NONE',  ( -3.800050802731187005, -0.9222479816126459840, -3.113457007523259268 ) ) ;
#22974 = EDGE_LOOP ( 'NONE', ( #21596, #30545, #22079, #24779 ) ) ;
#22975 = ADVANCED_FACE ( 'NONE', ( #24508 ), #9471, .T. ) ;
#22976 = CARTESIAN_POINT ( 'NONE',  ( -6.137550801365595277, -1.828967928396026510, 3.368539882008728004 ) ) ;
#22977 = AXIS2_PLACEMENT_3D ( 'NONE', #14076, #1900, #9540 ) ;
#22978 = CARTESIAN_POINT ( 'NONE',  ( -2.600000000000000089, 0.000000000000000000, 1.500000000000000000 ) ) ;
#22979 = CARTESIAN_POINT ( 'NONE',  ( 20.58436699794885882, -21.58689779341630199, -1.578270943419022077 ) ) ;
#22980 = ORIENTED_EDGE ( 'NONE', *, *, #26153, .T. ) ;
#22981 = DIRECTION ( 'NONE',  ( -1.000000000000000000, 0.000000000000000000, 0.000000000000000000 ) ) ;
#22982 = CARTESIAN_POINT ( 'NONE',  ( 2.437082531750073056, 7.858345965138778588, 7.214115859539244724 ) ) ;
#22983 = VECTOR ( 'NONE', #25365, 1000.000000000000227 ) ;
#22984 = AXIS2_PLACEMENT_3D ( 'NONE', #22796, #12914, #23134 ) ;
#22985 = EDGE_LOOP ( 'NONE', ( #21271, #1323, #13868, #14106 ) ) ;
#22986 = FACE_OUTER_BOUND ( 'NONE', #19405, .T. ) ;
#22987 = SECURITY_CLASSIFICATION_LEVEL ( 'unclassified' ) ;
#22989 = ORIENTED_EDGE ( 'NONE', *, *, #29276, .F. ) ;
#22988 = CARTESIAN_POINT ( 'NONE',  ( 73.45519860863089434, -21.36028973287599086, -4.522129901861166701 ) ) ;
#22990 = ORIENTED_EDGE ( 'NONE', *, *, #922, .T. ) ;
#22991 = CARTESIAN_POINT ( 'NONE',  ( 10.46133304479515758, -19.61932188654371600, 1.750340032278390412 ) ) ;
#22992 = ORIENTED_EDGE ( 'NONE', *, *, #11850, .F. ) ;
#22993 = DIRECTION ( 'NONE',  ( -1.000000000000000000, 0.000000000000000000, -0.000000000000000000 ) ) ;
#22995 = VERTEX_POINT ( 'NONE', #26553 ) ;
#22994 = CARTESIAN_POINT ( 'NONE',  ( -54.05892116629462407, 5.342703470191877635, 1.499999999999898304 ) ) ;
#22996 = CARTESIAN_POINT ( 'NONE',  ( 23.61632761762314203, -8.296864917633476111, 2.713652344655544724 ) ) ;
#22997 = PLANE ( 'NONE',  #514 ) ;
#22998 = AXIS2_PLACEMENT_3D ( 'NONE', #12567, #20111, #30460 ) ;
#22999 = AXIS2_PLACEMENT_3D ( 'NONE', #15551, #2896, #13061 ) ;
#23000 = DIRECTION ( 'NONE',  ( 0.000000000000000000, -0.4226182617407076014, 0.9063077870366461619 ) ) ;
#23001 = CARTESIAN_POINT ( 'NONE',  ( 0.7632845268449858223, 8.461683424485162419, -2.223716399040675196 ) ) ;
#23002 = VECTOR ( 'NONE', #14162, 1000.000000000000000 ) ;
#23003 = VECTOR ( 'NONE', #24741, 1000.000000000000000 ) ;
#23004 = ORIENTED_EDGE ( 'NONE', *, *, #9488, .T. ) ;
#23005 = AXIS2_PLACEMENT_3D ( 'NONE', #10696, #30454, #27760 ) ;
#23006 = FACE_OUTER_BOUND ( 'NONE', #20727, .T. ) ;
#23007 = CARTESIAN_POINT ( 'NONE',  ( 107.6567584420023280, 16.56235156533065123, -1.437178912938893438 ) ) ;
#23008 = CARTESIAN_POINT ( 'NONE',  ( 1.750000000000000000, -2.834406817834851378, -8.013497238472808704 ) ) ;
#23009 = LINE ( 'NONE', #22526, #23699 ) ;
#23010 = AXIS2_PLACEMENT_3D ( 'NONE', #5046, #19587, #14874 ) ;
#23011 = EDGE_CURVE ( 'NONE', #15781, #596, #2738, .T. ) ;
#23012 = CARTESIAN_POINT ( 'NONE',  ( -8.000050800000011009, -0.4525887372486252502, 3.137152558661513435 ) ) ;
#23013 = CARTESIAN_POINT ( 'NONE',  ( -7.300050802731188782, -1.549418761218565255, 2.853674364686380471 ) ) ;
#23014 = DIRECTION ( 'NONE',  ( -1.000000000000000000, -6.938893903907222067E-15, 0.000000000000000000 ) ) ;
#23015 = LINE ( 'NONE', #27871, #31097 ) ;
#23016 = EDGE_LOOP ( 'NONE', ( #27939, #16651, #1388, #3189 ) ) ;
#23017 = CARTESIAN_POINT ( 'NONE',  ( -6.112550801365593145, 1.088641768524161613, 3.675193018007247403 ) ) ;
#23018 = ORIENTED_EDGE ( 'NONE', *, *, #28333, .F. ) ;
#23019 = EDGE_CURVE ( 'NONE', #31320, #25210, #32111, .T. ) ;
#23020 = CARTESIAN_POINT ( 'NONE',  ( -4.004531657079157370, -2.325406398514293205, 1.883076972206379818 ) ) ;
#23021 = AXIS2_PLACEMENT_3D ( 'NONE', #29037, #11127, #13780 ) ;
#23022 = EDGE_CURVE ( 'NONE', #8063, #2968, #16471, .T. ) ;
#23023 = CARTESIAN_POINT ( 'NONE',  ( 108.0792187206003518, 18.61928101938756441, 5.148720508272580432 ) ) ;
#23024 = CARTESIAN_POINT ( 'NONE',  ( 2.637177389002316463, 8.024708101613472686E-33, -1.518999257951627158 ) ) ;
#23025 = CARTESIAN_POINT ( 'NONE',  ( 15.81086013943126822, -14.68957281887663413, 1.000000000000000000 ) ) ;
#23026 = ORIENTED_EDGE ( 'NONE', *, *, #9148, .F. ) ;
#23027 = CARTESIAN_POINT ( 'NONE',  ( 21.78578353139858947, -21.77542465828167551, 1.497561405439323368 ) ) ;
#23028 = AXIS2_PLACEMENT_3D ( 'NONE', #415, #28657, #23631 ) ;
#23029 = CIRCLE ( 'NONE', #2202, 4.000000000000001776 ) ;
#23030 = AXIS2_PLACEMENT_3D ( 'NONE', #15277, #25988, #25827 ) ;
#23031 = ORIENTED_EDGE ( 'NONE', *, *, #33000, .F. ) ;
#23032 = CARTESIAN_POINT ( 'NONE',  ( 2.440333456264101475, -1.206185435479534496, -10.60697035672505706 ) ) ;
#23033 = CALENDAR_DATE ( 2026, 6, 10 ) ;
#23034 = EDGE_CURVE ( 'NONE', #10425, #9712, #25682, .T. ) ;
#23035 = CARTESIAN_POINT ( 'NONE',  ( 102.4209028682126501, -3.965302267389474888, 4.043900685069918843 ) ) ;
#23036 = AXIS2_PLACEMENT_3D ( 'NONE', #10081, #12442, #20295 ) ;
#23037 = AXIS2_PLACEMENT_3D ( 'NONE', #5500, #26049, #25542 ) ;
#23038 = AXIS2_PLACEMENT_3D ( 'NONE', #30500, #66, #13101 ) ;
#23039 = DIRECTION ( 'NONE',  ( -0.000000000000000000, 0.000000000000000000, 1.000000000000000000 ) ) ;
#23041 = DIRECTION ( 'NONE',  ( 1.000000000000000000, 5.361488761196502513E-16, -0.000000000000000000 ) ) ;
#23040 = CARTESIAN_POINT ( 'NONE',  ( 7.064423659272766720, 7.906491560605081403, 3.748318449931938634 ) ) ;
#23042 = ORIENTED_EDGE ( 'NONE', *, *, #3269, .T. ) ;
#23043 = EDGE_CURVE ( 'NONE', #1359, #2488, #10878, .T. ) ;
#23044 = CARTESIAN_POINT ( 'NONE',  ( -7.407304909706597051, 1.062355717592094573, 2.999999999999999556 ) ) ;
#23045 = CARTESIAN_POINT ( 'NONE',  ( 3.249999999999999556, -8.264486777890077462, -4.472189673936872722 ) ) ;
#23046 = CARTESIAN_POINT ( 'NONE',  ( 25.79750000136559507, 2.363507492473148286, 1.913930629741525058 ) ) ;
#23047 = DIRECTION ( 'NONE',  ( 0.000000000000000000, 0.5735764363510474917, -0.8191520442889909104 ) ) ;
#23049 = VERTEX_POINT ( 'NONE', #7454 ) ;
#23048 = CARTESIAN_POINT ( 'NONE',  ( 1.305960519821096844, -9.941484022874826465, 1.500000000000000444 ) ) ;
#23050 = CARTESIAN_POINT ( 'NONE',  ( -6.362550801365593145, 2.752080473201636845, -2.228590825266444142 ) ) ;
#23051 = CARTESIAN_POINT ( 'NONE',  ( 107.8715724909225173, 17.46302487926284996, -2.785784909554371858 ) ) ;
#23052 = ADVANCED_FACE ( 'NONE', ( #25015 ), #17350, .F. ) ;
#23053 = CIRCLE ( 'NONE', #24634, 0.5000000000000004441 ) ;
#23054 = CARTESIAN_POINT ( 'NONE',  ( -37.80541082197543545, 3.520075575296775838, 1.500000000000000222 ) ) ;
#23055 = DIRECTION ( 'NONE',  ( -1.000000000000000000, 0.000000000000000000, -0.000000000000000000 ) ) ;
#23056 = ORIENTED_EDGE ( 'NONE', *, *, #19757, .F. ) ;
#23057 = ORIENTED_EDGE ( 'NONE', *, *, #6907, .T. ) ;
#23058 = CIRCLE ( 'NONE', #20937, 8.750000000000000000 ) ;
#23059 = VECTOR ( 'NONE', #2403, 1000.000000000000114 ) ;
#23060 =( BOUNDED_SURFACE ( )  B_SPLINE_SURFACE ( 3, 2, ( 
 ( #7142, #17338, #32396 ),
 ( #4629, #14805, #25002 ),
 ( #2116, #29551, #32731 ),
 ( #17484, #27682, #6637 ) ),
 .UNSPECIFIED., .F., .F., .F. ) 
 B_SPLINE_SURFACE_WITH_KNOTS ( ( 4, 4 ),
 ( 3, 3 ),
 ( 0.0001830234508717654455, 0.0002186438461075107423 ),
 ( 0.000000000000000000, 1.000000000000000000 ),
 .UNSPECIFIED. ) 
 GEOMETRIC_REPRESENTATION_ITEM ( )  RATIONAL_B_SPLINE_SURFACE ( (
 ( 1.000000000000000000, 0.7071067811865441310, 1.000000000000000000),
 ( 1.000000000000000000, 0.7464405371105022891, 1.000000000000000000),
 ( 1.000000000000000000, 0.7823978085798950488, 1.000000000000000000),
 ( 1.000000000000000000, 0.8123215895921556129, 1.000000000000000000) ) ) 
 REPRESENTATION_ITEM ( '' )  SURFACE ( )  );
#23062 = AXIS2_PLACEMENT_3D ( 'NONE', #14740, #9226, #7380 ) ;
#23061 = DIRECTION ( 'NONE',  ( 0.000000000000000000, 1.000000000000000000, 0.000000000000000000 ) ) ;
#23063 = CARTESIAN_POINT ( 'NONE',  ( 14.23800746264082839, 22.11259878822726321, -1.491740999229417941 ) ) ;
#23064 = ADVANCED_FACE ( 'NONE', ( #7156 ), #12795, .F. ) ;
#23065 = CONICAL_SURFACE ( 'NONE', #6517, 2.524999999999999467, 0.7853981633974472798 ) ;
#23066 = EDGE_CURVE ( 'NONE', #11856, #32242, #27865, .T. ) ;
#23067 = CARTESIAN_POINT ( 'NONE',  ( 24.17250000136559507, -3.024605502323851169, 0.3178988483021052969 ) ) ;
#23068 = AXIS2_PLACEMENT_3D ( 'NONE', #10462, #8109, #7623 ) ;
#23069 = CARTESIAN_POINT ( 'NONE',  ( -28.84101375771544440, 6.775292334731556565, 2.070007460141180200 ) ) ;
#23070 = CARTESIAN_POINT ( 'NONE',  ( 0.1574692293613787764, -9.672096048330555362, 4.391622967207778672 ) ) ;
#23071 = CIRCLE ( 'NONE', #30022, 300.7453860596897357 ) ;
#23072 = DIRECTION ( 'NONE',  ( -6.062761635205574522E-17, -0.7071067811865465735, -0.7071067811865484609 ) ) ;
#23073 = CARTESIAN_POINT ( 'NONE',  ( 3.499999999999999556, -7.009698679648292519, 3.730838147389666126 ) ) ;
#23074 = ORIENTED_EDGE ( 'NONE', *, *, #22581, .F. ) ;
#23075 = EDGE_CURVE ( 'NONE', #12879, #11105, #4980, .T. ) ;
#23076 = CARTESIAN_POINT ( 'NONE',  ( -35.00000000000000000, 0.000000000000000000, 3.000000000000004441 ) ) ;
#23077 = VECTOR ( 'NONE', #5994, 1000.000000000000000 ) ;
#23079 = VECTOR ( 'NONE', #17622, 1000.000000000000000 ) ;
#23078 = SHAPE_DEFINITION_REPRESENTATION ( #2579, #1085 ) ;
#23080 = DIRECTION ( 'NONE',  ( 1.000000000000000000, 0.000000000000000000, 0.000000000000000000 ) ) ;
#23081 = AXIS2_PLACEMENT_3D ( 'NONE', #8140, #804, #10808 ) ;
#23082 = VERTEX_POINT ( 'NONE', #15166 ) ;
#23084 = EDGE_CURVE ( 'NONE', #25302, #29856, #31555, .T. ) ;
#23083 = AXIS2_PLACEMENT_3D ( 'NONE', #26451, #14317, #875 ) ;
#23085 = FACE_OUTER_BOUND ( 'NONE', #1219, .T. ) ;
#23086 = AXIS2_PLACEMENT_3D ( 'NONE', #29519, #6612, #4108 ) ;
#23087 = ORIENTED_EDGE ( 'NONE', *, *, #30385, .F. ) ;
#23088 = CARTESIAN_POINT ( 'NONE',  ( -5.100050802731186828, 2.853674364686379583, 1.549418761218565921 ) ) ;
#23090 = VERTEX_POINT ( 'NONE', #127 ) ;
#23089 = CARTESIAN_POINT ( 'NONE',  ( 102.3448865208385143, -2.867967694234029530, -4.013697985705315219 ) ) ;
#23091 = ORIENTED_EDGE ( 'NONE', *, *, #129, .F. ) ;
#23092 = TOROIDAL_SURFACE ( 'NONE', #27360, 10.46966150227468795, 0.5000000000000000000 ) ;
#23093 = DIRECTION ( 'NONE',  ( 1.000000000000000000, -0.000000000000000000, 1.388624693425297489E-14 ) ) ;
#23094 = CARTESIAN_POINT ( 'NONE',  ( -6.862550801365594033, -0.3701630799359326152, 3.521866450007987037 ) ) ;
#23095 = DIRECTION ( 'NONE',  ( 1.000000000000000000, -8.574039729943018344E-17, -0.000000000000000000 ) ) ;
#23096 = CIRCLE ( 'NONE', #31133, 8.749000000000002331 ) ;
#23097 = FACE_OUTER_BOUND ( 'NONE', #17996, .T. ) ;
#23098 = VERTEX_POINT ( 'NONE', #1980 ) ;
#23099 = DIRECTION ( 'NONE',  ( 0.000000000000000000, 0.5735764363510406083, 0.8191520442889955733 ) ) ;
#23100 = CARTESIAN_POINT ( 'NONE',  ( 2.281627749324421917, -0.2935656086769610207, 1.757435426329174044 ) ) ;
#23101 = CARTESIAN_POINT ( 'NONE',  ( -0.5879824335954042525, -14.86230332063114545, 1.500000000000000444 ) ) ;
#23102 = CARTESIAN_POINT ( 'NONE',  ( 24.48500000136559507, 2.892927487894327410, -1.570731468192931635 ) ) ;
#23103 = FACE_OUTER_BOUND ( 'NONE', #18488, .T. ) ;
#23106 = ADVANCED_FACE ( 'NONE', ( #12308 ), #32267, .T. ) ;
#23105 = ORIENTED_EDGE ( 'NONE', *, *, #11041, .F. ) ;
#23104 = DIRECTION ( 'NONE',  ( 0.9896144216807907235, -1.385833989420258499E-14, 0.1437473352844997332 ) ) ;
#23107 = DIRECTION ( 'NONE',  ( 0.000000000000000000, 0.000000000000000000, 1.000000000000000000 ) ) ;
#23108 = CIRCLE ( 'NONE', #8679, 7.318435636271054534 ) ;
#23109 = CIRCLE ( 'NONE', #8682, 9.000000000000001776 ) ;
#23110 = CARTESIAN_POINT ( 'NONE',  ( -28.64700708014754582, 15.87868365833990048, 1.835632814149771086 ) ) ;
#23111 = CARTESIAN_POINT ( 'NONE',  ( 21.36000000136559507, 0.9349337715887185984, -3.156283516753368268 ) ) ;
#23112 = EDGE_CURVE ( 'NONE', #24130, #11257, #23029, .T. ) ;
#23113 = AXIS2_PLACEMENT_3D ( 'NONE', #26334, #31201, #28516 ) ;
#23114 = EDGE_CURVE ( 'NONE', #9305, #7402, #10125, .T. ) ;
#23115 = VECTOR ( 'NONE', #9144, 1000.000000000000000 ) ;
#23116 = DIRECTION ( 'NONE',  ( -1.000000000000000000, -0.000000000000000000, -0.000000000000000000 ) ) ;
#23117 = AXIS2_PLACEMENT_3D ( 'NONE', #31011, #17974, #15794 ) ;
#23118 = CARTESIAN_POINT ( 'NONE',  ( 5.885541416630534428, 8.385500676968931089, -0.3712256868992730441 ) ) ;
#23119 = CARTESIAN_POINT ( 'NONE',  ( 40.73830215457783055, -6.894995700244995085, 3.993433058216659948 ) ) ;
#23120 = EDGE_LOOP ( 'NONE', ( #30178, #29422 ) ) ;
#23121 = CARTESIAN_POINT ( 'NONE',  ( 22.00639167669143603, -21.80013755708273848, 1.500000000000000000 ) ) ;
#23122 = CIRCLE ( 'NONE', #31670, 3.750000000000000444 ) ;
#23123 = AXIS2_PLACEMENT_3D ( 'NONE', #21038, #28562, #10824 ) ;
#23124 = CARTESIAN_POINT ( 'NONE',  ( 1.624999999999999778, -1.464956435139467272, -10.90201369670500497 ) ) ;
#23125 = CARTESIAN_POINT ( 'NONE',  ( -4.637550801365592612, 1.088641768524161613, 3.675193018007246959 ) ) ;
#23126 = ORIENTED_EDGE ( 'NONE', *, *, #826, .F. ) ;
#23127 = DIRECTION ( 'NONE',  ( -1.000000000000000000, 0.000000000000000000, 0.000000000000000000 ) ) ;
#23128 = CYLINDRICAL_SURFACE ( 'NONE', #7, 4.000000000000001776 ) ;
#23129 = CARTESIAN_POINT ( 'NONE',  ( 0.000000000000000000, -9.680994141368730155, -5.222868219166962866 ) ) ;
#23130 = VERTEX_POINT ( 'NONE', #30562 ) ;
#23131 = EDGE_CURVE ( 'NONE', #24949, #8736, #20886, .T. ) ;
#23132 = PRODUCT_DEFINITION ( 'UNKNOWN', '', #12467, #12502 ) ;
#23133 = CIRCLE ( 'NONE', #24715, 3.000000000000000444 ) ;
#23134 = DIRECTION ( 'NONE',  ( 0.000000000000000000, -0.7071067811865507924, -0.7071067811865441310 ) ) ;
#23135 = ORIENTED_EDGE ( 'NONE', *, *, #28515, .T. ) ;
#23136 = CARTESIAN_POINT ( 'NONE',  ( 107.4543402635612637, -17.42228831489675400, 4.691818008238314519 ) ) ;
#23137 = PRODUCT_DEFINITION_SHAPE ( 'NONE', 'NONE',  #33099 ) ;
#23138 = AXIS2_PLACEMENT_3D ( 'NONE', #6318, #495, #20890 ) ;
#23140 = ORIENTED_EDGE ( 'NONE', *, *, #8961, .F. ) ;
#23139 = CARTESIAN_POINT ( 'NONE',  ( -12.44989959798873436, 19.51744974835125035, -2.318435636271050537 ) ) ;
#23141 = ORIENTED_EDGE ( 'NONE', *, *, #3149, .F. ) ;
#23142 = FACE_OUTER_BOUND ( 'NONE', #31472, .T. ) ;
#23143 = VECTOR ( 'NONE', #29698, 1000.000000000000000 ) ;
#23144 = AXIS2_PLACEMENT_3D ( 'NONE', #19081, #7024, #25257 ) ;
#23145 = AXIS2_PLACEMENT_3D ( 'NONE', #20408, #23244, #31273 ) ;
#23146 = VERTEX_POINT ( 'NONE', #2631 ) ;
#23147 = CYLINDRICAL_SURFACE ( 'NONE', #16627, 8.500000000000000000 ) ;
#23149 = EDGE_LOOP ( 'NONE', ( #27647, #7830, #13874, #18277 ) ) ;
#23148 = CARTESIAN_POINT ( 'NONE',  ( 3.249999999999999556, -8.734705317681623171, -0.4999240074895356933 ) ) ;
#23150 = DIRECTION ( 'NONE',  ( 1.000000000000000000, -0.000000000000000000, -0.000000000000000000 ) ) ;
#23151 = CARTESIAN_POINT ( 'NONE',  ( 14.51811802657236505, -16.11687040489192313, -1.753674770401980387 ) ) ;
#23152 = DIRECTION ( 'NONE',  ( -1.000000000000000000, 0.000000000000000000, 0.000000000000000000 ) ) ;
#23153 = APPROVAL_PERSON_ORGANIZATION ( #30287, #17193, #10193 ) ;
#23154 = CARTESIAN_POINT ( 'NONE',  ( -45.60000000000000142, -10.96966150227468972, 1.500000000000000000 ) ) ;
#23155 = LINE ( 'NONE', #28310, #8531 ) ;
#23156 = CARTESIAN_POINT ( 'NONE',  ( 0.4883783024448289933, -9.508715662567844618, 2.300561732649534896 ) ) ;
#23157 = ADVANCED_FACE ( 'NONE', ( #5143 ), #19857, .F. ) ;
#23158 = EDGE_CURVE ( 'NONE', #32925, #17962, #7536, .T. ) ;
#23159 = DIRECTION ( 'NONE',  ( -1.000000000000000000, 0.000000000000000000, 0.000000000000000000 ) ) ;
#23160 = LINE ( 'NONE', #21140, #10238 ) ;
#23161 = DIRECTION ( 'NONE',  ( 1.000000000000000000, -2.473959037481237219E-13, 0.000000000000000000 ) ) ;
#23162 = CARTESIAN_POINT ( 'NONE',  ( 14.13431920379513862, -20.70626837987542856, 1.500000000000000000 ) ) ;
#23163 = CARTESIAN_POINT ( 'NONE',  ( 84.65816297383790356, -6.961284151106942097, -0.02339150517595087880 ) ) ;
#23164 = VECTOR ( 'NONE', #15614, 1000.000000000000114 ) ;
#23165 = CARTESIAN_POINT ( 'NONE',  ( -30.51827900900859802, 4.402097243136377180, 5.049999999999999822 ) ) ;
#23166 = CARTESIAN_POINT ( 'NONE',  ( 0.7632845268398871230, -8.734705317681623171, -0.4999240074895356933 ) ) ;
#23167 = AXIS2_PLACEMENT_3D ( 'NONE', #17588, #30325, #32994 ) ;
#23168 = CARTESIAN_POINT ( 'NONE',  ( 5.885541615502097201, -8.322568858718549123, -1.090540896198895160 ) ) ;
#23169 = CARTESIAN_POINT ( 'NONE',  ( -2.700050802731186916, 2.853674364686379583, 1.549418761218565921 ) ) ;
#23170 = ORIENTED_EDGE ( 'NONE', *, *, #21629, .T. ) ;
#23171 = AXIS2_PLACEMENT_3D ( 'NONE', #2236, #22640, #11748 ) ;
#23172 = CARTESIAN_POINT ( 'NONE',  ( -4.887550801365593500, 2.752080473201636845, -2.228590825266444142 ) ) ;
#23173 = DIRECTION ( 'NONE',  ( 1.000000000000000000, 0.000000000000000000, 0.000000000000000000 ) ) ;
#23174 = DIRECTION ( 'NONE',  ( 0.000000000000000000, -1.224646799147351482E-16, 1.000000000000000000 ) ) ;
#23175 = CC_DESIGN_APPROVAL ( #6550, ( #1824 ) ) ;
#23176 = ORIENTED_EDGE ( 'NONE', *, *, #4183, .T. ) ;
#23177 = CARTESIAN_POINT ( 'NONE',  ( 6.038145268433179780, -5.096160642893607040, -6.771555838910908065 ) ) ;
#23178 = SHAPE_REPRESENTATION_RELATIONSHIP ( 'NONE' , 'NONE' ,  #8974, #24295 ) ;
#23179 = VERTEX_POINT ( 'NONE', #308 ) ;
#23180 = CYLINDRICAL_SURFACE ( 'NONE', #28416, 0.5000000000000004441 ) ;
#23181 = CALENDAR_DATE ( 2026, 6, 10 ) ;
#23183 = ORIENTED_EDGE ( 'NONE', *, *, #19419, .F. ) ;
#23182 = CARTESIAN_POINT ( 'NONE',  ( 6.448894291894883501, -17.04229596238074151, -4.522129901861166701 ) ) ;
#23184 = ORIENTED_EDGE ( 'NONE', *, *, #7553, .T. ) ;
#23185 = CARTESIAN_POINT ( 'NONE',  ( -4.155175066657748495, -6.548221803322783252, 1.745040299909109027 ) ) ;
#23186 = ORIENTED_EDGE ( 'NONE', *, *, #20651, .F. ) ;
#23187 = CARTESIAN_POINT ( 'NONE',  ( -7.700050800000000528, 0.3135853898029611342, -2.983565686104819648 ) ) ;
#23188 = AXIS2_PLACEMENT_3D ( 'NONE', #29967, #7235, #32830 ) ;
#23190 = ORIENTED_EDGE ( 'NONE', *, *, #1944, .T. ) ;
#23189 = DIRECTION ( 'NONE',  ( -1.000000000000000000, 3.119226488900586565E-17, -7.720356475505610171E-17 ) ) ;
#23191 = CARTESIAN_POINT ( 'NONE',  ( 29.19831543700435716, -9.049787287704361916, 1.915219082070893863 ) ) ;
#23192 = CARTESIAN_POINT ( 'NONE',  ( 108.0795389336126107, -19.21470297384341919, 2.839262079369133662 ) ) ;
#23193 = EDGE_CURVE ( 'NONE', #24814, #30219, #5945, .T. ) ;
#23194 = CYLINDRICAL_SURFACE ( 'NONE', #29351, 4.000000000000001776 ) ;
#23195 = CARTESIAN_POINT ( 'NONE',  ( -16.85000000000000142, -10.96966150227469683, -11.50000000000000000 ) ) ;
#23196 = EDGE_CURVE ( 'NONE', #2628, #8281, #7964, .T. ) ;
#23197 = ORIENTED_EDGE ( 'NONE', *, *, #17824, .T. ) ;
#23198 = EDGE_CURVE ( 'NONE', #29383, #425, #2809, .T. ) ;
#23199 = CARTESIAN_POINT ( 'NONE',  ( 3.499999999999999556, 5.904264776415128146, -2.046865518294647579 ) ) ;
#23200 = CARTESIAN_POINT ( 'NONE',  ( 69.32965659118902124, -6.955028994486257332, 4.522129901861162260 ) ) ;
#23201 = CARTESIAN_POINT ( 'NONE',  ( 0.000000000000000000, 0.000000000000000000, 8.000000000000000000 ) ) ;
#23202 = CARTESIAN_POINT ( 'NONE',  ( -6.750050802731187183, 2.983565686104819648, 0.3135853898029609677 ) ) ;
#23203 = EDGE_LOOP ( 'NONE', ( #15659, #211, #26928, #18815 ) ) ;
#23204 = CARTESIAN_POINT ( 'NONE',  ( 24.39659513448239991, -17.41072360183627055, 1.416990234759656575 ) ) ;
#23205 = CARTESIAN_POINT ( 'NONE',  ( -7.007304909706599361, -1.062355717592095017, -2.999999999999999556 ) ) ;
#23206 = CARTESIAN_POINT ( 'NONE',  ( 0.1606233661161347581, -7.854816391753067784, -7.161985370900642245 ) ) ;
#23207 = CARTESIAN_POINT ( 'NONE',  ( -34.98223484310472031, 0.5000000000000000000, 3.000000000000004441 ) ) ;
#23208 = B_SPLINE_CURVE_WITH_KNOTS ( 'NONE', 3,
 ( #20312, #30522, #573, #21145, #15440, #8423 ),
 .UNSPECIFIED., .F., .F.,
 ( 4, 2, 4 ),
 ( 0.000000000000000000, 0.0009761895847327114973, 0.001952379169465422995 ),
 .UNSPECIFIED. ) ;
#23209 = EDGE_LOOP ( 'NONE', ( #6338, #13488, #7370, #26176 ) ) ;
#23210 = CARTESIAN_POINT ( 'NONE',  ( -6.912550801365593856, 1.088641768524161613, 3.675193018007247403 ) ) ;
#23211 = ORIENTED_EDGE ( 'NONE', *, *, #12116, .F. ) ;
#23212 = CARTESIAN_POINT ( 'NONE',  ( -3.654531657079158169, 1.545410377633947174, -2.846291840500173365 ) ) ;
#23213 = AXIS2_PLACEMENT_3D ( 'NONE', #24980, #2091, #3432 ) ;
#23214 = DIRECTION ( 'NONE',  ( -0.1027947991993878041, 0.9947025833170222153, 0.000000000000000000 ) ) ;
#23215 = CARTESIAN_POINT ( 'NONE',  ( 1.879786566314391560, -10.72333674525774860, 1.762694233963469026 ) ) ;
#23216 = CARTESIAN_POINT ( 'NONE',  ( 10.11068946041697991, -12.10067465432540956, 1.499999999999575451 ) ) ;
#23217 = EDGE_LOOP ( 'NONE', ( #4744, #29051, #25952, #21963 ) ) ;
#23218 = DIRECTION ( 'NONE',  ( 0.1437473352845080599, 0.000000000000000000, -0.9896144216807893912 ) ) ;
#23219 = ORIENTED_EDGE ( 'NONE', *, *, #10565, .T. ) ;
#23220 = CARTESIAN_POINT ( 'NONE',  ( 1.743702975966804347, -1.493758447930603195, 1.500000000000000000 ) ) ;
#23221 = PERSON_AND_ORGANIZATION ( #6766, #25292 ) ;
#23222 = CARTESIAN_POINT ( 'NONE',  ( 69.06910216928156387, -6.089391585246120897, 4.033870539709172753 ) ) ;
#23223 = ADVANCED_FACE ( 'NONE', ( #15475 ), #3136, .T. ) ;
#23224 = CARTESIAN_POINT ( 'NONE',  ( 2.410813113178261968, -0.09135288943933156380, -1.740945950644691154 ) ) ;
#23226 = CARTESIAN_POINT ( 'NONE',  ( 5.489344087273877903, 6.285690376021097592, 5.138668362895301378 ) ) ;
#23225 = CARTESIAN_POINT ( 'NONE',  ( 0.5640492482744806635, 8.091724846332327914, -5.053269777826572273 ) ) ;
#23227 = ORIENTED_EDGE ( 'NONE', *, *, #29793, .T. ) ;
#23228 = FACE_OUTER_BOUND ( 'NONE', #23518, .T. ) ;
#23229 = CARTESIAN_POINT ( 'NONE',  ( 2.795120610031290198, 0.7443816538168119834, 9.728666380680513370 ) ) ;
#23230 = CARTESIAN_POINT ( 'NONE',  ( 0.000000000000000000, 0.5000000000000000000, 0.000000000000000000 ) ) ;
#23231 = CARTESIAN_POINT ( 'NONE',  ( 10.00000000000000000, 0.8254815157535241310, 4.681538312723519724 ) ) ;
#23233 = ORIENTED_EDGE ( 'NONE', *, *, #7146, .F. ) ;
#23232 = FACE_OUTER_BOUND ( 'NONE', #14036, .T. ) ;
#23234 = VECTOR ( 'NONE', #11429, 1000.000000000000000 ) ;
#23235 = CARTESIAN_POINT ( 'NONE',  ( -7.612550801365593145, -1.828967928396026510, 3.368539882008728004 ) ) ;
#23236 = DIRECTION ( 'NONE',  ( 0.000000000000000000, 0.000000000000000000, 1.000000000000000000 ) ) ;
#23237 = CARTESIAN_POINT ( 'NONE',  ( -31.80940264096946635, 0.000000000000000000, 1.292893218813456535 ) ) ;
#23238 = ORIENTED_EDGE ( 'NONE', *, *, #20060, .F. ) ;
#23239 = EDGE_LOOP ( 'NONE', ( #25126, #29055, #29173, #6520, #25865 ) ) ;
#23240 = CARTESIAN_POINT ( 'NONE',  ( 24.22349034905675325, -17.32906192875313423, -1.351230503573957131 ) ) ;
#23241 = CARTESIAN_POINT ( 'NONE',  ( 107.7674015406661425, 19.73292211253945538, -3.806892900268363800 ) ) ;
#23242 = CARTESIAN_POINT ( 'NONE',  ( 23.73500000136559507, 3.156283516753366047, 0.9349337715887203748 ) ) ;
#23243 = LINE ( 'NONE', #26072, #14017 ) ;
#23244 = DIRECTION ( 'NONE',  ( 8.326672684688674053E-17, 0.3746065934159164001, -0.9271838545667857590 ) ) ;
#23245 = CARTESIAN_POINT ( 'NONE',  ( 35.34214449211032871, -3.792788106923192792, 0.07017451552782108526 ) ) ;
#23246 = CARTESIAN_POINT ( 'NONE',  ( 29.19213769713835305, -8.050053894909860119, 1.529339505909079966 ) ) ;
#23247 = ORIENTED_EDGE ( 'NONE', *, *, #31104, .F. ) ;
#23248 = DIRECTION ( 'NONE',  ( 8.659560562355058583E-17, 0.3907311284892827086, 0.9205048534524364889 ) ) ;
#23249 = B_SPLINE_CURVE_WITH_KNOTS ( 'NONE', 3,
 ( #6865, #11905, #22109, #32323 ),
 .UNSPECIFIED., .F., .F.,
 ( 4, 4 ),
 ( 9.757819552369539906E-19, 0.0003032258210394150151 ),
 .UNSPECIFIED. ) ;
#23250 = ADVANCED_FACE ( 'NONE', ( #5642 ), #31375, .T. ) ;
#23251 = CALENDAR_DATE ( 2026, 6, 10 ) ;
#23252 = CARTESIAN_POINT ( 'NONE',  ( 102.6421141555943706, -1.710335469228581484, 0.07017451552783579571 ) ) ;
#23253 = EDGE_LOOP ( 'NONE', ( #30541, #314, #9680, #14952 ) ) ;
#23254 = CARTESIAN_POINT ( 'NONE',  ( -12.44989959798873791, 19.50000000000000000, -12.99999999999999645 ) ) ;
#23255 = EDGE_LOOP ( 'NONE', ( #7405, #3193, #3183, #31094, #4748, #8594, #19986, #17377, #3689, #16439, #22404, #218 ) ) ;
#23256 = CARTESIAN_POINT ( 'NONE',  ( -19.39001922729729088, 5.591785014860885639, 2.102227713797247155 ) ) ;
#23258 = EDGE_LOOP ( 'NONE', ( #30295, #22111, #1334, #22685 ) ) ;
#23257 = CARTESIAN_POINT ( 'NONE',  ( 69.01789987928717096, -5.063907424387957157, -4.112224952817434165 ) ) ;
#23259 = ORIENTED_EDGE ( 'NONE', *, *, #26662, .F. ) ;
#23260 = ADVANCED_FACE ( 'NONE', ( #5298 ), #31902, .F. ) ;
#23261 = ADVANCED_FACE ( 'NONE', ( #1589 ), #11713, .T. ) ;
#23262 = CARTESIAN_POINT ( 'NONE',  ( 18.53175858344379634, -21.44524224917989130, 1.500000000000000000 ) ) ;
#23263 = CARTESIAN_POINT ( 'NONE',  ( -6.062550801365593323, -0.3701630799359326152, 3.521866450007987037 ) ) ;
#23264 = CARTESIAN_POINT ( 'NONE',  ( 8.528645601772334217, -0.5000000000000011102, 1.500000000000000000 ) ) ;
#23265 = CARTESIAN_POINT ( 'NONE',  ( 109.4831014662948974, 20.77917954950586577, -0.4463807625373443777 ) ) ;
#23266 =( BOUNDED_CURVE ( )  B_SPLINE_CURVE ( 2, ( #5793, #15970, #8619, #29039, #6130, #20696, #25881, #2997, #26191, #30897, #7970 ),
 .UNSPECIFIED., .F., .T. ) 
 B_SPLINE_CURVE_WITH_KNOTS ( ( 3, 2, 2, 2, 2, 3 ),
 ( 0.3966116191895003862, 0.4000000000000000222, 0.4249999999999999889, 0.4500000000000000111, 0.4749999999999999778, 0.4966116191895003640 ),
 .UNSPECIFIED. ) 
 CURVE ( )  GEOMETRIC_REPRESENTATION_ITEM ( )  RATIONAL_B_SPLINE_CURVE ( ( 0.9821626249036858880, 0.9896829947469992783, 1.000000000000000000, 0.9238795325112867385, 1.000000000000000000, 0.9238795325112867385, 1.000000000000000000, 0.9238795325112867385, 1.000000000000000000, 0.9341965377642874602, 0.9821626249036858880 ) ) 
 REPRESENTATION_ITEM ( '' )  );
#23268 = EDGE_LOOP ( 'NONE', ( #14168, #22546, #2004, #16511, #1448 ) ) ;
#23267 = CARTESIAN_POINT ( 'NONE',  ( 0.1574692315735298220, -5.243558859478220313, 9.238013023060297257 ) ) ;
#23269 = CARTESIAN_POINT ( 'NONE',  ( 7.577572045913208321, 15.00000000000002132, 4.629213727441584325 ) ) ;
#23270 = CARTESIAN_POINT ( 'NONE',  ( 2.288113303901286422, -16.46502519983721413, 1.747280108055323522 ) ) ;
#23271 = CARTESIAN_POINT ( 'NONE',  ( 21.48500000136559507, 0.9349337715887185984, -3.156283516753368268 ) ) ;
#23272 = CARTESIAN_POINT ( 'NONE',  ( 3.063284526839887167, 0.4999240074894433228, 8.734705317681628500 ) ) ;
#23275 = ADVANCED_FACE ( 'NONE', ( #14127 ), #11615, .T. ) ;
#23274 = ORIENTED_EDGE ( 'NONE', *, *, #12610, .F. ) ;
#23273 = CARTESIAN_POINT ( 'NONE',  ( 107.5618984974341146, -18.98541497655834220, -4.517168112729012641 ) ) ;
#23276 = DIRECTION ( 'NONE',  ( -0.006769954505784999722, -0.9999770835954140402, -0.000000000000000000 ) ) ;
#23277 = B_SPLINE_CURVE_WITH_KNOTS ( 'NONE', 3,
 ( #24893, #1664, #26733, #17018, #1854, #14694, #1503, #3850, #29598, #2005 ),
 .UNSPECIFIED., .F., .F.,
 ( 4, 2, 2, 2, 4 ),
 ( 1.968338519002218415E-07, 0.0005467926089500440819, 0.001093388384048187825, 0.001639984159146331676, 0.002186579934244475745 ),
 .UNSPECIFIED. ) ;
#23278 = CARTESIAN_POINT ( 'NONE',  ( -29.36843332409777574, 14.72720444484234115, 1.864077576974227934 ) ) ;
#23279 = CARTESIAN_POINT ( 'NONE',  ( 24.98500000273118715, -0.2613211581691358698, -2.486304738420681559 ) ) ;
#23280 = CARTESIAN_POINT ( 'NONE',  ( -8.000050800000000351, 0.3135937863663861291, -2.983645574069408557 ) ) ;
#23281 = EDGE_CURVE ( 'NONE', #32470, #20203, #29520, .T. ) ;
#23282 = DIRECTION ( 'NONE',  ( -1.000000000000000000, 0.000000000000000000, 0.000000000000000000 ) ) ;
#23283 = LINE ( 'NONE', #10558, #20992 ) ;
#23284 = ORIENTED_EDGE ( 'NONE', *, *, #20606, .T. ) ;
#23285 = CARTESIAN_POINT ( 'NONE',  ( 107.6641398346957033, -20.45810202417174750, 1.500000000000000000 ) ) ;
#23286 = CARTESIAN_POINT ( 'NONE',  ( 56.97280603064898941, -277.2763395528616002, -0.4463807625373771293 ) ) ;
#23287 = ORIENTED_EDGE ( 'NONE', *, *, #23640, .T. ) ;
#23288 = CARTESIAN_POINT ( 'NONE',  ( -15.51216819290874227, -21.43932300455805873, 1.500000000000000000 ) ) ;
#23289 = CARTESIAN_POINT ( 'NONE',  ( 0.000000000000000000, 4.709950686174755319, -9.884132761439010650 ) ) ;
#23290 = CARTESIAN_POINT ( 'NONE',  ( -0.7739934281325309140, -8.972773999336983053, -4.522129901861164925 ) ) ;
#23292 = CARTESIAN_POINT ( 'NONE',  ( 107.9883904550100482, -17.90218755680270846, 5.108687026697555922 ) ) ;
#23291 = CARTESIAN_POINT ( 'NONE',  ( 7.686969782318655575, -9.486238560348441595, 1.000000000000000222 ) ) ;
#23293 = ORIENTED_EDGE ( 'NONE', *, *, #14280, .T. ) ;
#23294 = DIRECTION ( 'NONE',  ( -1.000000000000000000, 8.574039729943017111E-17, -0.000000000000000000 ) ) ;
#23295 = EDGE_LOOP ( 'NONE', ( #9913, #11943, #859, #30976 ) ) ;
#23296 = CARTESIAN_POINT ( 'NONE',  ( 0.000000000000000000, 10.85582367538894211, 1.425064293572374963 ) ) ;
#23298 = ORIENTED_EDGE ( 'NONE', *, *, #12853, .T. ) ;
#23297 = CARTESIAN_POINT ( 'NONE',  ( 109.3153218317886655, 19.84491634189296860, -3.222654707407530239 ) ) ;
#23299 = ORIENTED_EDGE ( 'NONE', *, *, #5299, .F. ) ;
#23300 = DIRECTION ( 'NONE',  ( 0.000000000000000000, 0.000000000000000000, 1.000000000000000000 ) ) ;
#23301 = ADVANCED_FACE ( 'NONE', ( #8935 ), #6613, .T. ) ;
#23302 = EDGE_CURVE ( 'NONE', #24612, #19151, #7012, .T. ) ;
#23303 = CARTESIAN_POINT ( 'NONE',  ( 5.489344046532323773, -6.978601450725515853, 4.149088721182507378 ) ) ;
#23305 = ORIENTED_EDGE ( 'NONE', *, *, #6038, .T. ) ;
#23304 = CARTESIAN_POINT ( 'NONE',  ( 1.278428506419904798, -2.392608122357158251, 1.500000000000000000 ) ) ;
#23306 = ORIENTED_EDGE ( 'NONE', *, *, #12949, .T. ) ;
#23307 = CARTESIAN_POINT ( 'NONE',  ( 21.03177542174473658, -17.18603084754145982, -1.753176640694677380 ) ) ;
#23308 = CARTESIAN_POINT ( 'NONE',  ( 18.65791233782715963, -7.001076235476726417, 2.184956778830005497 ) ) ;
#23309 = DIRECTION ( 'NONE',  ( 0.4999999999999981681, 0.8660254037844395958, -0.000000000000000000 ) ) ;
#23310 = DIRECTION ( 'NONE',  ( -0.4851627901281745370, -0.000000000000000000, -0.8744238486426618717 ) ) ;
#23311 = CARTESIAN_POINT ( 'NONE',  ( 107.9171431298509987, -16.87624379866894841, 2.462434481765830796 ) ) ;
#23312 = CARTESIAN_POINT ( 'NONE',  ( 107.5617870618796701, -18.98359792747699970, -4.522129903277523510 ) ) ;
#23313 = CARTESIAN_POINT ( 'NONE',  ( 0.5491634894704520153, -7.006993281499743098, 1.500000000000000222 ) ) ;
#23314 = CARTESIAN_POINT ( 'NONE',  ( 41.35430931302155244, -7.517178856345512195, 2.787783064021091661 ) ) ;
#23315 = EDGE_CURVE ( 'NONE', #5917, #19301, #32135, .T. ) ;
#23316 = FACE_OUTER_BOUND ( 'NONE', #23966, .T. ) ;
#23317 = CARTESIAN_POINT ( 'NONE',  ( 5.377543748152549874, 5.151476664237558900, -6.139290821770204687 ) ) ;
#23318 = CC_DESIGN_PERSON_AND_ORGANIZATION_ASSIGNMENT ( #18176, #10652, ( #10350 ) ) ;
#23319 = CARTESIAN_POINT ( 'NONE',  ( 5.612974441954674987, -5.432722698947198836, 6.163896661468954541 ) ) ;
#23320 = CARTESIAN_POINT ( 'NONE',  ( 6.880159790065805581, -8.691376398188692676, -0.8322990769133310485 ) ) ;
#23321 = CARTESIAN_POINT ( 'NONE',  ( 3.063284526839891608, 8.734705317681621395, 0.4999240074894719665 ) ) ;
#23322 = EDGE_LOOP ( 'NONE', ( #29493, #29405, #15807, #9334 ) ) ;
#23323 = CARTESIAN_POINT ( 'NONE',  ( -2.450050802731187360, -2.331437884370912705, 1.887961173149512062 ) ) ;
#23324 = CARTESIAN_POINT ( 'NONE',  ( -31.18783180709124636, 0.000000000000000000, 1.000000000000000000 ) ) ;
#23325 = ORIENTED_EDGE ( 'NONE', *, *, #30385, .T. ) ;
#23326 = CARTESIAN_POINT ( 'NONE',  ( 18.86054332783516330, -4.736068442360130248, -3.993434336035624366 ) ) ;
#23327 = ADVANCED_FACE ( 'NONE', ( #16807 ), #14274, .T. ) ;
#23328 = EDGE_LOOP ( 'NONE', ( #6064, #26847, #7907, #25808 ) ) ;
#23329 = CARTESIAN_POINT ( 'NONE',  ( 102.5305753040692736, -0.1042037546421111793, -1.010822989962086416 ) ) ;
#23330 = CONTEXT_DEPENDENT_SHAPE_REPRESENTATION ( #26369, #30064 ) ;
#23332 = ORIENTED_EDGE ( 'NONE', *, *, #12199, .F. ) ;
#23331 = CARTESIAN_POINT ( 'NONE',  ( 42.88108885380913193, -22.62752020922543750, -4.522129901861166701 ) ) ;
#23333 = ORIENTED_EDGE ( 'NONE', *, *, #3684, .F. ) ;
#23334 = CARTESIAN_POINT ( 'NONE',  ( 0.1079232672943445104, 10.52718011138291132, 2.097182127099708637 ) ) ;
#23335 = ORIENTED_EDGE ( 'NONE', *, *, #21956, .T. ) ;
#23336 = DIRECTION ( 'NONE',  ( -1.000000000000000000, 8.574039729943017111E-17, -0.000000000000000000 ) ) ;
#23338 = ORIENTED_EDGE ( 'NONE', *, *, #9971, .T. ) ;
#23337 = CARTESIAN_POINT ( 'NONE',  ( -2.429479563265797726, 0.4428684773465039748, 3.145100343978137758 ) ) ;
#23339 = CARTESIAN_POINT ( 'NONE',  ( 11.62091610453458301, 3.869040036316004016, 1.050000000000000044 ) ) ;
#23340 = CARTESIAN_POINT ( 'NONE',  ( -31.59999999999999787, -25.43932300454937945, 11.00000000000000000 ) ) ;
#23341 = CARTESIAN_POINT ( 'NONE',  ( -50.60000000000000142, -21.93932300454937945, 1.500000000000000000 ) ) ;
#23342 = CARTESIAN_POINT ( 'NONE',  ( -41.54004718934325524, -10.96999999999998643, 8.549999999999998934 ) ) ;
#23343 = ORIENTED_EDGE ( 'NONE', *, *, #31232, .F. ) ;
#23344 = FACE_OUTER_BOUND ( 'NONE', #26160, .T. ) ;
#23345 = CARTESIAN_POINT ( 'NONE',  ( 13.13178786249840435, -17.31629153505178920, -4.522129901861164925 ) ) ;
#23346 = CARTESIAN_POINT ( 'NONE',  ( 55.00869849602045036, -7.632537969515627907, -2.184956776156974811 ) ) ;
#23347 = CARTESIAN_POINT ( 'NONE',  ( 2.652619124157556740, 0.000000000000000000, -1.000000000000000000 ) ) ;
#23348 = DIRECTION ( 'NONE',  ( 0.03488359650710490256, 0.9989355049964836475, -0.03018263660036206442 ) ) ;
#23349 = CARTESIAN_POINT ( 'NONE',  ( 10.00000000000000000, -1.625881193364728805, 4.467071865485467086 ) ) ;
#23350 = CARTESIAN_POINT ( 'NONE',  ( 0.5032041927225605615, -7.418882907483827616, -6.298925283836324773 ) ) ;
#23351 = DIRECTION ( 'NONE',  ( 0.000000000000000000, -1.000000000000000000, 0.000000000000000000 ) ) ;
#23352 = ORIENTED_EDGE ( 'NONE', *, *, #10314, .F. ) ;
#23353 = CARTESIAN_POINT ( 'NONE',  ( -3.662550801365593411, -0.3701630799359326152, 3.521866450007987037 ) ) ;
#23354 = ORIENTED_EDGE ( 'NONE', *, *, #2689, .F. ) ;
#23355 = CARTESIAN_POINT ( 'NONE',  ( -8.150050800000000706, 0.9222479816126443186, 3.113457007523260156 ) ) ;
#23356 = CARTESIAN_POINT ( 'NONE',  ( 108.0068349480237373, 18.21621961241920573, 4.414771370926587224 ) ) ;
#23357 = DIRECTION ( 'NONE',  ( 0.000000000000000000, 0.000000000000000000, -1.000000000000000000 ) ) ;
#23358 = CARTESIAN_POINT ( 'NONE',  ( 25.61042644977005622, -17.59778802277103082, 1.000000000000000000 ) ) ;
#23359 = ORIENTED_EDGE ( 'NONE', *, *, #27945, .T. ) ;
#23360 = EDGE_CURVE ( 'NONE', #23664, #7166, #17705, .T. ) ;
#23361 = CARTESIAN_POINT ( 'NONE',  ( 68.99418471616998261, -4.594926857587732449, -3.390608975016885296 ) ) ;
#23362 = EDGE_CURVE ( 'NONE', #6075, #4203, #1152, .T. ) ;
#23363 = ORIENTED_EDGE ( 'NONE', *, *, #29795, .F. ) ;
#23364 = CARTESIAN_POINT ( 'NONE',  ( 0.5640492184783237883, 8.844377740304926405, 3.576105523026929855 ) ) ;
#23365 = EDGE_CURVE ( 'NONE', #17091, #25011, #5964, .T. ) ;
#23366 = DATE_AND_TIME ( #10828, #31207 ) ;
#23367 =( REPRESENTATION_RELATIONSHIP ('NONE','NONE', #1085, #13 ) REPRESENTATION_RELATIONSHIP_WITH_TRANSFORMATION ( #20819 )SHAPE_REPRESENTATION_RELATIONSHIP( ) );
#23368 = CARTESIAN_POINT ( 'NONE',  ( 40.88303942367309674, -6.721012086063126389, 4.185347298787005066 ) ) ;
#23369 = LINE ( 'NONE', #20864, #17621 ) ;
#23371 = PLANE ( 'NONE',  #21983 ) ;
#23370 = DIRECTION ( 'NONE',  ( 0.000000000000000000, 1.000000000000000000, 0.000000000000000000 ) ) ;
#23372 = ORIENTED_EDGE ( 'NONE', *, *, #19461, .T. ) ;
#23373 = CARTESIAN_POINT ( 'NONE',  ( 12.40148790557316616, 21.49000000000003041, -1.500000000000000000 ) ) ;
#23374 = CARTESIAN_POINT ( 'NONE',  ( 21.08401840680261330, -16.78474387324011374, 1.949999999999999956 ) ) ;
#23375 = CARTESIAN_POINT ( 'NONE',  ( 9.266707753004494563, -0.05004968855533439842, 1.221243012139963779 ) ) ;
#23377 = VERTEX_POINT ( 'NONE', #17311 ) ;
#23376 = CARTESIAN_POINT ( 'NONE',  ( 9.297238421960550170, 0.2387279282522293267, -1.050000000000000044 ) ) ;
#23378 = CARTESIAN_POINT ( 'NONE',  ( -5.712550801365594566, -1.088641768524163389, -3.675193018007246071 ) ) ;
#23379 = CARTESIAN_POINT ( 'NONE',  ( 4.499760686538666121, 0.000000000000000000, 6.000000000000000000 ) ) ;
#23380 = DIRECTION ( 'NONE',  ( 0.000000000000000000, 1.000000000000000000, 0.000000000000000000 ) ) ;
#23381 = ORIENTED_EDGE ( 'NONE', *, *, #31853, .F. ) ;
#23382 = ORIENTED_EDGE ( 'NONE', *, *, #25936, .F. ) ;
#23383 = CARTESIAN_POINT ( 'NONE',  ( 23.26681913457865392, -17.19558280316121568, -1.454198315410691000 ) ) ;
#23384 = CARTESIAN_POINT ( 'NONE',  ( -32.07659242536668387, -21.93932300455396245, -1.000000000000000000 ) ) ;
#23385 = ORIENTED_EDGE ( 'NONE', *, *, #21104, .T. ) ;
#23386 = CARTESIAN_POINT ( 'NONE',  ( 23.61000000136559507, 2.892927487894327410, -1.570731468192931635 ) ) ;
#23387 = CARTESIAN_POINT ( 'NONE',  ( 0.3045634402744734071, -9.425384029459451085, 4.096074720329322183 ) ) ;
#23388 = DIRECTION ( 'NONE',  ( 1.000000000000000000, -8.574039729943018344E-17, -0.000000000000000000 ) ) ;
#23389 = DIRECTION ( 'NONE',  ( 8.574039729943018344E-17, 1.000000000000000000, 0.000000000000000000 ) ) ;
#23390 = CARTESIAN_POINT ( 'NONE',  ( 35.27024661284173135, -8.402227462205930308, 0.4367666027820644170 ) ) ;
#23391 = VERTEX_POINT ( 'NONE', #9774 ) ;
#23392 = ADVANCED_FACE ( 'NONE', ( #17801 ), #2264, .T. ) ;
#23393 = DIRECTION ( 'NONE',  ( 0.000000000000000000, 0.000000000000000000, 1.000000000000000000 ) ) ;
#23394 = EDGE_CURVE ( 'NONE', #17959, #32155, #16620, .T. ) ;
#23395 = ORIENTED_EDGE ( 'NONE', *, *, #18545, .T. ) ;
#23396 = APPROVAL_DATE_TIME ( #13193, #19048 ) ;
#23397 = CARTESIAN_POINT ( 'NONE',  ( 28.60502136296933884, -6.760022240765948709, -3.993434336023340858 ) ) ;
#23398 = ORIENTED_EDGE ( 'NONE', *, *, #24866, .F. ) ;
#23399 = CARTESIAN_POINT ( 'NONE',  ( 16.02446143562542602, -14.75799222003427857, -0.9999999999999997780 ) ) ;
#23400 = ORIENTED_EDGE ( 'NONE', *, *, #18924, .F. ) ;
#23401 = CARTESIAN_POINT ( 'NONE',  ( -23.54713438638086842, 3.998227953278294944, 2.146185852361370383 ) ) ;
#23403 = EDGE_LOOP ( 'NONE', ( #27184, #23721, #21051, #1003 ) ) ;
#23402 = CARTESIAN_POINT ( 'NONE',  ( 18.85384210216383138, -4.810974696175653875, -4.093303788729898862 ) ) ;
#23404 = ORIENTED_EDGE ( 'NONE', *, *, #12830, .F. ) ;
#23405 = CARTESIAN_POINT ( 'NONE',  ( -15.51216819290874227, -21.43932300455805873, 1.500000000000000000 ) ) ;
#23406 = CARTESIAN_POINT ( 'NONE',  ( -7.512550801365593500, -3.675193018007245627, 1.088641768524163389 ) ) ;
#23407 = CARTESIAN_POINT ( 'NONE',  ( 25.67249999999999943, -1.291182301015472378, -2.378061970571982098 ) ) ;
#23408 = DIRECTION ( 'NONE',  ( 0.06927878976713820747, -0.9975973382524637723, 0.000000000000000000 ) ) ;
#23410 = ORIENTED_EDGE ( 'NONE', *, *, #20919, .F. ) ;
#23409 = CARTESIAN_POINT ( 'NONE',  ( 5.885541736258998569, 7.752826540560551649, -3.216848386727986675 ) ) ;
#23411 = CARTESIAN_POINT ( 'NONE',  ( 7.249760686538667009, 2.318425219014346172, -8.437262856154140067 ) ) ;
#23412 = CARTESIAN_POINT ( 'NONE',  ( 10.51841884045068731, 2.077444665426179782, 1.500000000000118572 ) ) ;
#23413 = CARTESIAN_POINT ( 'NONE',  ( -3.910407125125240579, -9.341411376702357217, 1.499999999999999778 ) ) ;
#23414 = CARTESIAN_POINT ( 'NONE',  ( 0.5704039292223133106, -7.316743080999480675, 6.124150562935273712 ) ) ;
#23415 = FACE_OUTER_BOUND ( 'NONE', #32992, .T. ) ;
#23417 = VERTEX_POINT ( 'NONE', #12449 ) ;
#23416 = DIRECTION ( 'NONE',  ( 6.062761635205578219E-17, 0.7071067811865465735, 0.7071067811865484609 ) ) ;
#23418 = LINE ( 'NONE', #7887, #14094 ) ;
#23419 = EDGE_CURVE ( 'NONE', #8954, #28455, #8090, .T. ) ;
#23420 = CARTESIAN_POINT ( 'NONE',  ( -30.10261078476095520, 12.34770688644884906, 1.923950361969430922 ) ) ;
#23421 = CARTESIAN_POINT ( 'NONE',  ( 25.29750000273118715, 2.594547506269380133, 0.7685399846772031918 ) ) ;
#23422 = FACE_OUTER_BOUND ( 'NONE', #30186, .T. ) ;
#23423 = CARTESIAN_POINT ( 'NONE',  ( 109.7786606840771952, 18.61415246516070354, 5.412820279296878923 ) ) ;
#23424 = CARTESIAN_POINT ( 'NONE',  ( -2.972652642344704166, -0.1886749676220912386, -1.397177942464456812 ) ) ;
#23425 = EDGE_CURVE ( 'NONE', #17955, #18253, #33017, .T. ) ;
#23426 = ORIENTED_EDGE ( 'NONE', *, *, #873, .T. ) ;
#23427 = CARTESIAN_POINT ( 'NONE',  ( -3.762942409646513386, 4.884725290497410777E-15, -2.999999999999999556 ) ) ;
#23428 = LINE ( 'NONE', #5580, #9754 ) ;
#23429 = EDGE_CURVE ( 'NONE', #22521, #29650, #6085, .T. ) ;
#23430 = ORIENTED_EDGE ( 'NONE', *, *, #8929, .T. ) ;
#23431 = CARTESIAN_POINT ( 'NONE',  ( 4.285194126261599773E-30, 4.979297819079224069E-14, -4.753758587302147731 ) ) ;
#23432 = CARTESIAN_POINT ( 'NONE',  ( 28.57616583554115053, -7.888378049809503523, -2.184956778837684244 ) ) ;
#23433 = ADVANCED_FACE ( 'NONE', ( #12611, #2441 ), #11966, .F. ) ;
#23434 = LINE ( 'NONE', #32995, #2913 ) ;
#23436 = CARTESIAN_POINT ( 'NONE',  ( 107.5356071280131118, -18.60369656572296293, 5.016949557071701093 ) ) ;
#23435 = DIRECTION ( 'NONE',  ( 1.000000000000000000, -0.000000000000000000, -0.000000000000000000 ) ) ;
#23437 = VERTEX_POINT ( 'NONE', #24979 ) ;
#23438 = CARTESIAN_POINT ( 'NONE',  ( -4.557304906975410574, -1.062355717592093463, -3.000000000000000888 ) ) ;
#23439 = ORIENTED_EDGE ( 'NONE', *, *, #82, .T. ) ;
#23440 = CARTESIAN_POINT ( 'NONE',  ( 107.5354615446400857, -18.60157483985592108, 5.015849210584171658 ) ) ;
#23442 = ORIENTED_EDGE ( 'NONE', *, *, #21919, .T. ) ;
#23441 = CARTESIAN_POINT ( 'NONE',  ( 109.1472041058640912, 18.90877050785832836, -4.999054092451833853 ) ) ;
#23443 = ADVANCED_FACE ( 'NONE', ( #5105 ), #20305, .F. ) ;
#23444 = ORIENTED_EDGE ( 'NONE', *, *, #25289, .T. ) ;
#23445 = DIRECTION ( 'NONE',  ( 1.000000000000000000, -0.000000000000000000, -0.000000000000000000 ) ) ;
#23446 = LINE ( 'NONE', #261, #5946 ) ;
#23448 = ORIENTED_EDGE ( 'NONE', *, *, #4266, .T. ) ;
#23447 = DIRECTION ( 'NONE',  ( -0.000000000000000000, -0.000000000000000000, -1.000000000000000000 ) ) ;
#23449 = ORIENTED_EDGE ( 'NONE', *, *, #4277, .T. ) ;
#23450 = CARTESIAN_POINT ( 'NONE',  ( 19.71936553561526395, -17.01520723777865740, -1.753252447592055896 ) ) ;
#23451 = LINE ( 'NONE', #74, #15024 ) ;
#23452 = LINE ( 'NONE', #15927, #25077 ) ;
#23453 = DIRECTION ( 'NONE',  ( 0.000000000000000000, 0.000000000000000000, 1.000000000000000000 ) ) ;
#23454 = CARTESIAN_POINT ( 'NONE',  ( 107.9076248307730594, -16.73918265980126918, 2.181394474119346505 ) ) ;
#23455 = EDGE_CURVE ( 'NONE', #19663, #14569, #32375, .T. ) ;
#23456 = CIRCLE ( 'NONE', #5837, 8.750000000000000000 ) ;
#23457 = ADVANCED_FACE ( 'NONE', ( #12118 ), #20912, .T. ) ;
#23458 = CARTESIAN_POINT ( 'NONE',  ( 18.52596969037426078, -16.42883989518809074, 1.500000000000000444 ) ) ;
#23459 = CARTESIAN_POINT ( 'NONE',  ( 18.69136968068891491, -6.627090290235385872, 2.787782631213004514 ) ) ;
#23460 = DIRECTION ( 'NONE',  ( 0.000000000000000000, 0.000000000000000000, 1.000000000000000000 ) ) ;
#23461 = CARTESIAN_POINT ( 'NONE',  ( 3.090086839179210454, 0.04810462266694562339, 0.6765469099963639099 ) ) ;
#23462 = CIRCLE ( 'NONE', #13822, 5.010000000000000675 ) ;
#23463 = ORIENTED_EDGE ( 'NONE', *, *, #27516, .F. ) ;
#23464 = SPHERICAL_SURFACE ( 'NONE', #22036, 0.5000000000000000000 ) ;
#23465 =( BOUNDED_CURVE ( )  B_SPLINE_CURVE ( 3, ( #30608, #23054, #10013, #20224 ),
 .UNSPECIFIED., .F., .F. ) 
 B_SPLINE_CURVE_WITH_KNOTS ( ( 4, 4 ),
 ( 3.141592653589793116, 6.283185307179586232 ),
 .UNSPECIFIED. ) 
 CURVE ( )  GEOMETRIC_REPRESENTATION_ITEM ( )  RATIONAL_B_SPLINE_CURVE ( ( 1.000000000000000000, 0.3333333333333333703, 0.3333333333333333703, 1.000000000000000000 ) ) 
 REPRESENTATION_ITEM ( '' )  );
#23466 = EDGE_CURVE ( 'NONE', #27801, #13878, #6481, .T. ) ;
#23467 = DIRECTION ( 'NONE',  ( 0.000000000000000000, 0.7071067811865431318, 0.7071067811865520136 ) ) ;
#23468 = ADVANCED_FACE ( 'NONE', ( #24825 ), #31194, .T. ) ;
#23469 = CARTESIAN_POINT ( 'NONE',  ( 12.40148790557316616, 21.49000000000003041, -1.500000000000000000 ) ) ;
#23470 = ORIENTED_EDGE ( 'NONE', *, *, #25928, .F. ) ;
#23471 = CARTESIAN_POINT ( 'NONE',  ( 22.61000000136559507, 2.892927487894327410, -1.570731468192931635 ) ) ;
#23472 = CARTESIAN_POINT ( 'NONE',  ( -8.000050800000000351, 0.000000000000000000, 0.000000000000000000 ) ) ;
#23473 = CYLINDRICAL_SURFACE ( 'NONE', #24751, 0.5000000000000000000 ) ;
#23474 = ORIENTED_EDGE ( 'NONE', *, *, #2840, .T. ) ;
#23475 = DIRECTION ( 'NONE',  ( 0.000000000000000000, 0.000000000000000000, 1.000000000000000000 ) ) ;
#23476 = ADVANCED_FACE ( 'NONE', ( #30858 ), #272, .F. ) ;
#23477 = AXIS2_PLACEMENT_3D ( 'NONE', #5584, #25804, #13232 ) ;
#23478 = VECTOR ( 'NONE', #18760, 1000.000000000000000 ) ;
#23479 = ORIENTED_EDGE ( 'NONE', *, *, #2190, .F. ) ;
#23480 = CARTESIAN_POINT ( 'NONE',  ( 69.10564588818930076, -2.490548236270818894, -1.915219082070890755 ) ) ;
#23481 = SECURITY_CLASSIFICATION_LEVEL ( 'unclassified' ) ;
#23483 = ORIENTED_EDGE ( 'NONE', *, *, #23847, .T. ) ;
#23482 = CARTESIAN_POINT ( 'NONE',  ( 68.59913483175071747, -3.860138077750989272, -2.184958020773514420 ) ) ;
#23484 = EDGE_LOOP ( 'NONE', ( #23183, #31854, #26915, #29666 ) ) ;
#23485 = CARTESIAN_POINT ( 'NONE',  ( -29.85000000000000497, -10.96966150227469505, -11.50000000000000000 ) ) ;
#23486 = EDGE_CURVE ( 'NONE', #2105, #18770, #25645, .T. ) ;
#23487 = ORIENTED_EDGE ( 'NONE', *, *, #5236, .T. ) ;
#23488 = VECTOR ( 'NONE', #31335, 1000.000000000000227 ) ;
#23489 = DIRECTION ( 'NONE',  ( 0.000000000000000000, -0.9510565162951502005, -0.3090169943749573322 ) ) ;
#23491 = EDGE_LOOP ( 'NONE', ( #7531, #32728, #13718, #32418 ) ) ;
#23490 = CARTESIAN_POINT ( 'NONE',  ( -2.249956573341760357, 1.323625320507108460, 3.284597389080124774 ) ) ;
#23492 = CARTESIAN_POINT ( 'NONE',  ( 13.24811108103750712, 6.657149145102930987, 1.050000000000000266 ) ) ;
#23493 = CARTESIAN_POINT ( 'NONE',  ( 108.0518026804759018, -18.81530782858648720, 3.657879498689815545 ) ) ;
#23494 = CARTESIAN_POINT ( 'NONE',  ( 26.34939556550226314, 19.05368625490716639, -2.334455007174267571 ) ) ;
#23495 = CARTESIAN_POINT ( 'NONE',  ( 0.1606232872998201999, 10.41111328664652014, -2.144970499002631037 ) ) ;
#23496 = ORIENTED_EDGE ( 'NONE', *, *, #28790, .T. ) ;
#23497 = CARTESIAN_POINT ( 'NONE',  ( -3.850050799999999995, -2.853674364686378695, -1.549418761218566809 ) ) ;
#23498 = CARTESIAN_POINT ( 'NONE',  ( -2.715578036410642326, -0.5452877988936790654, -1.748464050203881737 ) ) ;
#23499 = CARTESIAN_POINT ( 'NONE',  ( 18.64064227445962274, -7.194120883406243117, -1.873789191072353644 ) ) ;
#23500 = CARTESIAN_POINT ( 'NONE',  ( -0.9232102171129827894, 0.000000000000000000, -4.522129901861166701 ) ) ;
#23501 = EDGE_CURVE ( 'NONE', #30729, #4093, #23160, .T. ) ;
#23502 = DIRECTION ( 'NONE',  ( 0.000000000000000000, -0.9063077870366526012, 0.4226182617406936126 ) ) ;
#23503 = CARTESIAN_POINT ( 'NONE',  ( 110.5397548702477764, 21.00556809464028873, 2.806473568333437196 ) ) ;
#23504 = CARTESIAN_POINT ( 'NONE',  ( 0.6728002192015012373, -7.058361986489737561, -5.823680980849895050 ) ) ;
#23505 = CARTESIAN_POINT ( 'NONE',  ( 21.70556107702209303, -21.76510136446067278, 1.556570398778031716 ) ) ;
#23506 = VECTOR ( 'NONE', #26302, 1000.000000000000114 ) ;
#23507 = EDGE_CURVE ( 'NONE', #7400, #140, #30007, .T. ) ;
#23508 = CARTESIAN_POINT ( 'NONE',  ( -3.762550801365593500, 2.228590825266444142, 2.752080473201636845 ) ) ;
#23509 = ORIENTED_EDGE ( 'NONE', *, *, #20060, .T. ) ;
#23510 = CARTESIAN_POINT ( 'NONE',  ( -4.754531657079158258, -3.105402419394638791, 0.9198621039125867149 ) ) ;
#23511 = AXIS2_PLACEMENT_3D ( 'NONE', #5296, #21177, #18829 ) ;
#23512 = CARTESIAN_POINT ( 'NONE',  ( 9.331062908042598636, 15.00000000000002132, -4.612695725900422872 ) ) ;
#23513 = FACE_OUTER_BOUND ( 'NONE', #14676, .T. ) ;
#23514 = CARTESIAN_POINT ( 'NONE',  ( 10.90710808013595923, -12.60204455941995150, 1.000000000000000000 ) ) ;
#23515 = EDGE_LOOP ( 'NONE', ( #18146, #25397, #27492, #14055 ) ) ;
#23516 = CARTESIAN_POINT ( 'NONE',  ( 3.499999999999999556, 6.704570150426983233, 2.172265885002680808 ) ) ;
#23517 = ADVANCED_FACE ( 'NONE', ( #28658 ), #22964, .T. ) ;
#23518 = EDGE_LOOP ( 'NONE', ( #26182, #6814 ) ) ;
#23519 = CARTESIAN_POINT ( 'NONE',  ( 10.00000000000000178, -1.115095498423344988, 4.884328206559834129 ) ) ;
#23520 = APPROVAL_DATE_TIME ( #3494, #29663 ) ;
#23521 = AXIS2_PLACEMENT_3D ( 'NONE', #31138, #8224, #16229 ) ;
#23522 = VECTOR ( 'NONE', #26398, 1000.000000000000000 ) ;
#23523 = CARTESIAN_POINT ( 'NONE',  ( 54.97647335323577522, -6.479429838881364923, 4.033870040929349976 ) ) ;
#23525 = EDGE_CURVE ( 'NONE', #2806, #4621, #9143, .T. ) ;
#23524 = CIRCLE ( 'NONE', #11232, 2.999999999999998668 ) ;
#23526 = DIRECTION ( 'NONE',  ( -0.000000000000000000, -0.000000000000000000, -1.000000000000000000 ) ) ;
#23527 = AXIS2_PLACEMENT_3D ( 'NONE', #19099, #26781, #1715 ) ;
#23528 = CARTESIAN_POINT ( 'NONE',  ( 6.038145077921539539, 8.106170535363485641, -2.472816103755169248 ) ) ;
#23529 = VERTEX_POINT ( 'NONE', #8087 ) ;
#23530 = CARTESIAN_POINT ( 'NONE',  ( 3.063284526839890276, 7.360373001730978082, -4.729683950898788680 ) ) ;
#23531 = LINE ( 'NONE', #3648, #8095 ) ;
#23532 = CARTESIAN_POINT ( 'NONE',  ( 21.73500000136559507, 3.156283516753366047, 0.9349337715887203748 ) ) ;
#23533 = AXIS2_PLACEMENT_3D ( 'NONE', #13390, #23609, #21270 ) ;
#23535 = ORIENTED_EDGE ( 'NONE', *, *, #8929, .F. ) ;
#23534 = CARTESIAN_POINT ( 'NONE',  ( 9.284228442262035585, 0.2197421434176238808, -1.042917449647795758 ) ) ;
#23536 = CARTESIAN_POINT ( 'NONE',  ( -3.562550801365592879, -2.752080473201636845, 2.228590825266444586 ) ) ;
#23537 = DIRECTION ( 'NONE',  ( -1.000000000000000000, -0.000000000000000000, -0.000000000000000000 ) ) ;
#23538 = CARTESIAN_POINT ( 'NONE',  ( 85.08237158773125941, -5.954015309899377328, -2.787781826237480054 ) ) ;
#23539 = ORIENTED_EDGE ( 'NONE', *, *, #15787, .F. ) ;
#23540 = ORIENTED_EDGE ( 'NONE', *, *, #29969, .T. ) ;
#23541 = EDGE_CURVE ( 'NONE', #32276, #22947, #28504, .T. ) ;
#23542 = DIRECTION ( 'NONE',  ( 0.000000000000000000, 0.000000000000000000, 1.000000000000000000 ) ) ;
#23543 = CARTESIAN_POINT ( 'NONE',  ( 1.624999999999999778, 7.958834565716766285, 7.593217523260609170 ) ) ;
#23544 = EDGE_CURVE ( 'NONE', #12294, #20676, #5609, .T. ) ;
#23545 = CIRCLE ( 'NONE', #32656, 8.750000000000000000 ) ;
#23546 = CARTESIAN_POINT ( 'NONE',  ( 25.38252866315519896, -17.53427985683313040, 1.078182501543538230 ) ) ;
#23547 = AXIS2_PLACEMENT_3D ( 'NONE', #28236, #20881, #15361 ) ;
#23548 = CARTESIAN_POINT ( 'NONE',  ( 2.274274201625327230, 1.975651141462238858, 10.82112760146736896 ) ) ;
#23549 = CARTESIAN_POINT ( 'NONE',  ( 2.786096336624678926, -9.516507749480087597, 2.300561732651082103 ) ) ;
#23550 = CIRCLE ( 'NONE', #19817, 2.999999999999998668 ) ;
#23551 = CARTESIAN_POINT ( 'NONE',  ( 3.744708216408842549, 0.000000000000000000, -1.000000000000000000 ) ) ;
#23552 = CARTESIAN_POINT ( 'NONE',  ( 29.18862856207581302, -8.152784366139066208, 1.169950487266440575 ) ) ;
#23553 = ORIENTED_EDGE ( 'NONE', *, *, #10220, .F. ) ;
#23554 = CARTESIAN_POINT ( 'NONE',  ( -57.39048296612208588, -3.170628888746132468, 5.871858320049880398 ) ) ;
#23555 = CIRCLE ( 'NONE', #4364, 0.5000000000000004441 ) ;
#23556 = ORIENTED_EDGE ( 'NONE', *, *, #2731, .F. ) ;
#23557 = APPROVAL_STATUS ( 'not_yet_approved' ) ;
#23558 = CARTESIAN_POINT ( 'NONE',  ( 69.18703749905368738, -4.112663945013687261, 4.522129901861162260 ) ) ;
#23559 = ORIENTED_EDGE ( 'NONE', *, *, #7386, .T. ) ;
#23560 = DIRECTION ( 'NONE',  ( 1.000000000000000000, -8.574039729943018344E-17, -0.000000000000000000 ) ) ;
#23561 = VERTEX_POINT ( 'NONE', #29146 ) ;
#23562 = CARTESIAN_POINT ( 'NONE',  ( 5.323856294847530535, 1.496472198897159434, 3.277537277937063731 ) ) ;
#23564 = VERTEX_POINT ( 'NONE', #29653 ) ;
#23563 = CARTESIAN_POINT ( 'NONE',  ( 54.94664600394312970, -5.401721570094858649, -4.053847711501203932 ) ) ;
#23565 = VECTOR ( 'NONE', #9191, 1000.000000000000114 ) ;
#23566 = ORIENTED_EDGE ( 'NONE', *, *, #19952, .F. ) ;
#23567 = CARTESIAN_POINT ( 'NONE',  ( -5.712550801365593678, -1.088641768524163611, -3.675193018007245627 ) ) ;
#23568 = CONICAL_SURFACE ( 'NONE', #9142, 3.024999999999999911, 0.7853981633974520538 ) ;
#23569 = CARTESIAN_POINT ( 'NONE',  ( 8.045354371110260416, -1.465502149859543524, 1.500000000000000000 ) ) ;
#23570 = AXIS2_PLACEMENT_3D ( 'NONE', #19650, #17117, #27330 ) ;
#23571 = DIRECTION ( 'NONE',  ( -1.000000000000000000, 0.000000000000000000, 0.000000000000000000 ) ) ;
#23573 = ORIENTED_EDGE ( 'NONE', *, *, #25211, .T. ) ;
#23572 = CARTESIAN_POINT ( 'NONE',  ( 18.00993182317604990, 14.21018869494618819, -1.500000000000000000 ) ) ;
#23574 = CARTESIAN_POINT ( 'NONE',  ( 107.5894750467910228, -19.38218566293085843, 3.705121501346941404 ) ) ;
#23575 = AXIS2_PLACEMENT_3D ( 'NONE', #13891, #29142, #6229 ) ;
#23576 = CARTESIAN_POINT ( 'NONE',  ( 11.83510569430203319, 5.122261773727990075, 1.500000000000000000 ) ) ;
#23577 = CARTESIAN_POINT ( 'NONE',  ( 6.168724859680794204, -18.37409005221297775, 1.500000000000238032 ) ) ;
#23578 = DIRECTION ( 'NONE',  ( -1.000000000000000000, -0.000000000000000000, -0.000000000000000000 ) ) ;
#23579 = CIRCLE ( 'NONE', #11871, 5.009999999999999787 ) ;
#23580 = CYLINDRICAL_SURFACE ( 'NONE', #26701, 11.00000000000000000 ) ;
#23581 = EDGE_CURVE ( 'NONE', #23867, #30399, #1553, .T. ) ;
#23583 = ORIENTED_EDGE ( 'NONE', *, *, #29109, .T. ) ;
#23582 = DIRECTION ( 'NONE',  ( 1.000000000000000000, -8.574039729943018344E-17, -0.000000000000000000 ) ) ;
#23584 = CARTESIAN_POINT ( 'NONE',  ( -23.54713438637982748, 5.934235225036485595, 7.654118351624816796 ) ) ;
#23585 = EDGE_CURVE ( 'NONE', #26130, #5903, #14388, .T. ) ;
#23586 = VECTOR ( 'NONE', #13489, 1000.000000000000114 ) ;
#23587 = TOROIDAL_SURFACE ( 'NONE', #40, 6.923700951379999857, 9.000000000000001776 ) ;
#23588 = CARTESIAN_POINT ( 'NONE',  ( -28.03779898944224058, 16.55826090817324925, 1.819008976926004717 ) ) ;
#23589 = CARTESIAN_POINT ( 'NONE',  ( 25.04750000273118715, 0.7685399846772009713, -2.594547506269381909 ) ) ;
#23590 = CARTESIAN_POINT ( 'NONE',  ( 7.064632879756603145, -0.8180878109961264855, -8.711672189281433276 ) ) ;
#23591 = CARTESIAN_POINT ( 'NONE',  ( 101.8343541425947052, -4.513224517051876106, -3.236291054900928721 ) ) ;
#23592 = CARTESIAN_POINT ( 'NONE',  ( -3.038890739117042994, -0.3712649131886756049, -1.487764840819184142 ) ) ;
#23593 = CIRCLE ( 'NONE', #15607, 4.000000000000001776 ) ;
#23594 = CARTESIAN_POINT ( 'NONE',  ( -53.35155202832373078, 4.402097243136373628, 5.049999999999999822 ) ) ;
#23595 = TOROIDAL_SURFACE ( 'NONE', #3335, 6.818740222761507042, 0.5000000000000000000 ) ;
#23596 = AXIS2_PLACEMENT_3D ( 'NONE', #8496, #21861, #18544 ) ;
#23597 = CARTESIAN_POINT ( 'NONE',  ( 7.249760686538667009, -7.530955069117533540, 2.741043480754901118 ) ) ;
#23598 = ORIENTED_EDGE ( 'NONE', *, *, #23585, .T. ) ;
#23599 = CIRCLE ( 'NONE', #27877, 1.800000000000015810 ) ;
#23600 = AXIS2_PLACEMENT_3D ( 'NONE', #7691, #20877, #7498 ) ;
#23601 = CARTESIAN_POINT ( 'NONE',  ( 18.06874303396712023, -21.14907373873896645, 1.751201621425063193 ) ) ;
#23602 = LINE ( 'NONE', #20776, #25070 ) ;
#23603 = CARTESIAN_POINT ( 'NONE',  ( 6.880160201030087741, -8.703862158141008720, 0.6895871680713464569 ) ) ;
#23606 = CARTESIAN_POINT ( 'NONE',  ( 107.9965106981324681, -18.01911703775898488, 5.137942289311619781 ) ) ;
#23605 = CARTESIAN_POINT ( 'NONE',  ( 0.000000000000000000, 0.000000000000000000, 0.000000000000000000 ) ) ;
#23604 = CONICAL_SURFACE ( 'NONE', #19877, 2.524999999999999467, 0.7853981633974472798 ) ;
#23607 = ORIENTED_EDGE ( 'NONE', *, *, #27535, .T. ) ;
#23608 = AXIS2_PLACEMENT_3D ( 'NONE', #29670, #2075, #32184 ) ;
#23609 = DIRECTION ( 'NONE',  ( -1.000000000000000000, 0.000000000000000000, 0.000000000000000000 ) ) ;
#23610 = ORIENTED_EDGE ( 'NONE', *, *, #12194, .T. ) ;
#23611 = CYLINDRICAL_SURFACE ( 'NONE', #11875, 0.5000000000000008882 ) ;
#23613 = ORIENTED_EDGE ( 'NONE', *, *, #32400, .F. ) ;
#23612 = DIRECTION ( 'NONE',  ( 0.000000000000000000, 1.000000000000000000, 0.000000000000000000 ) ) ;
#23614 = EDGE_LOOP ( 'NONE', ( #5594, #21935, #19553, #30548 ) ) ;
#23615 = CARTESIAN_POINT ( 'NONE',  ( 101.7221769401408551, -2.897900707893039662, 3.993434276071444078 ) ) ;
#23616 = CARTESIAN_POINT ( 'NONE',  ( 4.749760686538667009, 2.741043480754926875, 7.530955069117522882 ) ) ;
#23617 = EDGE_CURVE ( 'NONE', #25632, #4026, #4074, .T. ) ;
#23619 = VERTEX_POINT ( 'NONE', #1403 ) ;
#23618 = CARTESIAN_POINT ( 'NONE',  ( 6.880159396099836400, -3.754731129947842749, 7.882559112973148707 ) ) ;
#23620 = VECTOR ( 'NONE', #29076, 1000.000000000000000 ) ;
#23621 = ORIENTED_EDGE ( 'NONE', *, *, #7007, .T. ) ;
#23622 = LINE ( 'NONE', #18605, #9559 ) ;
#23623 = VECTOR ( 'NONE', #18698, 1000.000000000000000 ) ;
#23624 = CARTESIAN_POINT ( 'NONE',  ( 0.000000000000000000, -9.680994141368802985, 5.222868219166823422 ) ) ;
#23625 = AXIS2_PLACEMENT_3D ( 'NONE', #10056, #30472, #15398 ) ;
#23626 = CARTESIAN_POINT ( 'NONE',  ( 24.38441422956697124, -17.22282062799600766, -1.000000000000000000 ) ) ;
#23627 = CARTESIAN_POINT ( 'NONE',  ( 107.9481247343239687, -17.32237119582743290, -4.511855742419091264 ) ) ;
#23628 = CARTESIAN_POINT ( 'NONE',  ( 3.063284526839887167, 3.174628368996073924, 8.152713396088772768 ) ) ;
#23629 = VECTOR ( 'NONE', #20580, 1000.000000000000227 ) ;
#23630 = AXIS2_PLACEMENT_3D ( 'NONE', #24796, #17764, #27972 ) ;
#23631 = DIRECTION ( 'NONE',  ( 0.000000000000000000, 0.000000000000000000, 1.000000000000000000 ) ) ;
#23632 = CARTESIAN_POINT ( 'NONE',  ( 0.5291895307230495282, -6.519846571640815824, 1.500000000000000444 ) ) ;
#23633 = CARTESIAN_POINT ( 'NONE',  ( 8.528645601772334217, -0.5000000000000011102, 1.500000000000000000 ) ) ;
#23634 = VECTOR ( 'NONE', #21340, 1000.000000000000000 ) ;
#23635 = AXIS2_PLACEMENT_3D ( 'NONE', #17411, #30144, #21918 ) ;
#23636 = CARTESIAN_POINT ( 'NONE',  ( -3.100050800000000439, -2.983565686104819648, -0.3135853898029605791 ) ) ;
#23637 = CARTESIAN_POINT ( 'NONE',  ( 2.802272078496832464, -0.3634031030573117715, 1.485394228827260577 ) ) ;
#23638 = EDGE_LOOP ( 'NONE', ( #20868, #23496, #17296, #7905, #7575 ) ) ;
#23639 = CARTESIAN_POINT ( 'NONE',  ( 7.064423637759001728, -3.647351267792851903, -7.953573330858871415 ) ) ;
#23640 = EDGE_CURVE ( 'NONE', #21723, #6904, #5428, .T. ) ;
#23641 = CARTESIAN_POINT ( 'NONE',  ( 107.3512941337518498, 17.37330583879708001, 3.589055591124487687 ) ) ;
#23642 = CYLINDRICAL_SURFACE ( 'NONE', #30626, 2.999999999999999112 ) ;
#23643 = VERTEX_POINT ( 'NONE', #31488 ) ;
#23644 = CARTESIAN_POINT ( 'NONE',  ( 21.79750000136559507, 2.363507492473148286, 1.913930629741525058 ) ) ;
#23645 = AXIS2_PLACEMENT_3D ( 'NONE', #28351, #18643, #13456 ) ;
#23646 = AXIS2_PLACEMENT_3D ( 'NONE', #13157, #16158, #10820 ) ;
#23647 = CARTESIAN_POINT ( 'NONE',  ( 25.34177696560086446, -2.134796180801955323, 1.506068310576387015 ) ) ;
#23648 = EDGE_CURVE ( 'NONE', #2670, #7219, #17149, .T. ) ;
#23649 = DIRECTION ( 'NONE',  ( -1.000000000000000000, 0.000000000000000000, 0.000000000000000000 ) ) ;
#23651 = ORIENTED_EDGE ( 'NONE', *, *, #27552, .T. ) ;
#23650 = AXIS2_PLACEMENT_3D ( 'NONE', #15443, #25653, #2773 ) ;
#23652 = CARTESIAN_POINT ( 'NONE',  ( 0.8612084954131845604, -8.440632053510048749, -1.499999999999999556 ) ) ;
#23653 = EDGE_LOOP ( 'NONE', ( #18713, #4700, #11452, #8800 ) ) ;
#23654 = VECTOR ( 'NONE', #4997, 1000.000000000000000 ) ;
#23655 = VECTOR ( 'NONE', #33097, 1000.000000000000000 ) ;
#23656 = VERTEX_POINT ( 'NONE', #19459 ) ;
#23657 = LINE ( 'NONE', #31211, #15056 ) ;
#23658 = ADVANCED_FACE ( 'NONE', ( #11735 ), #14240, .F. ) ;
#23659 = DATE_TIME_ROLE ( 'classification_date' ) ;
#23661 = EDGE_LOOP ( 'NONE', ( #22251, #11564, #25045 ) ) ;
#23660 = CARTESIAN_POINT ( 'NONE',  ( 22.86000000000000298, 1.573300977624590313, -1.942864903642426144 ) ) ;
#23662 = EDGE_LOOP ( 'NONE', ( #9909, #2036, #2163, #11715, #27251 ) ) ;
#23663 = DIRECTION ( 'NONE',  ( 8.574039729943018344E-17, 1.000000000000000000, 0.000000000000000000 ) ) ;
#23664 = VERTEX_POINT ( 'NONE', #21773 ) ;
#23666 = VERTEX_POINT ( 'NONE', #6733 ) ;
#23665 = CARTESIAN_POINT ( 'NONE',  ( 19.01480233880980819, -3.011762293215293429, -0.07017451552781921176 ) ) ;
#23667 = CARTESIAN_POINT ( 'NONE',  ( 29.18953645666586638, -9.308308156628569918, 0.07017451552781803215 ) ) ;
#23668 = CARTESIAN_POINT ( 'NONE',  ( 5.885541615502091872, 1.090540896198919585, -8.322568858718543794 ) ) ;
#23669 = EDGE_CURVE ( 'NONE', #8466, #25541, #13846, .T. ) ;
#23670 = DIRECTION ( 'NONE',  ( 0.1437473352845043406, 0.000000000000000000, -0.9896144216807899463 ) ) ;
#23671 = ADVANCED_FACE ( 'NONE', ( #14088 ), #1702, .T. ) ;
#23672 = CARTESIAN_POINT ( 'NONE',  ( 102.6609843814833027, -1.982062027707616192, 4.522129901861162260 ) ) ;
#23673 = FACE_OUTER_BOUND ( 'NONE', #22265, .T. ) ;
#23674 = ORIENTED_EDGE ( 'NONE', *, *, #19757, .T. ) ;
#23675 =( BOUNDED_SURFACE ( )  B_SPLINE_SURFACE ( 3, 2, ( 
 ( #21537, #31744, #8962 ),
 ( #16660, #9125, #32053 ),
 ( #4484, #21839, #19354 ),
 ( #29557, #16985, #13976 ),
 ( #32244, #26872, #6299 ),
 ( #9462, #27185, #6644 ) ),
 .UNSPECIFIED., .F., .F., .F. ) 
 B_SPLINE_SURFACE_WITH_KNOTS ( ( 4, 2, 4 ),
 ( 3, 3 ),
 ( 6.884163014324157004, 7.369072324149319897, 7.853981633974482790 ),
 ( 0.000000000000000000, 1.000000000000000000 ),
 .UNSPECIFIED. ) 
 GEOMETRIC_REPRESENTATION_ITEM ( )  RATIONAL_B_SPLINE_SURFACE ( (
 ( 1.000000000000000000, 0.8123215895924648100, 1.000000000000000000),
 ( 1.000000000000000000, 0.8591172521900213299, 1.000000000000000000),
 ( 1.000000000000000000, 0.9088222585364075234, 1.000000000000000000),
 ( 1.000000000000000000, 0.9794174349135026381, 1.000000000000000000),
 ( 1.000000000000000000, 1.000375673120273978, 1.000000000000000000),
 ( 1.000000000000000000, 1.000000000000000000, 1.000000000000000000) ) ) 
 REPRESENTATION_ITEM ( '' )  SURFACE ( )  );
#23676 = VECTOR ( 'NONE', #51, 1000.000000000000114 ) ;
#23677 = FACE_OUTER_BOUND ( 'NONE', #3490, .T. ) ;
#23678 = CARTESIAN_POINT ( 'NONE',  ( 109.7266016284592069, 16.47760998941503630, 5.471072653610983494 ) ) ;
#23679 = CARTESIAN_POINT ( 'NONE',  ( 69.14957877370493122, -7.691922716131041504, -1.169951105765761223 ) ) ;
#23680 = CARTESIAN_POINT ( 'NONE',  ( 2.514244811554134262, -8.107161948574434494E-17, -1.252246291852655125 ) ) ;
#23681 = VECTOR ( 'NONE', #27016, 1000.000000000000000 ) ;
#23682 = VECTOR ( 'NONE', #27794, 1000.000000000000000 ) ;
#23683 = CIRCLE ( 'NONE', #3933, 0.4499999999999992339 ) ;
#23684 = CARTESIAN_POINT ( 'NONE',  ( 24.00111451137534146, -6.623356326098185375E-16, -2.499999999999998224 ) ) ;
#23685 = CARTESIAN_POINT ( 'NONE',  ( 10.55147673363119232, 2.376879293651063652, 4.116875700062091248 ) ) ;
#23686 = PLANE ( 'NONE',  #19892 ) ;
#23687 = DIRECTION ( 'NONE',  ( -5.361488761196516318E-16, 1.000000000000000000, 0.000000000000000000 ) ) ;
#23688 = LOCAL_TIME ( 16, 7, 10.00000000000000000, #19202 ) ;
#23689 = CARTESIAN_POINT ( 'NONE',  ( -25.41317123495379704, 3.720325412122147846, 1.500000000000000000 ) ) ;
#23690 = CARTESIAN_POINT ( 'NONE',  ( -4.812550801365592434, 1.828967928396027176, -3.368539882008727115 ) ) ;
#23691 = VERTEX_POINT ( 'NONE', #28988 ) ;
#23692 = EDGE_CURVE ( 'NONE', #23643, #299, #20398, .T. ) ;
#23693 = CARTESIAN_POINT ( 'NONE',  ( -5.700050800000000528, -0.3135853898029607456, 2.983565686104819648 ) ) ;
#23694 = CARTESIAN_POINT ( 'NONE',  ( 107.9802527803230419, -17.78500706576073753, 4.325704939602341703 ) ) ;
#23695 = CARTESIAN_POINT ( 'NONE',  ( 5.377543748152549874, -4.007137495034861274, 6.940565734314584567 ) ) ;
#23696 = CARTESIAN_POINT ( 'NONE',  ( 10.90710808056855363, -12.60204455863645201, 1.499999999999860112 ) ) ;
#23697 = VERTEX_POINT ( 'NONE', #13898 ) ;
#23698 = DIRECTION ( 'NONE',  ( -1.000000000000000000, 0.000000000000000000, -0.000000000000000000 ) ) ;
#23699 = VECTOR ( 'NONE', #20534, 999.9999999999998863 ) ;
#23700 = VECTOR ( 'NONE', #32735, 1000.000000000000000 ) ;
#23701 = ORIENTED_EDGE ( 'NONE', *, *, #19281, .T. ) ;
#23702 = CARTESIAN_POINT ( 'NONE',  ( -3.222375984151267581, 0.000000000000000000, -1.000000000000000000 ) ) ;
#23703 = COORDINATED_UNIVERSAL_TIME_OFFSET ( 0, 0, .AHEAD. ) ;
#23704 = CARTESIAN_POINT ( 'NONE',  ( 84.99303864845812484, -4.506833362056713810, 4.312042181588143563 ) ) ;
#23705 = VECTOR ( 'NONE', #4905, 1000.000000000000000 ) ;
#23706 = ADVANCED_FACE ( 'NONE', ( #16271 ), #28922, .F. ) ;
#23707 = CARTESIAN_POINT ( 'NONE',  ( 9.288460890967574102, 0.2259157356912394610, 1.047117114142813499 ) ) ;
#23708 = DIRECTION ( 'NONE',  ( -8.541412920197219815E-17, -0.9961946980917455452, 0.08715574274765799934 ) ) ;
#23709 = ORIENTED_EDGE ( 'NONE', *, *, #3223, .T. ) ;
#23710 = EDGE_CURVE ( 'NONE', #16905, #25765, #24110, .T. ) ;
#23711 = CC_DESIGN_APPROVAL ( #13290, ( #25774 ) ) ;
#23712 = DIRECTION ( 'NONE',  ( 0.000000000000000000, -0.000000000000000000, -1.000000000000000000 ) ) ;
#23713 = EDGE_CURVE ( 'NONE', #14512, #26215, #9051, .T. ) ;
#23714 = CARTESIAN_POINT ( 'NONE',  ( -1.265925305626641768E-16, -1.476463073999604969, -4.787500056513382063 ) ) ;
#23715 = CARTESIAN_POINT ( 'NONE',  ( 21.48500000136559507, 0.9349337715887185984, -3.156283516753368268 ) ) ;
#23717 = ORIENTED_EDGE ( 'NONE', *, *, #392, .T. ) ;
#23716 = CARTESIAN_POINT ( 'NONE',  ( 108.2737967297448307, 19.70276815113069091, -2.517673782553874862 ) ) ;
#23718 = CARTESIAN_POINT ( 'NONE',  ( -4.012550801365593500, 1.828967928396027176, -3.368539882008727115 ) ) ;
#23719 = CARTESIAN_POINT ( 'NONE',  ( -1.394036994807634510E-16, -1.625881193364727917, 4.467071865485467086 ) ) ;
#23720 = CARTESIAN_POINT ( 'NONE',  ( 41.35536016469566789, -7.892720495271999148, -2.184957211637544638 ) ) ;
#23721 = ORIENTED_EDGE ( 'NONE', *, *, #9604, .F. ) ;
#23722 = VERTEX_POINT ( 'NONE', #17425 ) ;
#23723 = AXIS2_PLACEMENT_3D ( 'NONE', #15665, #25874, #2994 ) ;
#23724 = CARTESIAN_POINT ( 'NONE',  ( 0.1606233060821305736, -4.384181225617423294, 9.683549581721083044 ) ) ;
#23725 = CARTESIAN_POINT ( 'NONE',  ( -33.81874022276151237, 19.50000000000000000, 1.977928362984241017 ) ) ;
#23726 = CARTESIAN_POINT ( 'NONE',  ( -2.408800074497548849, -5.498703686517900202, 5.485967528433935314 ) ) ;
#23727 = CARTESIAN_POINT ( 'NONE',  ( 41.43709133142961321, -4.769546740945158625, 4.522129901861162260 ) ) ;
#23728 = ADVANCED_FACE ( 'NONE', ( #1909 ), #14587, .F. ) ;
#23729 = DIRECTION ( 'NONE',  ( -1.000000000000000000, -0.000000000000000000, 0.000000000000000000 ) ) ;
#23730 = CC_DESIGN_PERSON_AND_ORGANIZATION_ASSIGNMENT ( #12335, #2337, ( #2373 ) ) ;
#23731 = FACE_OUTER_BOUND ( 'NONE', #32354, .T. ) ;
#23732 = CARTESIAN_POINT ( 'NONE',  ( -3.687550801365593323, -2.752080473201636845, 2.228590825266444586 ) ) ;
#23733 = LOCAL_TIME ( 16, 7, 10.00000000000000000, #10108 ) ;
#23734 = DIRECTION ( 'NONE',  ( -1.000000000000000000, 0.000000000000000000, 0.000000000000000000 ) ) ;
#23735 = CARTESIAN_POINT ( 'NONE',  ( 41.35712849199996555, -8.497574858407944021, 0.4367667074078382949 ) ) ;
#23736 = ORIENTED_EDGE ( 'NONE', *, *, #13809, .F. ) ;
#23737 = CARTESIAN_POINT ( 'NONE',  ( 3.499999999999999556, 0.005878491403554959860, -7.047692205288322853 ) ) ;
#23738 = ORIENTED_EDGE ( 'NONE', *, *, #18407, .T. ) ;
#23739 = PERSON_AND_ORGANIZATION ( #6766, #25292 ) ;
#23740 = CARTESIAN_POINT ( 'NONE',  ( 102.4232086143177582, -3.998587120485036728, 3.995336663074131600 ) ) ;
#23741 = EDGE_CURVE ( 'NONE', #23437, #24462, #30310, .T. ) ;
#23742 = VECTOR ( 'NONE', #4687, 1000.000000000000000 ) ;
#23743 = CARTESIAN_POINT ( 'NONE',  ( 8.896977825536888318, -11.14034974407042711, -0.9999999999999997780 ) ) ;
#23744 = EDGE_LOOP ( 'NONE', ( #15759, #27189, #1539, #27529 ) ) ;
#23745 = FACE_OUTER_BOUND ( 'NONE', #9786, .T. ) ;
#23746 = ORIENTED_EDGE ( 'NONE', *, *, #23544, .T. ) ;
#23747 = VERTEX_POINT ( 'NONE', #12576 ) ;
#23748 = CARTESIAN_POINT ( 'NONE',  ( -15.06907680150157702, -21.88241439596534121, 1.340913934978399613 ) ) ;
#23749 = CARTESIAN_POINT ( 'NONE',  ( -4.662550801365592967, 3.521866450007987037, 0.3701630799359328372 ) ) ;
#23750 = DIRECTION ( 'NONE',  ( -0.000000000000000000, -0.08715574274766135776, -0.9961946980917452121 ) ) ;
#23751 = CARTESIAN_POINT ( 'NONE',  ( 1.073830709372254999, -2.621082672957672166, -1.760914646145874674 ) ) ;
#23753 = ORIENTED_EDGE ( 'NONE', *, *, #12692, .T. ) ;
#23752 = CARTESIAN_POINT ( 'NONE',  ( 1.787149210215136508, -1.031811077599730231, -1.500000000000000000 ) ) ;
#23754 = CARTESIAN_POINT ( 'NONE',  ( -5.437550801365592434, 1.088641768524161613, 3.675193018007247403 ) ) ;
#23755 = CARTESIAN_POINT ( 'NONE',  ( 21.51801198755429922, 16.55905037279375591, 1.500000000000234257 ) ) ;
#23756 = CARTESIAN_POINT ( 'NONE',  ( 0.000000000000000000, 0.000000000000000000, 0.000000000000000000 ) ) ;
#23757 = PLANE ( 'NONE',  #3338 ) ;
#23758 = LOCAL_TIME ( 16, 7, 10.00000000000000000, #19629 ) ;
#23760 = VERTEX_POINT ( 'NONE', #32985 ) ;
#23759 = DIRECTION ( 'NONE',  ( -1.000000000000000000, -0.000000000000000000, -0.000000000000000000 ) ) ;
#23761 = CARTESIAN_POINT ( 'NONE',  ( -25.76785678020393178, 4.411679249915887446, 2.134707912735335888 ) ) ;
#23762 = CARTESIAN_POINT ( 'NONE',  ( 23.42250000273118715, 1.291182301015469047, 2.378061970571981654 ) ) ;
#23763 = EDGE_CURVE ( 'NONE', #32887, #5204, #24326, .T. ) ;
#23764 = CARTESIAN_POINT ( 'NONE',  ( -17.09300656982994937, 9.321674377477680906, 2.002134007589346343 ) ) ;
#23765 = CARTESIAN_POINT ( 'NONE',  ( 46.69789307159569347, 25.15383447853596621, 4.629213727441585213 ) ) ;
#23766 = DIRECTION ( 'NONE',  ( 0.000000000000000000, 0.000000000000000000, -1.000000000000000000 ) ) ;
#23767 = CARTESIAN_POINT ( 'NONE',  ( 2.795120465739999727, -2.298374178342462049, 9.482538569678554907 ) ) ;
#23768 = CARTESIAN_POINT ( 'NONE',  ( -18.35000000000000142, -10.96966150227469505, -1.500000000000000000 ) ) ;
#23769 = CARTESIAN_POINT ( 'NONE',  ( -5.687550801365593323, 2.752080473201636845, -2.228590825266444142 ) ) ;
#23770 = ORIENTED_EDGE ( 'NONE', *, *, #10314, .T. ) ;
#23771 = CARTESIAN_POINT ( 'NONE',  ( 19.72213158284570156, -21.49998897973738821, 1.523512165873458279 ) ) ;
#23772 = DIRECTION ( 'NONE',  ( 0.000000000000000000, 0.000000000000000000, 1.000000000000000000 ) ) ;
#23773 = CARTESIAN_POINT ( 'NONE',  ( 2.274274201620948510, 9.915734732518576067, -4.762163868927066446 ) ) ;
#23775 = CARTESIAN_POINT ( 'NONE',  ( 107.4499334670178143, -17.35837986862966176, 4.517176980674937781 ) ) ;
#23774 = DIRECTION ( 'NONE',  ( 0.000000000000000000, 0.000000000000000000, 1.000000000000000000 ) ) ;
#23776 = EDGE_CURVE ( 'NONE', #21228, #10967, #11212, .T. ) ;
#23777 = ORIENTED_EDGE ( 'NONE', *, *, #4515, .F. ) ;
#23778 = EDGE_CURVE ( 'NONE', #6604, #32678, #15070, .T. ) ;
#23779 = CARTESIAN_POINT ( 'NONE',  ( 0.000000000000000000, 7.008469740302810891, -0.7425307242147067832 ) ) ;
#23780 = VERTEX_POINT ( 'NONE', #27469 ) ;
#23781 = DIRECTION ( 'NONE',  ( 1.000000000000000000, 0.000000000000000000, 0.000000000000000000 ) ) ;
#23782 = EDGE_CURVE ( 'NONE', #26129, #1852, #29808, .T. ) ;
#23784 = ORIENTED_EDGE ( 'NONE', *, *, #18081, .F. ) ;
#23783 = DIRECTION ( 'NONE',  ( 0.000000000000000000, 0.000000000000000000, -1.000000000000000000 ) ) ;
#23785 = VERTEX_POINT ( 'NONE', #4571 ) ;
#23786 = CARTESIAN_POINT ( 'NONE',  ( 69.32965659118902124, -6.955028994473984483, -4.522129901861164036 ) ) ;
#23787 = DIRECTION ( 'NONE',  ( -0.000000000000000000, -0.000000000000000000, -1.000000000000000000 ) ) ;
#23789 = ORIENTED_EDGE ( 'NONE', *, *, #9647, .T. ) ;
#23788 = DIRECTION ( 'NONE',  ( -1.000000000000000000, 0.000000000000000000, 0.000000000000000000 ) ) ;
#23790 = CARTESIAN_POINT ( 'NONE',  ( 14.71918161838887684, 9.125819088727514128, -1.050000000000000044 ) ) ;
#23791 = CARTESIAN_POINT ( 'NONE',  ( 6.353342831038617078, -18.33846711552379816, -1.748782834083794313 ) ) ;
#23792 = DIRECTION ( 'NONE',  ( 1.000000000000000000, 0.000000000000000000, 0.000000000000000000 ) ) ;
#23793 = CARTESIAN_POINT ( 'NONE',  ( 19.46384663048900876, -15.80031286559519010, -1.499999999999722444 ) ) ;
#23794 = CARTESIAN_POINT ( 'NONE',  ( 107.9809260575503629, -17.79470209034395012, -4.352197235538400655 ) ) ;
#23795 = DIRECTION ( 'NONE',  ( -0.000000000000000000, -0.000000000000000000, -1.000000000000000000 ) ) ;
#23796 = CARTESIAN_POINT ( 'NONE',  ( -57.14353245301024486, 0.5000000000000000000, -1.500000000000000000 ) ) ;
#23797 = CARTESIAN_POINT ( 'NONE',  ( 24.50111451137534146, -3.256483526998273983E-15, 2.499999999999998668 ) ) ;
#23798 = CARTESIAN_POINT ( 'NONE',  ( 29.24242457239596149, -6.576397578954725986, 3.993433898512776636 ) ) ;
#23799 = CARTESIAN_POINT ( 'NONE',  ( -3.889464452585704723, -3.181828567483031112, 1.500000000000000000 ) ) ;
#23800 = CARTESIAN_POINT ( 'NONE',  ( 0.000000000000000000, 0.000000000000000000, 7.482234843104714983 ) ) ;
#23801 = ORIENTED_EDGE ( 'NONE', *, *, #20488, .F. ) ;
#23802 = CARTESIAN_POINT ( 'NONE',  ( 6.356382228872879736, -3.475951004017282298, -7.873648075250535783 ) ) ;
#23803 = CARTESIAN_POINT ( 'NONE',  ( 107.3882468701019661, -16.47045351801639512, -2.697862662383026855 ) ) ;
#23804 = CARTESIAN_POINT ( 'NONE',  ( 2.976845687893344916, 9.149921655307451829, 0.5490754078162828344 ) ) ;
#23805 = ORIENTED_EDGE ( 'NONE', *, *, #31552, .T. ) ;
#23806 = CARTESIAN_POINT ( 'NONE',  ( 22.04750000136559507, -1.913930629741527500, 2.363507492473149618 ) ) ;
#23807 = EDGE_CURVE ( 'NONE', #30095, #24602, #1726, .T. ) ;
#23808 = CARTESIAN_POINT ( 'NONE',  ( 25.48003937004066444, -2.000525074609735832, -1.887699336444768505 ) ) ;
#23809 = CARTESIAN_POINT ( 'NONE',  ( 21.04494988260847776, -21.68420912488515739, 1.499840339240483766 ) ) ;
#23810 = ORIENTED_EDGE ( 'NONE', *, *, #31935, .T. ) ;
#23811 = CARTESIAN_POINT ( 'NONE',  ( 0.6737277144758835323, -5.221526237309871199, -1.499999999999999556 ) ) ;
#23812 =( NAMED_UNIT ( * ) SI_UNIT ( $, .STERADIAN. ) SOLID_ANGLE_UNIT ( ) );
#23813 = ORIENTED_EDGE ( 'NONE', *, *, #31797, .T. ) ;
#23814 = EDGE_CURVE ( 'NONE', #27203, #10039, #31606, .T. ) ;
#23815 = ORIENTED_EDGE ( 'NONE', *, *, #447, .T. ) ;
#23816 = LINE ( 'NONE', #23962, #13967 ) ;
#23817 = COORDINATED_UNIVERSAL_TIME_OFFSET ( 0, 0, .AHEAD. ) ;
#23819 = ORIENTED_EDGE ( 'NONE', *, *, #23617, .F. ) ;
#23818 = CARTESIAN_POINT ( 'NONE',  ( -4.575445569750785424, -7.851872718547149965, -0.9788672205760856615 ) ) ;
#23820 = ORIENTED_EDGE ( 'NONE', *, *, #9962, .T. ) ;
#23821 = CARTESIAN_POINT ( 'NONE',  ( -23.35000000000000142, -10.96966150227469505, 4.500000000000000888 ) ) ;
#23822 = ORIENTED_EDGE ( 'NONE', *, *, #3314, .T. ) ;
#23823 = DIRECTION ( 'NONE',  ( 0.000000000000000000, 0.03489949670250105246, -0.9993908270190957621 ) ) ;
#23825 = VERTEX_POINT ( 'NONE', #24789 ) ;
#23824 = CARTESIAN_POINT ( 'NONE',  ( 23.87320362638740789, -3.497993740947836994, -0.8105616805859642282 ) ) ;
#23826 = CARTESIAN_POINT ( 'NONE',  ( 0.000000000000000000, 0.000000000000000000, 0.000000000000000000 ) ) ;
#23827 = LINE ( 'NONE', #31369, #14367 ) ;
#23828 = CARTESIAN_POINT ( 'NONE',  ( -50.60000000000000142, -10.96966150227468972, 7.500000000000000000 ) ) ;
#23829 = DIRECTION ( 'NONE',  ( -1.000000000000000000, 0.000000000000000000, 0.000000000000000000 ) ) ;
#23830 = CARTESIAN_POINT ( 'NONE',  ( 107.5615483389071301, -18.98034905113282278, 4.530923109470624155 ) ) ;
#23831 = CARTESIAN_POINT ( 'NONE',  ( -53.98119003043982644, 5.049498764322128963, 2.713197721588770595 ) ) ;
#23832 = CARTESIAN_POINT ( 'NONE',  ( -23.35000000000000142, -10.96966150227469505, 4.500000000000000888 ) ) ;
#23833 = CARTESIAN_POINT ( 'NONE',  ( 18.61776180081012200, -7.449878658333833670, -1.169950778994415463 ) ) ;
#23834 = CARTESIAN_POINT ( 'NONE',  ( 10.57125986779756843, 0.8254815157535241310, 4.681538312723519724 ) ) ;
#23835 = CARTESIAN_POINT ( 'NONE',  ( -23.35000000000000142, -10.96966150227469505, -1.500000000000000000 ) ) ;
#23836 = DIRECTION ( 'NONE',  ( 2.219124775574934040E-17, 0.2588190451025216832, -0.9659258262890680902 ) ) ;
#23837 = CARTESIAN_POINT ( 'NONE',  ( 22.73500000273118715, -2.486304738420683780, 0.2613211581691335383 ) ) ;
#23838 = LINE ( 'NONE', #23207, #9707 ) ;
#23839 = B_SPLINE_CURVE_WITH_KNOTS ( 'NONE', 3,
 ( #14300, #19350, #16332, #1128, #5975, #26542, #19169, #1315 ),
 .UNSPECIFIED., .F., .F.,
 ( 4, 2, 2, 4 ),
 ( 2.024520226902067482E-07, 0.001261135997420257965, 0.001891602770119041712, 0.002522069542817825458 ),
 .UNSPECIFIED. ) ;
#23840 = EDGE_CURVE ( 'NONE', #22762, #3071, #30163, .T. ) ;
#23841 = CARTESIAN_POINT ( 'NONE',  ( 21.42249999999999943, -2.378061970571983430, 1.291182301015471490 ) ) ;
#23842 = CARTESIAN_POINT ( 'NONE',  ( -2.712550801365593234, -3.675193018007246071, 1.088641768524163167 ) ) ;
#23843 = ORIENTED_EDGE ( 'NONE', *, *, #25526, .F. ) ;
#23844 = CARTESIAN_POINT ( 'NONE',  ( -6.850050799999999995, 1.549418761218566143, -2.853674364686379583 ) ) ;
#23845 = ADVANCED_FACE ( 'NONE', ( #6882 ), #22279, .F. ) ;
#23846 = DIRECTION ( 'NONE',  ( 1.000000000000000000, -0.000000000000000000, -0.000000000000000000 ) ) ;
#23847 = EDGE_CURVE ( 'NONE', #21704, #8954, #25099, .T. ) ;
#23848 = CARTESIAN_POINT ( 'NONE',  ( 0.000000000000000000, 1.699438267350499521, -9.241976615262139205 ) ) ;
#23849 = CARTESIAN_POINT ( 'NONE',  ( 9.437548970008970528, 0.1642588933130853801, 1.000000000000000000 ) ) ;
#23850 = ORIENTED_EDGE ( 'NONE', *, *, #30625, .F. ) ;
#23851 = CARTESIAN_POINT ( 'NONE',  ( 68.95673039202250720, -3.844717801499071719, -2.184957270212465108 ) ) ;
#23852 = ORIENTED_EDGE ( 'NONE', *, *, #31884, .T. ) ;
#23853 = CARTESIAN_POINT ( 'NONE',  ( 1.138639876302608878, -9.033957850008556889, 1.500000000000000000 ) ) ;
#23854 = APPROVAL_STATUS ( 'not_yet_approved' ) ;
#23855 = ADVANCED_FACE ( 'NONE', ( #22623 ), #32832, .F. ) ;
#23856 = CARTESIAN_POINT ( 'NONE',  ( 85.01592635901123174, -4.880223576677269470, 4.275175582411163688 ) ) ;
#23857 = EDGE_CURVE ( 'NONE', #29226, #31221, #18232, .T. ) ;
#23858 = CARTESIAN_POINT ( 'NONE',  ( 6.883866482134013864, -8.452201317944586734, -2.190971798910030799 ) ) ;
#23859 = CARTESIAN_POINT ( 'NONE',  ( 22.16261821944717170, -17.22505787983993741, -1.541391846742717231 ) ) ;
#23860 = LINE ( 'NONE', #11491, #13427 ) ;
#23861 = ORIENTED_EDGE ( 'NONE', *, *, #13019, .T. ) ;
#23862 = CARTESIAN_POINT ( 'NONE',  ( 18.78902913792331475, -5.535453558220409853, 4.282233996325129688 ) ) ;
#23863 = DIRECTION ( 'NONE',  ( -1.000000000000000000, 8.574039729943022041E-17, 1.232595164407830946E-32 ) ) ;
#23864 = CARTESIAN_POINT ( 'NONE',  ( 22.11000000136559507, -2.892927487894331406, 1.570731468192932301 ) ) ;
#23865 = EDGE_CURVE ( 'NONE', #3159, #22549, #19211, .T. ) ;
#23867 = VERTEX_POINT ( 'NONE', #20766 ) ;
#23866 = DIRECTION ( 'NONE',  ( 0.000000000000000000, 0.000000000000000000, -1.000000000000000000 ) ) ;
#23868 = CARTESIAN_POINT ( 'NONE',  ( 0.000000000000000000, 0.000000000000000000, 0.000000000000000000 ) ) ;
#23869 = CARTESIAN_POINT ( 'NONE',  ( 108.1608272491863971, 19.07370950775312579, 3.877216635335003048 ) ) ;
#23870 = DIRECTION ( 'NONE',  ( 1.000000000000000000, 0.000000000000000000, 0.000000000000000000 ) ) ;
#23871 = ORIENTED_EDGE ( 'NONE', *, *, #14425, .F. ) ;
#23872 = ORIENTED_EDGE ( 'NONE', *, *, #30993, .F. ) ;
#23873 = CARTESIAN_POINT ( 'NONE',  ( 20.74999999999999645, -6.000000000000003553, 7.347880794884121708E-16 ) ) ;
#23874 = PLANE ( 'NONE',  #8089 ) ;
#23875 = CARTESIAN_POINT ( 'NONE',  ( 108.1641292914955130, -20.43278308392451947, -1.481931422884068761 ) ) ;
#23876 = CARTESIAN_POINT ( 'NONE',  ( 10.56870887191539587, 4.467071865485493731, -1.625881193364653088 ) ) ;
#23877 = CARTESIAN_POINT ( 'NONE',  ( 25.25168948427242199, -17.50930648703901582, 1.141351624973356849 ) ) ;
#23878 = CARTESIAN_POINT ( 'NONE',  ( 9.560873106162633529E-17, 1.115095498423374965, -4.884328206559825247 ) ) ;
#23879 = CARTESIAN_POINT ( 'NONE',  ( 0.000000000000000000, 0.000000000000000000, 0.000000000000000000 ) ) ;
#23880 = CARTESIAN_POINT ( 'NONE',  ( -3.437550801365593767, -1.088641768524163611, -3.675193018007245627 ) ) ;
#23881 = ADVANCED_FACE ( 'NONE', ( #7889 ), #15246, .T. ) ;
#23882 = CARTESIAN_POINT ( 'NONE',  ( 107.4500593345376558, -17.36019228850485163, -4.522129901861164925 ) ) ;
#23883 = CARTESIAN_POINT ( 'NONE',  ( 102.5153059484010640, -5.316817625849363793, 1.873789182723388791 ) ) ;
#23884 = ORIENTED_EDGE ( 'NONE', *, *, #19060, .F. ) ;
#23885 = CARTESIAN_POINT ( 'NONE',  ( 17.41559371906258136, 18.02474698348859405, 1.508259000770581615 ) ) ;
#23886 = ADVANCED_FACE ( 'NONE', ( #709 ), #28409, .T. ) ;
#23887 = ORIENTED_EDGE ( 'NONE', *, *, #11632, .T. ) ;
#23888 = COORDINATED_UNIVERSAL_TIME_OFFSET ( 0, 0, .AHEAD. ) ;
#23889 = CARTESIAN_POINT ( 'NONE',  ( 18.75846136547140830, -5.877139905506971296, 3.996604665398700629 ) ) ;
#23890 = EDGE_CURVE ( 'NONE', #14922, #31656, #28123, .T. ) ;
#23891 = DIRECTION ( 'NONE',  ( 0.000000000000000000, 0.000000000000000000, -1.000000000000000000 ) ) ;
#23892 = ORIENTED_EDGE ( 'NONE', *, *, #25048, .F. ) ;
#23893 = DIRECTION ( 'NONE',  ( -0.000000000000000000, -1.000000000000000000, -0.000000000000000000 ) ) ;
#23894 = ORIENTED_EDGE ( 'NONE', *, *, #10917, .F. ) ;
#23895 = VERTEX_POINT ( 'NONE', #31148 ) ;
#23896 = CARTESIAN_POINT ( 'NONE',  ( -1.033057378353439804, -8.048844657541355474, -4.522129901861164925 ) ) ;
#23897 = CARTESIAN_POINT ( 'NONE',  ( -5.012550801365594388, -3.368539882008727115, -1.828967928396027842 ) ) ;
#23898 = CARTESIAN_POINT ( 'NONE',  ( 25.98499999999999943, 2.486304738420679783, -0.2613211581691337604 ) ) ;
#23899 = EDGE_CURVE ( 'NONE', #11936, #9106, #5993, .T. ) ;
#23900 = CARTESIAN_POINT ( 'NONE',  ( 0.000000000000000000, 0.000000000000000000, 0.000000000000000000 ) ) ;
#23902 = ORIENTED_EDGE ( 'NONE', *, *, #26197, .T. ) ;
#23901 = CARTESIAN_POINT ( 'NONE',  ( 11.15636752060594716, 3.970267605981960379, -1.500000000000000222 ) ) ;
#23903 = CARTESIAN_POINT ( 'NONE',  ( -6.287550801365593856, 2.228590825266444142, 2.752080473201636845 ) ) ;
#23904 = CARTESIAN_POINT ( 'NONE',  ( 12.93395381280125278, 7.012641540630032644, 1.500000000000000000 ) ) ;
#23905 = DIRECTION ( 'NONE',  ( 0.000000000000000000, 0.000000000000000000, 1.000000000000000000 ) ) ;
#23906 = CARTESIAN_POINT ( 'NONE',  ( 21.73500000136559507, 1.570731468192929858, 2.892927487894329186 ) ) ;
#23908 = ORIENTED_EDGE ( 'NONE', *, *, #28299, .F. ) ;
#23907 = DIRECTION ( 'NONE',  ( -0.6916610887771522664, 0.000000000000000000, -0.7222222222222217658 ) ) ;
#23909 = B_SPLINE_CURVE_WITH_KNOTS ( 'NONE', 3,
 ( #32004, #2079, #14112, #10427 ),
 .UNSPECIFIED., .F., .F.,
 ( 4, 4 ),
 ( 0.000000000000000000, 0.003022500951957912251 ),
 .UNSPECIFIED. ) ;
#23910 = CARTESIAN_POINT ( 'NONE',  ( -30.17898719005535213, 11.44152090502456787, 1.947135075133271220 ) ) ;
#23911 = CARTESIAN_POINT ( 'NONE',  ( 21.23500000273118715, 2.486304738420679783, -0.2613211581691337604 ) ) ;
#23912 = CARTESIAN_POINT ( 'NONE',  ( -23.54713438637982748, 3.520075575296777171, 1.500000000000000000 ) ) ;
#23913 = CARTESIAN_POINT ( 'NONE',  ( 3.499999999999999556, 0.000000000000000000, 0.000000000000000000 ) ) ;
#23914 = CARTESIAN_POINT ( 'NONE',  ( 8.870145747188287189, 0.5000000000000001110, 0.000000000000000000 ) ) ;
#23915 = CARTESIAN_POINT ( 'NONE',  ( 0.7632845268398871230, -5.538577986808947529, 6.772677083992368452 ) ) ;
#23916 = EDGE_CURVE ( 'NONE', #17640, #26134, #30014, .T. ) ;
#23917 = LINE ( 'NONE', #6053, #18310 ) ;
#23918 = CARTESIAN_POINT ( 'NONE',  ( -5.837550801365594566, -1.088641768524163389, -3.675193018007246071 ) ) ;
#23919 = ORIENTED_EDGE ( 'NONE', *, *, #18586, .F. ) ;
#23920 =( BOUNDED_SURFACE ( )  B_SPLINE_SURFACE ( 3, 2, ( 
 ( #19546, #32081, #6490 ),
 ( #4010, #14178, #24377 ),
 ( #29743, #1493, #11669 ),
 ( #9152, #24884, #29238 ) ),
 .UNSPECIFIED., .F., .F., .F. ) 
 B_SPLINE_SURFACE_WITH_KNOTS ( ( 4, 4 ),
 ( 3, 3 ),
 ( 0.000000000000000000, 0.003454001599076453322 ),
 ( 0.000000000000000000, 1.000000000000000000 ),
 .UNSPECIFIED. ) 
 GEOMETRIC_REPRESENTATION_ITEM ( )  RATIONAL_B_SPLINE_SURFACE ( (
 ( 1.000000000000000000, 0.7097644798780626818, 1.000000000000000000),
 ( 1.000000000000000000, 0.7097691176663378787, 1.000000000000000000),
 ( 1.000000000000000000, 0.7097737773069716649, 1.000000000000000000),
 ( 1.000000000000000000, 0.7097784590644244940, 1.000000000000000000) ) ) 
 REPRESENTATION_ITEM ( '' )  SURFACE ( )  );
#23921 = CARTESIAN_POINT ( 'NONE',  ( 18.74274612900821779, -21.25842652921702935, 1.734019191250946168 ) ) ;
#23922 = CARTESIAN_POINT ( 'NONE',  ( 7.249760686538667009, -6.940565734314570356, -4.007137495034885255 ) ) ;
#23924 = LINE ( 'NONE', #8544, #8058 ) ;
#23923 = CARTESIAN_POINT ( 'NONE',  ( 108.1033628964161295, 18.75372531717770386, -4.515627636720681792 ) ) ;
#23925 = ORIENTED_EDGE ( 'NONE', *, *, #22420, .F. ) ;
#23926 = CARTESIAN_POINT ( 'NONE',  ( -4.512942406915326998, 4.884725290497410777E-15, -2.999999999999999556 ) ) ;
#23927 = ORIENTED_EDGE ( 'NONE', *, *, #21077, .T. ) ;
#23928 = DIRECTION ( 'NONE',  ( 1.000000000000000000, 0.000000000000000000, 0.000000000000000000 ) ) ;
#23930 = ORIENTED_EDGE ( 'NONE', *, *, #25311, .T. ) ;
#23929 = CARTESIAN_POINT ( 'NONE',  ( -1.394036994807583480E-16, -1.625881193364668409, -4.467071865485488402 ) ) ;
#23931 = VERTEX_POINT ( 'NONE', #379 ) ;
#23932 = CYLINDRICAL_SURFACE ( 'NONE', #31619, 11.00000000000000000 ) ;
#23933 = EDGE_CURVE ( 'NONE', #14830, #4619, #18802, .T. ) ;
#23934 = CARTESIAN_POINT ( 'NONE',  ( 0.000000000000000000, -2.861184399890954300, -6.440778198864141935 ) ) ;
#23935 = CC_DESIGN_PERSON_AND_ORGANIZATION_ASSIGNMENT ( #354, #10530, ( #6052 ) ) ;
#23937 = ORIENTED_EDGE ( 'NONE', *, *, #20205, .T. ) ;
#23936 = CARTESIAN_POINT ( 'NONE',  ( 18.91097450938967484, -4.172349046794661120, 3.084778196783016568 ) ) ;
#23938 = CARTESIAN_POINT ( 'NONE',  ( 9.302055952181039089, 0.2457637073014076745, -1.050000000000000044 ) ) ;
#23939 = CARTESIAN_POINT ( 'NONE',  ( 10.00000000000000178, -8.574039729943018837E-16, 0.000000000000000000 ) ) ;
#23940 = CARTESIAN_POINT ( 'NONE',  ( 108.0410785058465279, -18.66088238176251224, -3.974415582670320912 ) ) ;
#23941 = CARTESIAN_POINT ( 'NONE',  ( 8.486535498532354893, -10.66169397763258253, -1.499999999999820366 ) ) ;
#23942 = CARTESIAN_POINT ( 'NONE',  ( 107.9486069274682336, -17.32931465714983688, -4.530749433310830909 ) ) ;
#23943 = CARTESIAN_POINT ( 'NONE',  ( 0.000000000000000000, 6.100541242131516384, 3.528937025535512362 ) ) ;
#23944 = CARTESIAN_POINT ( 'NONE',  ( 24.67250000273118715, -2.378061970571983430, 1.291182301015471490 ) ) ;
#23945 = CARTESIAN_POINT ( 'NONE',  ( 85.03618457008606413, -5.204454441937159892, 3.993433531046222118 ) ) ;
#23946 = EDGE_CURVE ( 'NONE', #24299, #2424, #2568, .T. ) ;
#23947 = CARTESIAN_POINT ( 'NONE',  ( 3.554613218822866294, -15.76807188677689631, 4.522129901861158707 ) ) ;
#23948 = CARTESIAN_POINT ( 'NONE',  ( 3.086618293031886395, -0.003885106576433895991, 0.6225218429476599979 ) ) ;
#23949 = ORIENTED_EDGE ( 'NONE', *, *, #26545, .F. ) ;
#23950 = DIRECTION ( 'NONE',  ( -1.000000000000000000, -0.000000000000000000, -0.000000000000000000 ) ) ;
#23951 = EDGE_CURVE ( 'NONE', #14212, #32393, #17201, .T. ) ;
#23952 = DIRECTION ( 'NONE',  ( -1.000000000000000000, -0.000000000000000000, -0.000000000000000000 ) ) ;
#23953 = DIRECTION ( 'NONE',  ( -0.04710975479914572550, -0.5265925107009689077, 0.8488115212910427587 ) ) ;
#23954 = ORIENTED_EDGE ( 'NONE', *, *, #19634, .F. ) ;
#23955 = CARTESIAN_POINT ( 'NONE',  ( -41.86373177837819526, -16.13513036599590222, 5.128141679950119602 ) ) ;
#23956 = CARTESIAN_POINT ( 'NONE',  ( 20.71913853892345614, -21.61372392228095407, 1.559032431776717020 ) ) ;
#23957 = ORIENTED_EDGE ( 'NONE', *, *, #12858, .T. ) ;
#23958 = DIRECTION ( 'NONE',  ( 8.541412920197221047E-17, 0.9961946980917458783, -0.08715574274765462703 ) ) ;
#23959 = CARTESIAN_POINT ( 'NONE',  ( 7.240458295750347162, -14.59873704243364756, 1.084202172485504434E-15 ) ) ;
#23960 = ORIENTED_EDGE ( 'NONE', *, *, #32831, .F. ) ;
#23961 = ORIENTED_EDGE ( 'NONE', *, *, #15680, .F. ) ;
#23962 = CARTESIAN_POINT ( 'NONE',  ( 2.619932554246560023E-16, 3.055657119358801133, 3.641590349731939735 ) ) ;
#23963 = SECURITY_CLASSIFICATION_LEVEL ( 'unclassified' ) ;
#23965 = ORIENTED_EDGE ( 'NONE', *, *, #17760, .T. ) ;
#23964 = PLANE ( 'NONE',  #11182 ) ;
#23966 = EDGE_LOOP ( 'NONE', ( #21520, #11954, #3738 ) ) ;
#23967 = LINE ( 'NONE', #31852, #22493 ) ;
#23968 = ORIENTED_EDGE ( 'NONE', *, *, #10018, .T. ) ;
#23969 = CARTESIAN_POINT ( 'NONE',  ( 23.22564588060107482, -21.93932300456764040, 1.000000000000000000 ) ) ;
#23970 = PLANE ( 'NONE',  #11777 ) ;
#23972 = VERTEX_POINT ( 'NONE', #26275 ) ;
#23971 = DIRECTION ( 'NONE',  ( -1.000000000000000000, 0.000000000000000000, 0.000000000000000000 ) ) ;
#23973 = CARTESIAN_POINT ( 'NONE',  ( 21.92250000273118715, -1.291182301015472600, -2.378061970571982098 ) ) ;
#23974 = CARTESIAN_POINT ( 'NONE',  ( 26.08945412691624099, 19.05746434167065928, -1.050000000000000044 ) ) ;
#23975 = DIRECTION ( 'NONE',  ( 1.000000000000000000, 1.387778780781445833E-14, 4.846230290920773249E-16 ) ) ;
#23976 = CARTESIAN_POINT ( 'NONE',  ( 101.6022419886208610, -1.170867242066747860, -0.07017451552781628354 ) ) ;
#23977 = CARTESIAN_POINT ( 'NONE',  ( 108.0608891800116709, -18.94615116146357536, 4.531103216122085442 ) ) ;
#23978 = VECTOR ( 'NONE', #7808, 1000.000000000000000 ) ;
#23979 = CARTESIAN_POINT ( 'NONE',  ( 72.52374898135332160, -19.78015497550546442, -4.522129901861164925 ) ) ;
#23980 = DIRECTION ( 'NONE',  ( -1.000000000000000000, 0.000000000000000000, 0.000000000000000000 ) ) ;
#23981 = EDGE_CURVE ( 'NONE', #17584, #27584, #11313, .T. ) ;
#23982 = ADVANCED_FACE ( 'NONE', ( #29114 ), #6660, .T. ) ;
#23983 = CARTESIAN_POINT ( 'NONE',  ( 5.612974259723585213, 7.650268724902057116, 2.996912441296202267 ) ) ;
#23984 = CARTESIAN_POINT ( 'NONE',  ( -34.49361350329746756, 0.1741578047003206897, -2.493613503297456013 ) ) ;
#23985 = DIRECTION ( 'NONE',  ( 3.471561733563245301E-15, 0.000000000000000000, -1.000000000000000000 ) ) ;
#23986 = CARTESIAN_POINT ( 'NONE',  ( 21.75111450864415730, -1.283275288181523244E-15, -2.499999999999998668 ) ) ;
#23987 = CARTESIAN_POINT ( 'NONE',  ( -2.662550801365593411, -3.521866450007987037, -0.3701630799359323931 ) ) ;
#23988 = ORIENTED_EDGE ( 'NONE', *, *, #15570, .F. ) ;
#23989 = CARTESIAN_POINT ( 'NONE',  ( -8.000050800000000351, -2.331437884370912705, 1.887961173149512062 ) ) ;
#23990 = CIRCLE ( 'NONE', #28275, 0.4500000000000001776 ) ;
#23991 = AXIS2_PLACEMENT_3D ( 'NONE', #22967, #22670, #5108 ) ;
#23992 = CARTESIAN_POINT ( 'NONE',  ( 10.47272779071480819, 17.64623289522323191, -5.396302277755719246 ) ) ;
#23993 = CARTESIAN_POINT ( 'NONE',  ( -5.200050800000000528, 2.331437884370912705, -1.887961173149511618 ) ) ;
#23994 = CARTESIAN_POINT ( 'NONE',  ( 7.158832484464911161, -3.801775501249473610, 1.500000000000000000 ) ) ;
#23995 = ORIENTED_EDGE ( 'NONE', *, *, #11682, .F. ) ;
#23996 = CARTESIAN_POINT ( 'NONE',  ( 7.429379966294620274, -10.00822258298124190, -1.499999999999999778 ) ) ;
#23997 = VECTOR ( 'NONE', #6120, 1000.000000000000000 ) ;
#23998 = ORIENTED_EDGE ( 'NONE', *, *, #24403, .T. ) ;
#23999 = CARTESIAN_POINT ( 'NONE',  ( 0.4715469964658544066, -8.230657990693778459, 1.499999999999999556 ) ) ;
#24000 = APPROVAL_DATE_TIME ( #3640, #13290 ) ;
#24001 = CARTESIAN_POINT ( 'NONE',  ( 40.87842237877963925, -5.874508746777070023, 4.155404504730444870 ) ) ;
#24002 = EDGE_CURVE ( 'NONE', #1418, #4740, #16237, .T. ) ;
#24003 = DIRECTION ( 'NONE',  ( 0.000000000000000000, 0.000000000000000000, 1.000000000000000000 ) ) ;
#24004 = DIRECTION ( 'NONE',  ( 0.000000000000000000, 1.000000000000000000, 0.000000000000000000 ) ) ;
#24005 = CARTESIAN_POINT ( 'NONE',  ( 15.28872660057388799, 20.76088595412472060, 4.629213727441584325 ) ) ;
#24006 = ORIENTED_EDGE ( 'NONE', *, *, #24585, .T. ) ;
#24007 = CARTESIAN_POINT ( 'NONE',  ( 18.75828436641558028, -5.879118399717575549, 3.993434336035622589 ) ) ;
#24008 = LINE ( 'NONE', #13804, #30523 ) ;
#24009 = CARTESIAN_POINT ( 'NONE',  ( 0.000000000000000000, -5.522688772756352726, -6.461416928141300531 ) ) ;
#24010 = AXIS2_PLACEMENT_3D ( 'NONE', #24012, #11817, #19527 ) ;
#24011 = ADVANCED_FACE ( 'NONE', ( #18733 ), #13960, .F. ) ;
#24013 = ORIENTED_EDGE ( 'NONE', *, *, #10601, .F. ) ;
#24012 = CARTESIAN_POINT ( 'NONE',  ( -12.44989959798873791, 0.000000000000000000, -12.99999999999999645 ) ) ;
#24014 = CARTESIAN_POINT ( 'NONE',  ( -3.812550801365593323, 3.368539882008727115, 1.828967928396026954 ) ) ;
#24015 = AXIS2_PLACEMENT_3D ( 'NONE', #8733, #20784, #16070 ) ;
#24016 = CARTESIAN_POINT ( 'NONE',  ( 18.62684137740528811, -7.348387214320800886, 1.526432259289672855 ) ) ;
#24017 = DIRECTION ( 'NONE',  ( 0.000000000000000000, 0.000000000000000000, 1.000000000000000000 ) ) ;
#24018 = VECTOR ( 'NONE', #27799, 1000.000000000000000 ) ;
#24019 = CARTESIAN_POINT ( 'NONE',  ( 7.249760686538667009, -2.741043480754877582, -7.530955069117540646 ) ) ;
#24020 = CARTESIAN_POINT ( 'NONE',  ( 1.750000000000000222, 8.265874651078018331, 1.981241088980808751 ) ) ;
#24021 = PLANE ( 'NONE',  #15133 ) ;
#24022 = FACE_OUTER_BOUND ( 'NONE', #27213, .T. ) ;
#24023 = ADVANCED_FACE ( 'NONE', ( #16998 ), #4499, .F. ) ;
#24024 = CARTESIAN_POINT ( 'NONE',  ( -50.60000000000000142, -10.96966150227468972, 6.999999999999999112 ) ) ;
#24025 = ORIENTED_EDGE ( 'NONE', *, *, #20671, .F. ) ;
#24026 = DIRECTION ( 'NONE',  ( 0.000000000000000000, 0.9961946980917451011, 0.08715574274766293983 ) ) ;
#24027 = CARTESIAN_POINT ( 'NONE',  ( -59.75626822162179508, -5.804869634004071521, 5.128141679950119602 ) ) ;
#24028 = EDGE_CURVE ( 'NONE', #15458, #29777, #5456, .T. ) ;
#24029 = CARTESIAN_POINT ( 'NONE',  ( -3.787550801365593411, -0.3701630799359326152, 3.521866450007987037 ) ) ;
#24030 = AXIS2_PLACEMENT_3D ( 'NONE', #4130, #16980, #20026 ) ;
#24031 = DIRECTION ( 'NONE',  ( -0.000000000000000000, -0.000000000000000000, -1.000000000000000000 ) ) ;
#24032 = CARTESIAN_POINT ( 'NONE',  ( 23.62691144361181372, -7.794821506209283157, 1.529339877365281763 ) ) ;
#24033 = ORIENTED_EDGE ( 'NONE', *, *, #3666, .F. ) ;
#24034 = CARTESIAN_POINT ( 'NONE',  ( 3.249999999999999556, 4.472189673936786569, 8.264486777890123648 ) ) ;
#24035 = CIRCLE ( 'NONE', #30490, 11.00000000000000000 ) ;
#24036 = AXIS2_PLACEMENT_3D ( 'NONE', #5416, #7410, #28148 ) ;
#24037 = ORIENTED_EDGE ( 'NONE', *, *, #25551, .F. ) ;
#24038 = APPROVAL_DATE_TIME ( #28910, #26006 ) ;
#24039 = EDGE_CURVE ( 'NONE', #32678, #30689, #13554, .T. ) ;
#24040 = CARTESIAN_POINT ( 'NONE',  ( 54.97719073509556864, -6.505350304057381017, 3.995336669067921953 ) ) ;
#24041 = VECTOR ( 'NONE', #20339, 1000.000000000000000 ) ;
#24042 = AXIS2_PLACEMENT_3D ( 'NONE', #16748, #29632, #32321 ) ;
#24043 = CARTESIAN_POINT ( 'NONE',  ( -8.000050800000000351, 0.000000000000000000, 0.000000000000000000 ) ) ;
#24044 = VERTEX_POINT ( 'NONE', #27199 ) ;
#24045 = CARTESIAN_POINT ( 'NONE',  ( 0.08034252266852373592, -10.71005054582363414, 1.301095883299237643 ) ) ;
#24046 = ADVANCED_FACE ( 'NONE', ( #6970 ), #1640, .F. ) ;
#24047 = ORIENTED_EDGE ( 'NONE', *, *, #5403, .F. ) ;
#24048 = ORIENTED_EDGE ( 'NONE', *, *, #1021, .F. ) ;
#24049 = FACE_OUTER_BOUND ( 'NONE', #4086, .T. ) ;
#24050 = CARTESIAN_POINT ( 'NONE',  ( -5.062550801365593323, -3.521866450007987037, -0.3701630799359323931 ) ) ;
#24051 = CARTESIAN_POINT ( 'NONE',  ( 22.42250000000000298, -2.378061970571983430, 1.291182301015471712 ) ) ;
#24052 = CARTESIAN_POINT ( 'NONE',  ( 0.1142986632944693048, -6.518936808292961516, -1.773886185393975135 ) ) ;
#24054 = EDGE_LOOP ( 'NONE', ( #1393, #21563, #15857, #26165 ) ) ;
#24053 = CARTESIAN_POINT ( 'NONE',  ( 3.249999999999999556, -6.478011392632939902, 6.807171995660557862 ) ) ;
#24055 = CARTESIAN_POINT ( 'NONE',  ( -7.987550801365593145, 3.521866450007987037, 0.3701630799359328372 ) ) ;
#24056 = CARTESIAN_POINT ( 'NONE',  ( 16.54275606342307725, 11.79585867019468992, 1.500000000000000000 ) ) ;
#24057 = AXIS2_PLACEMENT_3D ( 'NONE', #2165, #12836, #30607 ) ;
#24058 = DIRECTION ( 'NONE',  ( 1.000000000000000000, 0.000000000000000000, 0.000000000000000000 ) ) ;
#24060 = EDGE_CURVE ( 'NONE', #31165, #9839, #14487, .T. ) ;
#24059 = CARTESIAN_POINT ( 'NONE',  ( 21.98500000136559507, -2.892927487894331406, 1.570731468192932301 ) ) ;
#24061 = AXIS2_PLACEMENT_3D ( 'NONE', #15955, #13447, #23489 ) ;
#24063 = VERTEX_POINT ( 'NONE', #17174 ) ;
#24062 = CARTESIAN_POINT ( 'NONE',  ( 2.589202905186827053, -4.126870756446547439, 9.453729690310151312 ) ) ;
#24064 = EDGE_CURVE ( 'NONE', #3757, #2205, #19643, .T. ) ;
#24065 = AXIS2_PLACEMENT_3D ( 'NONE', #25140, #2440, #15280 ) ;
#24066 = AXIS2_PLACEMENT_3D ( 'NONE', #4480, #7807, #788 ) ;
#24067 = CARTESIAN_POINT ( 'NONE',  ( 22.67250000273118715, -2.378061970571983430, 1.291182301015471712 ) ) ;
#24068 = CARTESIAN_POINT ( 'NONE',  ( 0.000000000000000000, 18.00000000000000355, 0.000000000000000000 ) ) ;
#24069 = CARTESIAN_POINT ( 'NONE',  ( 0.000000000000000000, 10.90201369670498366, 1.464956435139577851 ) ) ;
#24070 = CARTESIAN_POINT ( 'NONE',  ( -4.499068592350032425, -5.402544097203555218, -1.500000000000000444 ) ) ;
#24071 = AXIS2_PLACEMENT_3D ( 'NONE', #10032, #7215, #20095 ) ;
#24072 = CARTESIAN_POINT ( 'NONE',  ( 0.3045633657615061107, -6.808202580038380525, -7.698316278340186614 ) ) ;
#24073 = CARTESIAN_POINT ( 'NONE',  ( -5.749676575031998027, 0.000000000000000000, -6.923700951379999857 ) ) ;
#24074 = CARTESIAN_POINT ( 'NONE',  ( -2.987550801365593145, -0.3701630799359326152, 3.521866450007987037 ) ) ;
#24075 = EDGE_LOOP ( 'NONE', ( #20046, #25824 ) ) ;
#24076 = ADVANCED_FACE ( 'NONE', ( #25695 ), #22857, .T. ) ;
#24077 = CARTESIAN_POINT ( 'NONE',  ( 20.55936702064834165, -21.63501724500275714, 1.474765012620294025 ) ) ;
#24078 = VECTOR ( 'NONE', #21503, 1000.000000000000000 ) ;
#24079 = DIRECTION ( 'NONE',  ( 0.000000000000000000, 0.7071067811865460184, 0.7071067811865490160 ) ) ;
#24081 = CARTESIAN_POINT ( 'NONE',  ( 10.56870887191539587, -1.625881193364728805, 4.467071865485467086 ) ) ;
#24080 = CARTESIAN_POINT ( 'NONE',  ( -15.02135460118491217, 0.000000000000000000, 1.095404497688272638 ) ) ;
#24082 = EDGE_LOOP ( 'NONE', ( #2237, #19853, #1652, #16436 ) ) ;
#24083 = TOROIDAL_SURFACE ( 'NONE', #18230, 300.0401151713995773, 1.800000000000017142 ) ;
#24084 = AXIS2_PLACEMENT_3D ( 'NONE', #11428, #8898, #21624 ) ;
#24085 = B_SPLINE_CURVE_WITH_KNOTS ( 'NONE', 3,
 ( #6926, #19654, #24648, #12121, #9093, #6617, #14785, #29691 ),
 .UNSPECIFIED., .F., .F.,
 ( 4, 2, 2, 4 ),
 ( 9.034501660022746213E-05, 0.009114482626497340256, 0.01362655143144589527, 0.01813862023639444682 ),
 .UNSPECIFIED. ) ;
#24086 = DIRECTION ( 'NONE',  ( 0.000000000000000000, 0.000000000000000000, 1.000000000000000000 ) ) ;
#24087 = AXIS2_PLACEMENT_3D ( 'NONE', #24430, #28795, #31822 ) ;
#24088 = ORIENTED_EDGE ( 'NONE', *, *, #18842, .F. ) ;
#24089 = CARTESIAN_POINT ( 'NONE',  ( 107.5617723795404999, -18.98359893170737323, 4.522129901861158707 ) ) ;
#24091 = VERTEX_POINT ( 'NONE', #12800 ) ;
#24090 = CARTESIAN_POINT ( 'NONE',  ( 69.01337413186240610, -4.973203518777342680, -3.998506773567884753 ) ) ;
#24092 = ORIENTED_EDGE ( 'NONE', *, *, #10950, .T. ) ;
#24093 = CARTESIAN_POINT ( 'NONE',  ( -8.000050800000018114, 1.979734913925816908, -2.936190332390367086 ) ) ;
#24094 = VECTOR ( 'NONE', #30339, 1000.000000000000000 ) ;
#24095 = EDGE_CURVE ( 'NONE', #20953, #25225, #23015, .T. ) ;
#24096 = CIRCLE ( 'NONE', #4361, 5.009999999999999787 ) ;
#24098 = CIRCLE ( 'NONE', #15571, 5.010000000000000675 ) ;
#24097 = CARTESIAN_POINT ( 'NONE',  ( 0.000000000000000000, 0.000000000000000000, 0.000000000000000000 ) ) ;
#24100 = ORIENTED_EDGE ( 'NONE', *, *, #18186, .F. ) ;
#24099 = CARTESIAN_POINT ( 'NONE',  ( 18.89416411554475062, -4.360255511983738508, 3.387663576533886278 ) ) ;
#24101 = CARTESIAN_POINT ( 'NONE',  ( 10.52016698309699372, 2.080188552104354383, -1.499999999999170441 ) ) ;
#24102 = DIRECTION ( 'NONE',  ( -0.03487826274237469659, -0.9987827659587182882, -0.03487826274237469659 ) ) ;
#24103 = CARTESIAN_POINT ( 'NONE',  ( 2.274274201627370040, 7.958834565715812381, -7.593217523255793466 ) ) ;
#24104 = ADVANCED_FACE ( 'NONE', ( #30568 ), #135, .F. ) ;
#24105 = CARTESIAN_POINT ( 'NONE',  ( 6.666829201526672577, -7.372062170296981520, -1.500000000000000000 ) ) ;
#24106 = CARTESIAN_POINT ( 'NONE',  ( 107.9587511384790872, -17.47538877214310915, -3.690911647522888916 ) ) ;
#24107 = EDGE_CURVE ( 'NONE', #2628, #7539, #21487, .T. ) ;
#24108 = CARTESIAN_POINT ( 'NONE',  ( 3.499999999999999556, -5.979767908488830663, -1.814490771706242622 ) ) ;
#24109 = AXIS2_PLACEMENT_3D ( 'NONE', #6202, #1024, #31623 ) ;
#24110 = LINE ( 'NONE', #29296, #18781 ) ;
#24111 = CARTESIAN_POINT ( 'NONE',  ( 5.377543748152549874, -7.892520144992443143, 1.391664247347202288 ) ) ;
#24112 = CIRCLE ( 'NONE', #32134, 6.248999999999998778 ) ;
#24113 = AXIS2_PLACEMENT_3D ( 'NONE', #12158, #31306, #3389 ) ;
#24114 = CARTESIAN_POINT ( 'NONE',  ( -0.5616989984783457013, -12.44624546261724163, 4.522129901861158707 ) ) ;
#24115 = CARTESIAN_POINT ( 'NONE',  ( 0.000000000000000000, 0.000000000000000000, 0.000000000000000000 ) ) ;
#24116 =( BOUNDED_CURVE ( )  B_SPLINE_CURVE ( 2, ( #27247, #30434, #1689, #12369, #22587, #4365, #32801, #14544, #1876 ),
 .UNSPECIFIED., .F., .F. ) 
 B_SPLINE_CURVE_WITH_KNOTS ( ( 3, 2, 2, 2, 3 ),
 ( 0.2000000000000001776, 0.2250000000000001166, 0.2500000000000000555, 0.2750000000000000777, 0.2966116191895003529 ),
 .UNSPECIFIED. ) 
 CURVE ( )  GEOMETRIC_REPRESENTATION_ITEM ( )  RATIONAL_B_SPLINE_CURVE ( ( 0.9999999999999994449, 0.9238795325112872936, 1.000000000000000000, 0.9238795325112867385, 1.000000000000000000, 0.9238795325112867385, 1.000000000000000000, 0.9341965377642874602, 0.9821626249036858880 ) ) 
 REPRESENTATION_ITEM ( '' )  );
#24117 = VERTEX_POINT ( 'NONE', #9640 ) ;
#24118 = LINE ( 'NONE', #16587, #20971 ) ;
#24119 = AXIS2_PLACEMENT_3D ( 'NONE', #23756, #11537, #23905 ) ;
#24120 = CIRCLE ( 'NONE', #28414, 4.999999999999999112 ) ;
#24121 = CARTESIAN_POINT ( 'NONE',  ( 8.870145747188287189, 0.000000000000000000, -1.000000000000000000 ) ) ;
#24122 = PLANE ( 'NONE',  #18863 ) ;
#24123 = ORIENTED_EDGE ( 'NONE', *, *, #23710, .F. ) ;
#24124 = VECTOR ( 'NONE', #16255, 1000.000000000000000 ) ;
#24125 = EDGE_CURVE ( 'NONE', #17057, #27222, #4408, .T. ) ;
#24126 = AXIS2_PLACEMENT_3D ( 'NONE', #13732, #18599, #10742 ) ;
#24127 = CC_DESIGN_PERSON_AND_ORGANIZATION_ASSIGNMENT ( #29905, #32586, ( #12431 ) ) ;
#24128 = CARTESIAN_POINT ( 'NONE',  ( -2.207304909706596874, -1.062355717592093463, -3.000000000000000888 ) ) ;
#24129 = CARTESIAN_POINT ( 'NONE',  ( 21.02910828058320902, -21.78322936331055359, -1.363801422436344613 ) ) ;
#24130 = VERTEX_POINT ( 'NONE', #30749 ) ;
#24131 = CARTESIAN_POINT ( 'NONE',  ( 8.520101525921534247, -14.04815114857715841, -1.500000000000000222 ) ) ;
#24132 = ORIENTED_EDGE ( 'NONE', *, *, #27562, .T. ) ;
#24133 = VECTOR ( 'NONE', #20042, 1000.000000000000000 ) ;
#24134 = EDGE_LOOP ( 'NONE', ( #13613, #27304, #15491, #4992 ) ) ;
#24135 = CARTESIAN_POINT ( 'NONE',  ( 25.20116447083585953, -17.53130488828775313, -1.247823832777839703 ) ) ;
#24136 = B_SPLINE_SURFACE_WITH_KNOTS ( 'NONE', 1, 3, ( 
 ( #24359, #1978, #4490, #4301, #14479, #32061, #24691, #3995 ),
 ( #19179, #1631, #4142, #1325, #12001, #17348, #1475, #11820 ) ),
 .UNSPECIFIED., .F., .F., .F.,
 ( 2, 2 ),
 ( 4, 2, 2, 4 ),
 ( 0.000000000000000000, 1.000000000000000000 ),
 ( 0.000000000000000000, 0.5000000000000000000, 0.7500000000000000000, 1.000000000000000000 ),
 .UNSPECIFIED. ) ;
#24137 = CALENDAR_DATE ( 2026, 6, 10 ) ;
#24139 = EDGE_LOOP ( 'NONE', ( #28641, #21102, #31545, #17911, #17680, #3585, #1700, #16714, #20762, #27751, #6365, #11437, #31326, #15418, #5092, #26503 ) ) ;
#24138 = DIRECTION ( 'NONE',  ( -0.03488359650710499277, 0.9989355049964836475, 0.03018263660036203666 ) ) ;
#24140 = EDGE_LOOP ( 'NONE', ( #26428, #31246, #14442, #28270, #6909 ) ) ;
#24141 = CARTESIAN_POINT ( 'NONE',  ( 24.92250000136559507, -1.913930629741527500, 2.363507492473149618 ) ) ;
#24142 = ADVANCED_FACE ( 'NONE', ( #27550 ), #4646, .F. ) ;
#24143 = CIRCLE ( 'NONE', #9732, 4.000000000000002665 ) ;
#24144 = CIRCLE ( 'NONE', #15075, 1.676012832569465205 ) ;
#24145 = ORIENTED_EDGE ( 'NONE', *, *, #1799, .T. ) ;
#24146 = CARTESIAN_POINT ( 'NONE',  ( 13.65718777918027271, -19.09288791508984673, 4.522129901861158707 ) ) ;
#24147 = CARTESIAN_POINT ( 'NONE',  ( 5.377543748152550762, -7.530955069117533540, 2.741043480754901118 ) ) ;
#24149 = ORIENTED_EDGE ( 'NONE', *, *, #23585, .F. ) ;
#24148 = CARTESIAN_POINT ( 'NONE',  ( 35.34214449212152687, -3.792788106923345559, -0.4367666027766938242 ) ) ;
#24150 = VECTOR ( 'NONE', #9820, 999.9999999999998863 ) ;
#24151 = CARTESIAN_POINT ( 'NONE',  ( 21.50111451137534146, -3.256483526998273983E-15, 2.499999999999998668 ) ) ;
#24152 = DIRECTION ( 'NONE',  ( 1.040834085586084257E-14, 0.000000000000000000, -1.000000000000000000 ) ) ;
#24153 = VECTOR ( 'NONE', #15426, 1000.000000000000000 ) ;
#24154 = VECTOR ( 'NONE', #2186, 1000.000000000000227 ) ;
#24155 = CARTESIAN_POINT ( 'NONE',  ( 101.9216173105994443, -5.769792427975438009, 0.07017451552781736601 ) ) ;
#24156 = PLANE ( 'NONE',  #28481 ) ;
#24158 = CARTESIAN_POINT ( 'NONE',  ( 108.0286932287532409, -18.48253747268860536, 4.344751374527882959 ) ) ;
#24157 = AXIS2_PLACEMENT_3D ( 'NONE', #6553, #26127, #3230 ) ;
#24159 = CARTESIAN_POINT ( 'NONE',  ( 6.399351475474185591, -16.64279405588517946, -5.485967528433938867 ) ) ;
#24160 = CARTESIAN_POINT ( 'NONE',  ( 47.95950916398559372, -8.432626694227655761, -0.4367665434710258365 ) ) ;
#24161 = CARTESIAN_POINT ( 'NONE',  ( 25.75999999999999801, -2.208672634433321348E-15, -2.499999999999997780 ) ) ;
#24162 = VECTOR ( 'NONE', #31436, 1000.000000000000000 ) ;
#24163 = CARTESIAN_POINT ( 'NONE',  ( -31.57659242536668032, -27.93932300454937590, -1.000000000000000000 ) ) ;
#24164 = AXIS2_PLACEMENT_3D ( 'NONE', #3132, #25680, #304 ) ;
#24165 = LINE ( 'NONE', #31381, #19869 ) ;
#24166 = CARTESIAN_POINT ( 'NONE',  ( -4.562942409646513653, -3.366872799099910998E-15, -3.000000000000000000 ) ) ;
#24167 = CARTESIAN_POINT ( 'NONE',  ( 4.749760686538667009, -6.940565734314625423, 4.007137495034787555 ) ) ;
#24168 = CIRCLE ( 'NONE', #28460, 8.000000000000000000 ) ;
#24169 = VECTOR ( 'NONE', #14169, 1000.000000000000114 ) ;
#24170 = CARTESIAN_POINT ( 'NONE',  ( 108.0068349480237515, 18.21621961241920573, 4.414771370926588112 ) ) ;
#24171 = CARTESIAN_POINT ( 'NONE',  ( -4.700050802731189137, -2.853674364686378695, -1.549418761218566809 ) ) ;
#24172 = ORIENTED_EDGE ( 'NONE', *, *, #32900, .T. ) ;
#24173 = VECTOR ( 'NONE', #4541, 1000.000000000000000 ) ;
#24174 = CARTESIAN_POINT ( 'NONE',  ( -4.950050800000000528, 0.9222479816126443186, 3.113457007523260156 ) ) ;
#24175 = CARTESIAN_POINT ( 'NONE',  ( 84.48140976240843258, -4.087790770806424057, -3.993432235010177855 ) ) ;
#24176 = CARTESIAN_POINT ( 'NONE',  ( 8.706508905304414014, -1.271749511658974319, 1.000000000000000000 ) ) ;
#24177 = AXIS2_PLACEMENT_3D ( 'NONE', #1793, #24342, #21826 ) ;
#24178 = ORIENTED_EDGE ( 'NONE', *, *, #30056, .F. ) ;
#24179 = CARTESIAN_POINT ( 'NONE',  ( -6.957304906975410042, -1.062355717592095017, -2.999999999999999556 ) ) ;
#24180 = ORIENTED_EDGE ( 'NONE', *, *, #22454, .F. ) ;
#24181 = CARTESIAN_POINT ( 'NONE',  ( 0.8806224662995314478, -9.175208741423659831, 1.499999999999824363 ) ) ;
#24182 = APPROVAL_DATE_TIME ( #11485, #28639 ) ;
#24183 = ORIENTED_EDGE ( 'NONE', *, *, #19153, .T. ) ;
#24184 = CARTESIAN_POINT ( 'NONE',  ( 69.04182551544533908, -5.543251471631118754, 4.312042181584448741 ) ) ;
#24185 = EDGE_CURVE ( 'NONE', #29127, #24602, #30078, .T. ) ;
#24186 = EDGE_CURVE ( 'NONE', #21865, #9415, #32912, .T. ) ;
#24187 = DIRECTION ( 'NONE',  ( -1.000000000000000000, -0.000000000000000000, 0.000000000000000000 ) ) ;
#24188 = VECTOR ( 'NONE', #15314, 1000.000000000000000 ) ;
#24189 = CARTESIAN_POINT ( 'NONE',  ( 18.83159731376704826, -5.059626785708270624, -4.275175838844416099 ) ) ;
#24190 = CARTESIAN_POINT ( 'NONE',  ( 23.03249562537437711, -17.15537757201811786, -1.465178982930819052 ) ) ;
#24191 = DIRECTION ( 'NONE',  ( -0.000000000000000000, -0.000000000000000000, -1.000000000000000000 ) ) ;
#24192 = ADVANCED_FACE ( 'NONE', ( #28202 ), #26486, .F. ) ;
#24193 = AXIS2_PLACEMENT_3D ( 'NONE', #18021, #32760, #25027 ) ;
#24194 = ORIENTED_EDGE ( 'NONE', *, *, #18188, .T. ) ;
#24195 = DIRECTION ( 'NONE',  ( -0.000000000000000000, -0.000000000000000000, -1.000000000000000000 ) ) ;
#24196 = DIRECTION ( 'NONE',  ( 0.000000000000000000, 1.000000000000000000, 0.000000000000000000 ) ) ;
#24197 = VECTOR ( 'NONE', #21595, 1000.000000000000000 ) ;
#24198 = CARTESIAN_POINT ( 'NONE',  ( 2.274274201625318348, -5.222868219166783454, -9.680994141368850947 ) ) ;
#24199 = CIRCLE ( 'NONE', #9788, 8.749000000000002331 ) ;
#24201 = VERTEX_POINT ( 'NONE', #21185 ) ;
#24200 = CARTESIAN_POINT ( 'NONE',  ( 4.749760686538667009, -6.940565734314570356, -4.007137495034885255 ) ) ;
#24202 = CARTESIAN_POINT ( 'NONE',  ( -3.412550801365593411, -3.368539882008727115, -1.828967928396028064 ) ) ;
#24203 = DIRECTION ( 'NONE',  ( -0.000000000000000000, -0.000000000000000000, -1.000000000000000000 ) ) ;
#24204 = DIRECTION ( 'NONE',  ( 0.000000000000000000, 0.000000000000000000, 1.000000000000000000 ) ) ;
#24205 = CARTESIAN_POINT ( 'NONE',  ( 2.589202987961075397, -2.218054364314524740, -10.07394153291407335 ) ) ;
#24206 = CARTESIAN_POINT ( 'NONE',  ( 4.749760686538667009, -5.151476664237518044, 6.139290821770238438 ) ) ;
#24207 = APPROVAL_PERSON_ORGANIZATION ( #8018, #5764, #22904 ) ;
#24208 = DIRECTION ( 'NONE',  ( -0.000000000000000000, -1.000000000000000000, -0.000000000000000000 ) ) ;
#24209 = CYLINDRICAL_SURFACE ( 'NONE', #18780, 2.999999999999999112 ) ;
#24210 = CYLINDRICAL_SURFACE ( 'NONE', #24695, 2.999999999999999112 ) ;
#24211 = CARTESIAN_POINT ( 'NONE',  ( -1.694237876703142742, -1.500727999663424184, 4.522129901861159595 ) ) ;
#24212 = VERTEX_POINT ( 'NONE', #3480 ) ;
#24213 = CARTESIAN_POINT ( 'NONE',  ( 3.249999999999999556, 2.223716399045691183, -8.461683424509292450 ) ) ;
#24214 = ORIENTED_EDGE ( 'NONE', *, *, #15000, .T. ) ;
#24215 = FACE_OUTER_BOUND ( 'NONE', #24440, .T. ) ;
#24216 = CIRCLE ( 'NONE', #14039, 0.5000000000000004441 ) ;
#24217 = DIRECTION ( 'NONE',  ( 0.000000000000000000, -2.309263891220325604E-14, 1.000000000000000000 ) ) ;
#24218 = VECTOR ( 'NONE', #303, 1000.000000000000000 ) ;
#24219 = CARTESIAN_POINT ( 'NONE',  ( -2.387550801365593056, 3.521866450007987037, 0.3701630799359328372 ) ) ;
#24220 = VECTOR ( 'NONE', #7247, 1000.000000000000227 ) ;
#24221 = CARTESIAN_POINT ( 'NONE',  ( 4.749760686538667009, 6.139290821770257089, 5.151476664237498504 ) ) ;
#24222 = CARTESIAN_POINT ( 'NONE',  ( 85.11758351742646767, -6.522238754302136954, 1.873788413188252067 ) ) ;
#24223 = EDGE_LOOP ( 'NONE', ( #25931, #27723, #9520, #260 ) ) ;
#24224 = CARTESIAN_POINT ( 'NONE',  ( -59.00528660915777124, -4.776024318451533190, 5.482724712897171671 ) ) ;
#24225 = AXIS2_PLACEMENT_3D ( 'NONE', #10103, #28328, #17819 ) ;
#24226 = ADVANCED_FACE ( 'NONE', ( #15673 ), #8620, .T. ) ;
#24227 = ORIENTED_EDGE ( 'NONE', *, *, #6923, .F. ) ;
#24228 = APPROVAL_DATE_TIME ( #17012, #8398 ) ;
#24230 = DIRECTION ( 'NONE',  ( 0.9947025833170223263, 0.1027947991993880261, -0.000000000000000000 ) ) ;
#24229 = LOCAL_TIME ( 16, 7, 10.00000000000000000, #963 ) ;
#24231 = CARTESIAN_POINT ( 'NONE',  ( 7.603296595623502796, -4.061113686736324446, -1.000000000000000222 ) ) ;
#24232 = ORIENTED_EDGE ( 'NONE', *, *, #28790, .F. ) ;
#24233 = CARTESIAN_POINT ( 'NONE',  ( 5.509727295071394693, 5.993169562190667321, 2.952988490976601099 ) ) ;
#24234 = ORIENTED_EDGE ( 'NONE', *, *, #13653, .T. ) ;
#24235 = EDGE_LOOP ( 'NONE', ( #24575, #11486, #2451, #14597 ) ) ;
#24236 = CARTESIAN_POINT ( 'NONE',  ( 0.000000000000000000, 0.000000000000000000, 0.000000000000000000 ) ) ;
#24237 = CARTESIAN_POINT ( 'NONE',  ( -4.212550801365593678, -3.368539882008727115, -1.828967928396027842 ) ) ;
#24238 = CARTESIAN_POINT ( 'NONE',  ( 23.42249999999999943, -2.378061970571983430, 1.291182301015471712 ) ) ;
#24239 = CARTESIAN_POINT ( 'NONE',  ( 0.8184811075176973150, -4.596091560410645371, -1.500000000000000000 ) ) ;
#24241 = ORIENTED_EDGE ( 'NONE', *, *, #2198, .T. ) ;
#24240 = DIRECTION ( 'NONE',  ( 3.469446951953478110E-15, -0.000000000000000000, -1.000000000000000000 ) ) ;
#24242 = VECTOR ( 'NONE', #2713, 1000.000000000000000 ) ;
#24243 = CARTESIAN_POINT ( 'NONE',  ( -5.337550801365593678, -1.828967928396026510, 3.368539882008728004 ) ) ;
#24244 = DIRECTION ( 'NONE',  ( 1.000000000000000000, 0.000000000000000000, 0.000000000000000000 ) ) ;
#24245 = DIRECTION ( 'NONE',  ( 0.000000000000000000, 0.000000000000000000, 1.000000000000000000 ) ) ;
#24246 = CARTESIAN_POINT ( 'NONE',  ( -56.33578448492038859, 0.003046479527604620090, 1.500000000000000000 ) ) ;
#24247 = ORIENTED_EDGE ( 'NONE', *, *, #21104, .F. ) ;
#24249 = EDGE_LOOP ( 'NONE', ( #14361, #253, #22992, #24671 ) ) ;
#24248 = FACE_OUTER_BOUND ( 'NONE', #1596, .T. ) ;
#24250 = CARTESIAN_POINT ( 'NONE',  ( 23.61000000273119070, -1.573300977624594976, 1.942864903642425700 ) ) ;
#24251 = CC_DESIGN_SECURITY_CLASSIFICATION ( #32825, ( #33105 ) ) ;
#24252 = EDGE_CURVE ( 'NONE', #28862, #2488, #26037, .T. ) ;
#24253 = DIRECTION ( 'NONE',  ( 0.000000000000000000, 1.000000000000000000, 0.000000000000000000 ) ) ;
#24254 = CARTESIAN_POINT ( 'NONE',  ( -29.34923860676941842, 14.86020659576501224, 1.860696004608973109 ) ) ;
#24255 = DIRECTION ( 'NONE',  ( 1.000000000000000000, 0.000000000000000000, 0.000000000000000000 ) ) ;
#24256 = LINE ( 'NONE', #14209, #16180 ) ;
#24257 = ADVANCED_FACE ( 'NONE', ( #13636 ), #21028, .F. ) ;
#24258 = DIRECTION ( 'NONE',  ( -0.000000000000000000, 0.08715574274765452989, 0.9961946980917458783 ) ) ;
#24259 = CARTESIAN_POINT ( 'NONE',  ( -2.737550801365594477, -3.368539882008727115, -1.828967928396028064 ) ) ;
#24260 = CARTESIAN_POINT ( 'NONE',  ( 48.09670199522224721, -9.430894477034977186, -0.07017451552783579571 ) ) ;
#24261 = ORIENTED_EDGE ( 'NONE', *, *, #14851, .T. ) ;
#24262 = AXIS2_PLACEMENT_3D ( 'NONE', #23834, #11124, #21325 ) ;
#24263 = SPHERICAL_SURFACE ( 'NONE', #19415, 0.5000000000000000000 ) ;
#24264 = EDGE_CURVE ( 'NONE', #12815, #27372, #23838, .T. ) ;
#24265 = CARTESIAN_POINT ( 'NONE',  ( 5.612718383992088889, 8.054241895195652035, -1.622626842546680104 ) ) ;
#24267 = DIRECTION ( 'NONE',  ( 0.000000000000000000, 0.000000000000000000, -1.000000000000000000 ) ) ;
#24266 = CYLINDRICAL_SURFACE ( 'NONE', #25183, 2.999999999999999112 ) ;
#24268 = EDGE_CURVE ( 'NONE', #16746, #12234, #11862, .T. ) ;
#24269 = VERTEX_POINT ( 'NONE', #10982 ) ;
#24270 = DIRECTION ( 'NONE',  ( 0.000000000000000000, 0.8660254037844362651, 0.5000000000000039968 ) ) ;
#24271 = VERTEX_POINT ( 'NONE', #16315 ) ;
#24272 = DIRECTION ( 'NONE',  ( -0.1908089953765452484, 0.000000000000000000, 0.9816271834476638647 ) ) ;
#24274 = ORIENTED_EDGE ( 'NONE', *, *, #14851, .F. ) ;
#24273 = CARTESIAN_POINT ( 'NONE',  ( 18.86045606321215118, -4.737043885707785229, -3.995006647709321790 ) ) ;
#24275 = ORIENTED_EDGE ( 'NONE', *, *, #30707, .T. ) ;
#24276 = EDGE_CURVE ( 'NONE', #27732, #7771, #16147, .T. ) ;
#24277 = FACE_OUTER_BOUND ( 'NONE', #13238, .T. ) ;
#24279 = ORIENTED_EDGE ( 'NONE', *, *, #26933, .F. ) ;
#24278 = CARTESIAN_POINT ( 'NONE',  ( 107.3891785634640570, -16.48386933944874855, 2.725368464337420527 ) ) ;
#24280 = DIRECTION ( 'NONE',  ( -0.4999999999999978906, -0.8660254037844399289, 0.000000000000000000 ) ) ;
#24281 = CARTESIAN_POINT ( 'NONE',  ( 2.655375060943963472, -12.56041828387959747, 1.000000000000000000 ) ) ;
#24282 = DIRECTION ( 'NONE',  ( 0.000000000000000000, 0.000000000000000000, -1.000000000000000000 ) ) ;
#24283 = CARTESIAN_POINT ( 'NONE',  ( 8.690654616497502261, -10.89241706857619540, -1.500000000000000000 ) ) ;
#24285 = VERTEX_POINT ( 'NONE', #8312 ) ;
#24284 = CARTESIAN_POINT ( 'NONE',  ( 107.9691564671736188, -17.62522291648321371, -4.956268131904038476 ) ) ;
#24286 = LINE ( 'NONE', #24108, #17283 ) ;
#24287 = EDGE_CURVE ( 'NONE', #1302, #11856, #24665, .T. ) ;
#24288 = CARTESIAN_POINT ( 'NONE',  ( 3.063284526839889832, 3.174628368996186278, -8.152713396088721254 ) ) ;
#24289 = DIRECTION ( 'NONE',  ( -8.326672684688671588E-17, -0.3746065934159163446, 0.9271838545667856479 ) ) ;
#24290 = DESIGN_CONTEXT ( 'detailed design', #17589, 'design' ) ;
#24291 = CARTESIAN_POINT ( 'NONE',  ( 0.3285611067768013926, -13.34342412962908497, 4.522129901861158707 ) ) ;
#24292 = CARTESIAN_POINT ( 'NONE',  ( 69.32965659118902124, -6.955028994473984483, -4.522129901861164036 ) ) ;
#24293 = ORIENTED_EDGE ( 'NONE', *, *, #27142, .T. ) ;
#24294 = DIRECTION ( 'NONE',  ( -1.000000000000000000, -0.000000000000000000, -0.000000000000000000 ) ) ;
#24295 = ADVANCED_BREP_SHAPE_REPRESENTATION ( '', ( #10563, #2865 ), #7630 ) ;
#24296 = CLOSED_SHELL ( 'NONE', ( #26993, #32514, #2481, #12005, #6851, #22320, #7117, #7304, #18149, #6729, #15290, #17532, #20200, #20343, #20085, #1233, #30511, #7217, #21210, #26472, #16149, #19620, #6647, #24226, #3597, #32702, #24888, #7826, #23261, #7776, #23106, #19374, #16098, #30873, #13317, #13075, #27957, #16525, #18471, #31279, #5497, #295, #7929, #31835, #3037, #30692, #29274, #32252, #20009, #29676, #25569, #18982, #3846, #4096, #13301, #1644, #26697, #18137, #24879, #7319, #17937, #1590, #67, #17585, #14225, #16938, #13669, #14042, #20801, #26829, #13255, #25878, #282, #3564, #4758, #13547, #25411, #5711, #31765, #25953, #31378, #23223, #25716, #3386, #12739, #4612, #3675, #15802, #2067, #28042, #20505, #28143, #123, #6476, #10553, #15982, #19228, #1053, #2279, #18130, #6325, #20556, #31474, #12606, #8513, #32681, #27895, #494, #29377, #26708, #18800, #19121, #18124, #7966, #23881 ) ) ;
#24297 = CARTESIAN_POINT ( 'NONE',  ( -5.521001242456725855, 0.4999999999999998890, -5.764947386686739783 ) ) ;
#24298 = PLANE ( 'NONE',  #26371 ) ;
#24299 = VERTEX_POINT ( 'NONE', #458 ) ;
#24300 = CARTESIAN_POINT ( 'NONE',  ( 25.11000000273118715, 1.573300977624590313, -1.942864903642426144 ) ) ;
#24301 = EDGE_CURVE ( 'NONE', #9041, #533, #28742, .T. ) ;
#24302 = CARTESIAN_POINT ( 'NONE',  ( 46.92593983402662872, 24.78664516185572708, -5.396302277755718357 ) ) ;
#24303 = ORIENTED_EDGE ( 'NONE', *, *, #13683, .F. ) ;
#24304 = CARTESIAN_POINT ( 'NONE',  ( 7.308590057547465157, -13.58425266979916124, -1.500000000000000444 ) ) ;
#24305 = EDGE_CURVE ( 'NONE', #16462, #22307, #16645, .T. ) ;
#24306 = EDGE_LOOP ( 'NONE', ( #21876, #20946, #2245, #32511, #4013 ) ) ;
#24307 = ORIENTED_EDGE ( 'NONE', *, *, #24501, .F. ) ;
#24308 = CARTESIAN_POINT ( 'NONE',  ( 24.83519197235521148, -17.49564329958954545, -1.498842795365640690 ) ) ;
#24309 = APPROVAL_ROLE ( '' ) ;
#24311 = VERTEX_POINT ( 'NONE', #18161 ) ;
#24310 = CARTESIAN_POINT ( 'NONE',  ( 3.830085165118310759E-16, 4.467071865485471527, 1.625881193364712596 ) ) ;
#24312 = VERTEX_POINT ( 'NONE', #8459 ) ;
#24313 = CARTESIAN_POINT ( 'NONE',  ( 24.23500000136559507, -1.570731468192933633, -2.892927487894330962 ) ) ;
#24314 = EDGE_CURVE ( 'NONE', #13727, #22830, #18652, .T. ) ;
#24315 = ORIENTED_EDGE ( 'NONE', *, *, #5697, .F. ) ;
#24316 = CARTESIAN_POINT ( 'NONE',  ( 26.08945412691624099, 19.05746434167065928, 1.050000000000000044 ) ) ;
#24317 = LINE ( 'NONE', #32194, #32634 ) ;
#24319 = ORIENTED_EDGE ( 'NONE', *, *, #14425, .T. ) ;
#24318 = DIRECTION ( 'NONE',  ( -0.8476835837759374437, 0.5305021600302710638, 0.000000000000000000 ) ) ;
#24320 = CARTESIAN_POINT ( 'NONE',  ( 2.619932554246560023E-16, 3.055657119358801133, 3.641590349731939735 ) ) ;
#24321 = CARTESIAN_POINT ( 'NONE',  ( -12.44989959798873791, 19.50000000000000000, -1.818740222761502601 ) ) ;
#24322 = DIRECTION ( 'NONE',  ( 1.000000000000000000, -8.574039729943018344E-17, -0.000000000000000000 ) ) ;
#24323 = DIRECTION ( 'NONE',  ( 0.000000000000000000, 0.000000000000000000, 1.000000000000000000 ) ) ;
#24324 = FACE_OUTER_BOUND ( 'NONE', #3788, .T. ) ;
#24325 = EDGE_CURVE ( 'NONE', #23377, #8422, #28552, .T. ) ;
#24326 =( BOUNDED_CURVE ( )  B_SPLINE_CURVE ( 2, ( #17574, #22126, #9399, #14745, #10054, #27118, #19765, #20267, #24943, #12228, #22435 ),
 .UNSPECIFIED., .F., .F. ) 
 B_SPLINE_CURVE_WITH_KNOTS ( ( 3, 2, 2, 2, 2, 3 ),
 ( 0.3966116191895003862, 0.4000000000000000222, 0.4249999999999999889, 0.4500000000000000111, 0.4749999999999999778, 0.4966116191895003640 ),
 .UNSPECIFIED. ) 
 CURVE ( )  GEOMETRIC_REPRESENTATION_ITEM ( )  RATIONAL_B_SPLINE_CURVE ( ( 0.9821626249036858880, 0.9896829947469992783, 1.000000000000000000, 0.9238795325112867385, 1.000000000000000000, 0.9238795325112867385, 1.000000000000000000, 0.9238795325112867385, 1.000000000000000000, 0.9341965377642874602, 0.9821626249036858880 ) ) 
 REPRESENTATION_ITEM ( '' )  );
#24327 = CARTESIAN_POINT ( 'NONE',  ( 10.00000000000000000, 4.116875700062082366, 2.376879293651078751 ) ) ;
#24328 = CARTESIAN_POINT ( 'NONE',  ( 79.17573959169237696, 22.98125563777605151, 4.629213727441585213 ) ) ;
#24329 = CARTESIAN_POINT ( 'NONE',  ( 10.55147673363118876, -2.376879293651094294, 4.116875700062075261 ) ) ;
#24330 = CARTESIAN_POINT ( 'NONE',  ( 25.75999999999999801, 5.000000000000000000, 0.000000000000000000 ) ) ;
#24331 = CARTESIAN_POINT ( 'NONE',  ( 2.598264985223430301, 0.000000000000000000, -5.684322216989628807 ) ) ;
#24332 = FACE_OUTER_BOUND ( 'NONE', #7518, .T. ) ;
#24333 = DIRECTION ( 'NONE',  ( 0.000000000000000000, 0.000000000000000000, -1.000000000000000000 ) ) ;
#24334 = CARTESIAN_POINT ( 'NONE',  ( -5.350050802731187716, 0.3135853898029611342, -2.983565686104819648 ) ) ;
#24335 = VERTEX_POINT ( 'NONE', #26192 ) ;
#24336 = ADVANCED_FACE ( 'NONE', ( #3301 ), #32025, .T. ) ;
#24337 = CARTESIAN_POINT ( 'NONE',  ( -6.750050800000001239, 3.113457007523260156, -0.9222479816126439855 ) ) ;
#24338 = CARTESIAN_POINT ( 'NONE',  ( 22.93781385240136572, -21.92295985586710572, -1.128554941024477953 ) ) ;
#24339 = CYLINDRICAL_SURFACE ( 'NONE', #8195, 10.96966150227469328 ) ;
#24340 = CARTESIAN_POINT ( 'NONE',  ( 6.653983693896913465, -6.711078333449102651, 1.500000000000000000 ) ) ;
#24341 = ORIENTED_EDGE ( 'NONE', *, *, #15570, .T. ) ;
#24342 = DIRECTION ( 'NONE',  ( 0.000000000000000000, 0.000000000000000000, 1.000000000000000000 ) ) ;
#24343 = ORIENTED_EDGE ( 'NONE', *, *, #7407, .T. ) ;
#24344 = CARTESIAN_POINT ( 'NONE',  ( 0.3598463914740824832, -8.266277061147796701, 1.772553072661675166 ) ) ;
#24345 = PERSON_AND_ORGANIZATION ( #6766, #25292 ) ;
#24346 = DIRECTION ( 'NONE',  ( -1.000000000000000000, 0.000000000000000000, 0.000000000000000000 ) ) ;
#24347 = VERTEX_POINT ( 'NONE', #22168 ) ;
#24348 = CARTESIAN_POINT ( 'NONE',  ( 54.94547365669386352, -5.359363431748539242, 3.993434333351774779 ) ) ;
#24349 = CYLINDRICAL_SURFACE ( 'NONE', #8042, 5.010000000000000675 ) ;
#24350 = CARTESIAN_POINT ( 'NONE',  ( 84.97133056964233333, -4.152779584596041573, -4.112223744635283396 ) ) ;
#24351 = CARTESIAN_POINT ( 'NONE',  ( 24.14342515507837561, -17.38895391569489135, -1.425886477553355736 ) ) ;
#24352 = LINE ( 'NONE', #11001, #6492 ) ;
#24353 = ORIENTED_EDGE ( 'NONE', *, *, #9103, .F. ) ;
#24354 = CYLINDRICAL_SURFACE ( 'NONE', #4506, 0.5000000000000000000 ) ;
#24355 = CARTESIAN_POINT ( 'NONE',  ( 6.037141848526922594, -7.798898458906302622, 3.315649934461692983 ) ) ;
#24357 = ORIENTED_EDGE ( 'NONE', *, *, #31420, .F. ) ;
#24356 = CARTESIAN_POINT ( 'NONE',  ( 25.65417410921524421, 2.315637413981730841, -1.793282383124906065 ) ) ;
#24358 = DIRECTION ( 'NONE',  ( -1.000000000000000000, -0.000000000000000000, 0.000000000000000000 ) ) ;
#24359 = CARTESIAN_POINT ( 'NONE',  ( 102.5305753040692878, -0.1042037546421146210, 0.07017451552781951707 ) ) ;
#24360 = CARTESIAN_POINT ( 'NONE',  ( 42.35322304602171783, -22.56891886512033096, -4.522129901861166701 ) ) ;
#24361 = CYLINDRICAL_SURFACE ( 'NONE', #27822, 6.000000000000000000 ) ;
#24362 = CARTESIAN_POINT ( 'NONE',  ( 0.5640491561247187313, 9.516580665849673437, 0.6680154998105086728 ) ) ;
#24363 = CARTESIAN_POINT ( 'NONE',  ( 5.489343806296446360, -1.307372367723691919, 8.012901424861405886 ) ) ;
#24364 = LINE ( 'NONE', #17499, #12903 ) ;
#24365 = DIRECTION ( 'NONE',  ( 0.000000000000000000, 0.000000000000000000, 1.000000000000000000 ) ) ;
#24366 = ORIENTED_EDGE ( 'NONE', *, *, #15105, .T. ) ;
#24367 = CARTESIAN_POINT ( 'NONE',  ( 21.00111451137534146, -1.283275288181523244E-15, -2.499999999999998668 ) ) ;
#24368 = VERTEX_POINT ( 'NONE', #19002 ) ;
#24369 = ADVANCED_FACE ( 'NONE', ( #21665 ), #11781, .F. ) ;
#24370 = CYLINDRICAL_SURFACE ( 'NONE', #3365, 8.025310301077755781 ) ;
#24371 = CARTESIAN_POINT ( 'NONE',  ( -58.44930958907092844, -3.890057978239433112, 5.414538096233303399 ) ) ;
#24372 = EDGE_CURVE ( 'NONE', #26262, #285, #32211, .T. ) ;
#24373 = CARTESIAN_POINT ( 'NONE',  ( 18.74780019990318536, -5.996310340153152119, -5.695980980372493008 ) ) ;
#24374 = CARTESIAN_POINT ( 'NONE',  ( 12.96639998074314271, 0.000000000000000000, 9.444203806868394224 ) ) ;
#24375 = CARTESIAN_POINT ( 'NONE',  ( 0.5640492482715756539, -5.053269777829524578, -8.091724846341634247 ) ) ;
#24376 = ORIENTED_EDGE ( 'NONE', *, *, #5503, .F. ) ;
#24377 = CARTESIAN_POINT ( 'NONE',  ( 107.3512941337730950, 17.37330583879339940, -3.572537589583222317 ) ) ;
#24378 = VERTEX_POINT ( 'NONE', #9094 ) ;
#24379 = CALENDAR_DATE ( 2026, 6, 10 ) ;
#24380 = CARTESIAN_POINT ( 'NONE',  ( 102.4232231159381286, -3.998796565576680617, 3.995006639018732653 ) ) ;
#24381 = CARTESIAN_POINT ( 'NONE',  ( 7.215348531073052740, -5.907639145588611029, -0.9999999999999997780 ) ) ;
#24382 = EDGE_LOOP ( 'NONE', ( #6250, #30506 ) ) ;
#24383 = DIRECTION ( 'NONE',  ( 8.281886410780523353E-17, 0.9659258262890698665, -0.2588190451025149663 ) ) ;
#24384 = ORIENTED_EDGE ( 'NONE', *, *, #4891, .T. ) ;
#24385 = EDGE_LOOP ( 'NONE', ( #13033, #20916, #13571, #19547, #13066 ) ) ;
#24386 = CARTESIAN_POINT ( 'NONE',  ( 25.75999999999999801, -2.208672634433321348E-15, 0.000000000000000000 ) ) ;
#24387 = CARTESIAN_POINT ( 'NONE',  ( 10.00000000000000000, -3.641590349731909537, -3.055657119358837992 ) ) ;
#24388 = CARTESIAN_POINT ( 'NONE',  ( 21.73499999999999943, -0.2613211581691358698, -2.486304738420681559 ) ) ;
#24389 = CARTESIAN_POINT ( 'NONE',  ( 1.058453267035363021, -9.473955959261930460, -1.500000000000000222 ) ) ;
#24391 = ORIENTED_EDGE ( 'NONE', *, *, #16506, .T. ) ;
#24390 = CARTESIAN_POINT ( 'NONE',  ( 3.499999999999999556, -2.417132211460010005, -8.149077976821821778 ) ) ;
#24392 = CARTESIAN_POINT ( 'NONE',  ( -6.487550801365593145, 2.752080473201636845, -2.228590825266444142 ) ) ;
#24393 = CYLINDRICAL_SURFACE ( 'NONE', #4319, 0.5000000000000002220 ) ;
#24394 = PLANE ( 'NONE',  #15586 ) ;
#24395 = LINE ( 'NONE', #27075, #21997 ) ;
#24396 = ORIENTED_EDGE ( 'NONE', *, *, #29178, .F. ) ;
#24398 = VERTEX_POINT ( 'NONE', #11470 ) ;
#24397 = CARTESIAN_POINT ( 'NONE',  ( 5.612974384376780534, -7.013635602076178976, -4.279837954023545166 ) ) ;
#24399 = CARTESIAN_POINT ( 'NONE',  ( 7.249760686538667009, -4.007137495034861274, 6.940565734314584567 ) ) ;
#24400 = CARTESIAN_POINT ( 'NONE',  ( 20.73500000273118715, -2.486304738420683780, 0.2613211581691335383 ) ) ;
#24401 = EDGE_CURVE ( 'NONE', #14502, #24299, #11971, .T. ) ;
#24402 = CARTESIAN_POINT ( 'NONE',  ( 25.61000000136559507, 2.892927487894327410, -1.570731468192931635 ) ) ;
#24403 = EDGE_CURVE ( 'NONE', #3558, #16126, #22537, .T. ) ;
#24404 = FACE_OUTER_BOUND ( 'NONE', #18199, .T. ) ;
#24405 = CARTESIAN_POINT ( 'NONE',  ( -4.458024584373125876, -5.037940649430906248, -1.499999999999999112 ) ) ;
#24406 = DIRECTION ( 'NONE',  ( -1.000000000000000000, 8.574039729943018344E-17, -0.000000000000000000 ) ) ;
#24407 = PRODUCT_DEFINITION_SHAPE ( 'NONE', 'NONE',  #2068 ) ;
#24408 = CARTESIAN_POINT ( 'NONE',  ( 102.2233072702346419, -1.127920370132899475, 0.4367666012506544182 ) ) ;
#24409 = CARTESIAN_POINT ( 'NONE',  ( -4.087550801365593678, 2.752080473201636845, -2.228590825266444142 ) ) ;
#24410 = VERTEX_POINT ( 'NONE', #32379 ) ;
#24411 = PLANE ( 'NONE',  #31615 ) ;
#24412 = ORIENTED_EDGE ( 'NONE', *, *, #32430, .F. ) ;
#24413 = DIRECTION ( 'NONE',  ( -0.1027947991993877624, 0.9947025833170222153, 0.000000000000000000 ) ) ;
#24414 = CARTESIAN_POINT ( 'NONE',  ( 102.5829460782277351, -0.8583298743146002829, -2.713652344655542503 ) ) ;
#24416 = DIRECTION ( 'NONE',  ( 1.000000000000000000, -0.000000000000000000, -0.000000000000000000 ) ) ;
#24415 = CARTESIAN_POINT ( 'NONE',  ( 7.249760686538667009, -2.210816291636156006, -8.466096581343503402 ) ) ;
#24417 = VERTEX_POINT ( 'NONE', #13948 ) ;
#24418 = DIRECTION ( 'NONE',  ( -0.000000000000000000, 0.4226182617406968323, 0.9063077870366511579 ) ) ;
#24419 = ORIENTED_EDGE ( 'NONE', *, *, #8937, .T. ) ;
#24420 = CARTESIAN_POINT ( 'NONE',  ( 2.592584512317752665, -10.27797909967270229, 0.9926283730659328786 ) ) ;
#24422 = ORIENTED_EDGE ( 'NONE', *, *, #32156, .T. ) ;
#24421 = CARTESIAN_POINT ( 'NONE',  ( 102.3442575486588737, -2.858888224824346125, -3.999773674151783087 ) ) ;
#24423 = ORIENTED_EDGE ( 'NONE', *, *, #29639, .F. ) ;
#24424 = CYLINDRICAL_SURFACE ( 'NONE', #7065, 5.100000000000000533 ) ;
#24425 = DIRECTION ( 'NONE',  ( 0.000000000000000000, -0.9271838545667856479, -0.3746065934159162891 ) ) ;
#24427 = EDGE_LOOP ( 'NONE', ( #10259, #3570, #23448, #15295 ) ) ;
#24426 = CARTESIAN_POINT ( 'NONE',  ( -1.924618011135691642, -13.55759823803114550, -1.499999999999999556 ) ) ;
#24428 = CARTESIAN_POINT ( 'NONE',  ( 10.52016698344803558, 2.080188551888086934, -1.050000000000000044 ) ) ;
#24429 = EDGE_CURVE ( 'NONE', #31023, #15485, #16962, .T. ) ;
#24430 = CARTESIAN_POINT ( 'NONE',  ( -31.10918640827616244, -27.93932300454937590, 1.404595502311727362 ) ) ;
#24431 = CARTESIAN_POINT ( 'NONE',  ( 7.193574579131897906, -9.614801642833084472, -1.500000000000000000 ) ) ;
#24433 = ORIENTED_EDGE ( 'NONE', *, *, #22927, .F. ) ;
#24432 = CARTESIAN_POINT ( 'NONE',  ( 107.9509692546103139, -17.36333158048723035, -4.612881207896696090 ) ) ;
#24434 = CARTESIAN_POINT ( 'NONE',  ( 3.499999999999999556, 1.106368468154540263, -8.427689411260562480 ) ) ;
#24435 = EDGE_CURVE ( 'NONE', #20064, #13402, #6927, .T. ) ;
#24436 = DIRECTION ( 'NONE',  ( 1.000000000000000000, -0.000000000000000000, -0.000000000000000000 ) ) ;
#24437 = CARTESIAN_POINT ( 'NONE',  ( 4.749760686538667009, 8.385837730238846314E-14, -8.014274990069656823 ) ) ;
#24438 = DIRECTION ( 'NONE',  ( -0.03489949670250104552, 0.9993908270190956511, 0.000000000000000000 ) ) ;
#24439 = CARTESIAN_POINT ( 'NONE',  ( 0.7632845268398883443, -7.360373001730875053, -4.729683950898950329 ) ) ;
#24440 = EDGE_LOOP ( 'NONE', ( #13243, #13397, #20323, #26998 ) ) ;
#24441 = CARTESIAN_POINT ( 'NONE',  ( 0.5704035821693400621, 0.6538686328479551557, 9.519055809315281280 ) ) ;
#24442 = EDGE_CURVE ( 'NONE', #9082, #26824, #1292, .T. ) ;
#24443 = DIRECTION ( 'NONE',  ( 1.000000000000000000, -8.574039729943018344E-17, -0.000000000000000000 ) ) ;
#24444 = DIRECTION ( 'NONE',  ( 1.000000000000000000, -8.574039729943018344E-17, -0.000000000000000000 ) ) ;
#24445 = ORIENTED_EDGE ( 'NONE', *, *, #28744, .F. ) ;
#24446 = CARTESIAN_POINT ( 'NONE',  ( -8.000050800000000351, 1.467282277383798572, -3.195100177104094552 ) ) ;
#24447 = ADVANCED_FACE ( 'NONE', ( #3623 ), #9282, .F. ) ;
#24448 = DIRECTION ( 'NONE',  ( 1.000000000000000000, -8.574039729943018344E-17, -0.000000000000000000 ) ) ;
#24449 = ORIENTED_EDGE ( 'NONE', *, *, #31684, .F. ) ;
#24450 = LINE ( 'NONE', #22142, #18766 ) ;
#24451 = ORIENTED_EDGE ( 'NONE', *, *, #17083, .F. ) ;
#24452 = ORIENTED_EDGE ( 'NONE', *, *, #19557, .T. ) ;
#24453 = CARTESIAN_POINT ( 'NONE',  ( 25.29940076078040434, -17.51841556854384052, -1.122629911123405488 ) ) ;
#24455 = EDGE_LOOP ( 'NONE', ( #1832, #11595, #28751, #16026 ) ) ;
#24454 = DIRECTION ( 'NONE',  ( -1.000000000000000000, -0.000000000000000000, -0.000000000000000000 ) ) ;
#24456 = ORIENTED_EDGE ( 'NONE', *, *, #6491, .T. ) ;
#24457 = CARTESIAN_POINT ( 'NONE',  ( 23.29750000136559862, -0.3178988483021076838, -3.024605502323848949 ) ) ;
#24458 = ORIENTED_EDGE ( 'NONE', *, *, #11240, .F. ) ;
#24459 = DIRECTION ( 'NONE',  ( -1.000000000000000000, -0.000000000000000000, -0.000000000000000000 ) ) ;
#24460 = PLANE ( 'NONE',  #2200 ) ;
#24462 = VERTEX_POINT ( 'NONE', #6618 ) ;
#24461 = FACE_OUTER_BOUND ( 'NONE', #14948, .T. ) ;
#24463 = DIRECTION ( 'NONE',  ( 0.000000000000000000, 0.000000000000000000, 1.000000000000000000 ) ) ;
#24464 = CARTESIAN_POINT ( 'NONE',  ( -56.40999100167014291, 0.01723988236541950519, -1.011943104398846049 ) ) ;
#24465 = ADVANCED_FACE ( 'NONE', ( #6773 ), #8940, .F. ) ;
#24466 = CARTESIAN_POINT ( 'NONE',  ( 5.887529755120530339, 1.089605374054371856, 8.323904922804400641 ) ) ;
#24467 = DIRECTION ( 'NONE',  ( -0.9975973382524639943, -0.06927878976713693071, 0.000000000000000000 ) ) ;
#24468 = CARTESIAN_POINT ( 'NONE',  ( 3.544356706773102328, -14.29624599654279393, -5.485967528433937979 ) ) ;
#24469 = CARTESIAN_POINT ( 'NONE',  ( 85.14283307489681363, -6.932413485865820846, -0.07017451552783708635 ) ) ;
#24470 = DIRECTION ( 'NONE',  ( 0.000000000000000000, 0.000000000000000000, 1.000000000000000000 ) ) ;
#24471 = EDGE_CURVE ( 'NONE', #10785, #9954, #13783, .T. ) ;
#24472 = ADVANCED_FACE ( 'NONE', ( #24332 ), #4264, .F. ) ;
#24473 = CARTESIAN_POINT ( 'NONE',  ( 9.999999999999998224, -4.681538312723512618, -0.8254815157535732029 ) ) ;
#24474 = CYLINDRICAL_SURFACE ( 'NONE', #6506, 5.010000000000000675 ) ;
#24475 = CARTESIAN_POINT ( 'NONE',  ( 23.73500000273118715, -2.486304738420683780, 0.2613211581691335383 ) ) ;
#24476 = CARTESIAN_POINT ( 'NONE',  ( 21.60999999999999943, -1.942864903642428587, -1.573300977624592756 ) ) ;
#24477 = EDGE_CURVE ( 'NONE', #14922, #12461, #9734, .T. ) ;
#24478 = CARTESIAN_POINT ( 'NONE',  ( -5.200050802731187360, 3.113457007523260156, -0.9222479816126439855 ) ) ;
#24479 = ORIENTED_EDGE ( 'NONE', *, *, #25085, .T. ) ;
#24480 = CARTESIAN_POINT ( 'NONE',  ( -7.737550801365593145, -1.828967928396026510, 3.368539882008728004 ) ) ;
#24481 = DIRECTION ( 'NONE',  ( -1.000000000000000000, -0.000000000000000000, -0.000000000000000000 ) ) ;
#24482 = CARTESIAN_POINT ( 'NONE',  ( 0.000000000000000000, 0.000000000000000000, -6.999999999999998224 ) ) ;
#24483 = CARTESIAN_POINT ( 'NONE',  ( 7.230698036208883295, -5.790874022015763067, 1.000000000000000000 ) ) ;
#24484 = EDGE_LOOP ( 'NONE', ( #3566, #6894, #5365, #12292 ) ) ;
#24485 = LINE ( 'NONE', #29702, #2662 ) ;
#24486 = DIRECTION ( 'NONE',  ( 0.000000000000000000, 0.000000000000000000, 1.000000000000000000 ) ) ;
#24487 = EDGE_CURVE ( 'NONE', #7070, #32887, #15337, .T. ) ;
#24488 = VERTEX_POINT ( 'NONE', #9941 ) ;
#24489 = CARTESIAN_POINT ( 'NONE',  ( 5.359215096090147235, -13.14304817624114285, 1.756412860341782789 ) ) ;
#24490 = APPLICATION_PROTOCOL_DEFINITION ( 'international standard', 'config_control_design', 1994, #2234 ) ;
#24491 = DIRECTION ( 'NONE',  ( -1.000000000000000000, -0.000000000000000000, -0.000000000000000000 ) ) ;
#24492 = ORIENTED_EDGE ( 'NONE', *, *, #12657, .T. ) ;
#24493 = CARTESIAN_POINT ( 'NONE',  ( 8.694260012178464336, -0.3977034846782427358, -1.500000000000002442 ) ) ;
#24494 = B_SPLINE_CURVE_WITH_KNOTS ( 'NONE', 3,
 ( #16810, #9592, #29335, #3959 ),
 .UNSPECIFIED., .F., .F.,
 ( 4, 4 ),
 ( 0.002128777998666837260, 0.002455751998630970826 ),
 .UNSPECIFIED. ) ;
#24495 = DIRECTION ( 'NONE',  ( -1.000000000000000000, 0.000000000000000000, 0.000000000000000000 ) ) ;
#24496 = CARTESIAN_POINT ( 'NONE',  ( 18.76278968803789127, -5.828757946052309791, -4.074610069491733988 ) ) ;
#24497 = CARTESIAN_POINT ( 'NONE',  ( 23.74728587540558422, -17.43182369245569063, -1.598909884665929315 ) ) ;
#24498 = LINE ( 'NONE', #9969, #8563 ) ;
#24499 = EDGE_LOOP ( 'NONE', ( #17855, #32330, #21392, #4202 ) ) ;
#24500 = DIRECTION ( 'NONE',  ( -1.000000000000000000, 8.574039729943022041E-17, 1.232595164407830946E-32 ) ) ;
#24501 = EDGE_CURVE ( 'NONE', #10426, #8063, #29504, .T. ) ;
#24502 = CARTESIAN_POINT ( 'NONE',  ( 23.13226153066252522, -21.93404782914821993, -1.074068642721640376 ) ) ;
#24503 = CARTESIAN_POINT ( 'NONE',  ( 6.356382228872880624, -7.873648075250523348, 3.475951004017304946 ) ) ;
#24505 = ORIENTED_EDGE ( 'NONE', *, *, #28741, .T. ) ;
#24504 = CARTESIAN_POINT ( 'NONE',  ( -1.147424988311422256, 0.5000000000000000000, 7.899334717979326292 ) ) ;
#24506 = FACE_OUTER_BOUND ( 'NONE', #7978, .T. ) ;
#24507 = CARTESIAN_POINT ( 'NONE',  ( 6.038145208238973716, -3.842870190353647075, -7.553619661406949959 ) ) ;
#24508 = FACE_OUTER_BOUND ( 'NONE', #3118, .T. ) ;
#24509 = CARTESIAN_POINT ( 'NONE',  ( -23.35000000000000142, -10.96966150227469505, 4.000000000000000000 ) ) ;
#24510 = EDGE_CURVE ( 'NONE', #3811, #13648, #14554, .T. ) ;
#24511 = DIRECTION ( 'NONE',  ( 8.541412920197218582E-17, 0.9961946980917461003, -0.08715574274765119922 ) ) ;
#24512 = CARTESIAN_POINT ( 'NONE',  ( 24.35832023931450507, -17.33818253687174860, -1.317734466820339900 ) ) ;
#24513 = DIRECTION ( 'NONE',  ( -7.472768010110610900E-18, -0.08715574274765197638, -0.9961946980917461003 ) ) ;
#24514 = CARTESIAN_POINT ( 'NONE',  ( -29.55113075415135881, 8.128449843281648768, 2.033773019847134655 ) ) ;
#24515 = AXIS2_PLACEMENT_3D ( 'NONE', #4780, #25169, #12967 ) ;
#24516 = ORIENTED_EDGE ( 'NONE', *, *, #1543, .F. ) ;
#24517 = CARTESIAN_POINT ( 'NONE',  ( -2.800050802731187005, 3.113457007523260156, -0.9222479816126439855 ) ) ;
#24518 = EDGE_LOOP ( 'NONE', ( #28487, #30985, #20096, #1508 ) ) ;
#24519 = CARTESIAN_POINT ( 'NONE',  ( 4.749760686538667009, 5.151476664237477188, 6.139290821770273077 ) ) ;
#24520 = EDGE_CURVE ( 'NONE', #536, #32661, #169, .T. ) ;
#24521 = CIRCLE ( 'NONE', #18665, 0.4499999999999999001 ) ;
#24522 = CARTESIAN_POINT ( 'NONE',  ( 109.0735342931897378, 18.49854792216788368, 5.381233289707400225 ) ) ;
#24523 =( BOUNDED_CURVE ( )  B_SPLINE_CURVE ( 3, ( #24331, #11620, #32024, #19323 ),
 .UNSPECIFIED., .F., .F. ) 
 B_SPLINE_CURVE_WITH_KNOTS ( ( 4, 4 ),
 ( 0.2844899013887131067, 0.5370275574894030068 ),
 .UNSPECIFIED. ) 
 CURVE ( )  GEOMETRIC_REPRESENTATION_ITEM ( )  RATIONAL_B_SPLINE_CURVE ( ( 1.000000000000000000, 0.9946924518608444288, 0.9946924518608444288, 1.000000000000000000 ) ) 
 REPRESENTATION_ITEM ( '' )  );
#24524 = CARTESIAN_POINT ( 'NONE',  ( 10.00000000000000000, -0.8254815157534942660, -4.681538312723525053 ) ) ;
#24525 = CARTESIAN_POINT ( 'NONE',  ( 3.499999999999999556, 0.000000000000000000, 0.000000000000000000 ) ) ;
#24526 = CARTESIAN_POINT ( 'NONE',  ( 107.8775346209187234, 20.32496164342445510, 0.000000000000000000 ) ) ;
#24527 = ORIENTED_EDGE ( 'NONE', *, *, #16142, .T. ) ;
#24528 = CARTESIAN_POINT ( 'NONE',  ( 0.000000000000000000, 0.000000000000000000, 0.000000000000000000 ) ) ;
#24529 = ADVANCED_FACE ( 'NONE', ( #14631 ), #21746, .F. ) ;
#24530 = CC_DESIGN_PERSON_AND_ORGANIZATION_ASSIGNMENT ( #4858, #20241, ( #1899 ) ) ;
#24531 = ORIENTED_EDGE ( 'NONE', *, *, #18433, .F. ) ;
#24532 = COORDINATED_UNIVERSAL_TIME_OFFSET ( 0, 0, .AHEAD. ) ;
#24533 = CARTESIAN_POINT ( 'NONE',  ( 85.03550338738804726, -5.199678113354736730, 4.001039873195242791 ) ) ;
#24534 = VECTOR ( 'NONE', #6938, 1000.000000000000000 ) ;
#24535 = DIRECTION ( 'NONE',  ( 0.000000000000000000, 0.000000000000000000, -1.000000000000000000 ) ) ;
#24536 = AXIS2_PLACEMENT_3D ( 'NONE', #30688, #15266, #7256 ) ;
#24537 = CARTESIAN_POINT ( 'NONE',  ( 25.75999999999999801, -2.208672634433321348E-15, 0.000000000000000000 ) ) ;
#24538 = ORIENTED_EDGE ( 'NONE', *, *, #10999, .F. ) ;
#24539 = ORIENTED_EDGE ( 'NONE', *, *, #6392, .F. ) ;
#24540 = PLANE ( 'NONE',  #30059 ) ;
#24541 = CARTESIAN_POINT ( 'NONE',  ( 2.274274201621893976, 10.90201369671108722, -1.464956435144929570 ) ) ;
#24542 = EDGE_CURVE ( 'NONE', #10302, #280, #15616, .T. ) ;
#24543 = CARTESIAN_POINT ( 'NONE',  ( 24.54749999999999943, -2.594547506269383685, -0.7685399846772043020 ) ) ;
#24544 = CARTESIAN_POINT ( 'NONE',  ( 3.074330700587167620, -11.22349925427311312, -1.500000000000000000 ) ) ;
#24545 = B_SPLINE_CURVE_WITH_KNOTS ( 'NONE', 3,
 ( #20129, #28777, #3077, #15907, #5397, #30979, #10568, #16058, #30835, #28285 ),
 .UNSPECIFIED., .F., .F.,
 ( 4, 2, 2, 2, 4 ),
 ( 2.740849916237977078E-07, 0.0005478761651001723409, 0.001095478245208722241, 0.001643080325317271924, 0.002190682405425822040 ),
 .UNSPECIFIED. ) ;
#24546 = AXIS2_PLACEMENT_3D ( 'NONE', #26269, #20439, #15392 ) ;
#24548 = EDGE_LOOP ( 'NONE', ( #21579, #6152, #22019, #28037 ) ) ;
#24547 = CARTESIAN_POINT ( 'NONE',  ( 0.000000000000000000, 0.000000000000000000, 0.000000000000000000 ) ) ;
#24549 = CARTESIAN_POINT ( 'NONE',  ( -8.062550801365594211, 0.3701630799359330593, -3.521866450007987037 ) ) ;
#24550 = CARTESIAN_POINT ( 'NONE',  ( 10.56183597391177464, -4.753758587302148619, 0.000000000000000000 ) ) ;
#24551 = EDGE_CURVE ( 'NONE', #29952, #24347, #16155, .T. ) ;
#24552 = CARTESIAN_POINT ( 'NONE',  ( 102.9361373302715918, -5.944196040818414239, 2.713652344655544724 ) ) ;
#24553 = LINE ( 'NONE', #27423, #10344 ) ;
#24554 = ORIENTED_EDGE ( 'NONE', *, *, #2801, .F. ) ;
#24556 = VERTEX_POINT ( 'NONE', #22672 ) ;
#24555 = CARTESIAN_POINT ( 'NONE',  ( 13.56175523640557756, 21.92011675111214686, 1.183903575935491226 ) ) ;
#24557 = DIRECTION ( 'NONE',  ( 1.000000000000000000, -8.574039729943018344E-17, -0.000000000000000000 ) ) ;
#24558 = CARTESIAN_POINT ( 'NONE',  ( 7.249760686538667009, -5.064320921489867899, 7.135485519861982873 ) ) ;
#24559 = AXIS2_PLACEMENT_3D ( 'NONE', #4477, #32550, #9617 ) ;
#24560 = CARTESIAN_POINT ( 'NONE',  ( 10.56183597391177464, -0.2500000000000192624, 5.003758587302147731 ) ) ;
#24561 = AXIS2_PLACEMENT_3D ( 'NONE', #1472, #6801, #4139 ) ;
#24562 = CARTESIAN_POINT ( 'NONE',  ( -6.550050802731187005, -0.3135853898029607456, 2.983565686104819648 ) ) ;
#24563 = CARTESIAN_POINT ( 'NONE',  ( -4.548089889563796007, -6.140210766943967613, -1.500000000000000444 ) ) ;
#24564 = CYLINDRICAL_SURFACE ( 'NONE', #15668, 5.010000000000000675 ) ;
#24565 = CIRCLE ( 'NONE', #23527, 8.749000000000002331 ) ;
#24566 = CARTESIAN_POINT ( 'NONE',  ( 29.31981545343394657, -4.303267367674513899, 2.184956339553084437 ) ) ;
#24567 = CARTESIAN_POINT ( 'NONE',  ( -3.137550801365593500, 3.368539882008727115, 1.828967928396026954 ) ) ;
#24568 = ORIENTED_EDGE ( 'NONE', *, *, #24787, .T. ) ;
#24569 = FACE_OUTER_BOUND ( 'NONE', #15304, .T. ) ;
#24570 = ORIENTED_EDGE ( 'NONE', *, *, #10798, .T. ) ;
#24571 = AXIS2_PLACEMENT_3D ( 'NONE', #5712, #28453, #25950 ) ;
#24572 = DIRECTION ( 'NONE',  ( 1.000000000000000000, -8.574039729943018344E-17, -0.000000000000000000 ) ) ;
#24573 = CARTESIAN_POINT ( 'NONE',  ( 69.13057415542958495, -2.987362752436060642, -2.713652344655542503 ) ) ;
#24574 = CARTESIAN_POINT ( 'NONE',  ( 24.29160796521804144, -17.33532173511319385, 1.337584091083817928 ) ) ;
#24575 = ORIENTED_EDGE ( 'NONE', *, *, #24372, .T. ) ;
#24576 = CARTESIAN_POINT ( 'NONE',  ( 20.00016891673595154, -21.67414139014260144, 1.443203664631087069 ) ) ;
#24577 = ORIENTED_EDGE ( 'NONE', *, *, #6005, .F. ) ;
#24578 = FACE_OUTER_BOUND ( 'NONE', #3887, .T. ) ;
#24580 = VERTEX_POINT ( 'NONE', #7422 ) ;
#24579 = CARTESIAN_POINT ( 'NONE',  ( 102.3440636142975535, -2.856088703579951815, -3.995336663081834772 ) ) ;
#24581 = CIRCLE ( 'NONE', #21922, 5.010000000000000675 ) ;
#24582 = ORIENTED_EDGE ( 'NONE', *, *, #15769, .T. ) ;
#24583 = EDGE_CURVE ( 'NONE', #28828, #21569, #23208, .T. ) ;
#24584 = FACE_OUTER_BOUND ( 'NONE', #13195, .T. ) ;
#24585 = EDGE_CURVE ( 'NONE', #536, #25915, #3256, .T. ) ;
#24586 = VECTOR ( 'NONE', #23416, 1000.000000000000114 ) ;
#24587 = CARTESIAN_POINT ( 'NONE',  ( 69.10564588828751198, -2.490548236270822446, 1.915219082070892531 ) ) ;
#24589 = EDGE_LOOP ( 'NONE', ( #6185, #1419, #8481, #29742, #24615, #1612 ) ) ;
#24588 = CARTESIAN_POINT ( 'NONE',  ( 14.44929100883576822, -20.94157545051515967, -1.499999999999999334 ) ) ;
#24590 = CARTESIAN_POINT ( 'NONE',  ( 23.82349779659365652, 17.94250544621599630, -1.049999999999882361 ) ) ;
#24591 = CARTESIAN_POINT ( 'NONE',  ( 9.282537329960035777, 0.2172754300400975558, -1.041239158277174948 ) ) ;
#24592 = CARTESIAN_POINT ( 'NONE',  ( -3.910108620251236289, -3.305117197436432619, 1.500000000000158096 ) ) ;
#24593 = CARTESIAN_POINT ( 'NONE',  ( 7.230698036208976553, -5.790874022015092493, -1.000000000000000000 ) ) ;
#24595 = ORIENTED_EDGE ( 'NONE', *, *, #13334, .F. ) ;
#24594 = CARTESIAN_POINT ( 'NONE',  ( 108.0271645861481602, -18.46052539945377902, -4.398898937011770371 ) ) ;
#24596 = CARTESIAN_POINT ( 'NONE',  ( 2.970200582152835445, -7.065646041987108994, 5.831559621424839079 ) ) ;
#24597 = AXIS2_PLACEMENT_3D ( 'NONE', #23252, #20742, #3363 ) ;
#24598 = DIRECTION ( 'NONE',  ( -0.000000000000000000, -0.000000000000000000, -1.000000000000000000 ) ) ;
#24599 = CARTESIAN_POINT ( 'NONE',  ( 24.92250000136559507, -1.913930629741527500, 2.363507492473149618 ) ) ;
#24600 = CARTESIAN_POINT ( 'NONE',  ( 15.28872660057388977, 20.76088595412472415, -4.612695725900422872 ) ) ;
#24601 = CARTESIAN_POINT ( 'NONE',  ( -45.71000000000000085, -10.96999999999998643, 1.499999999999999556 ) ) ;
#24602 = VERTEX_POINT ( 'NONE', #2768 ) ;
#24603 = CARTESIAN_POINT ( 'NONE',  ( 0.1574692247319860738, 1.187839595765007639, 10.55579611470142964 ) ) ;
#24604 = AXIS2_PLACEMENT_3D ( 'NONE', #18999, #802, #29185 ) ;
#24605 = CARTESIAN_POINT ( 'NONE',  ( -2.476225935960405966, -0.3178988483021057410, 3.024605502323848949 ) ) ;
#24606 = CARTESIAN_POINT ( 'NONE',  ( 107.3477315916820913, -15.88627780335592732, -1.500000000000000000 ) ) ;
#24607 = EDGE_LOOP ( 'NONE', ( #1880, #14752, #1042, #28192 ) ) ;
#24608 = CIRCLE ( 'NONE', #83, 2.999999999999999112 ) ;
#24609 = AXIS2_PLACEMENT_3D ( 'NONE', #27914, #12352, #22572 ) ;
#24610 = CARTESIAN_POINT ( 'NONE',  ( -8.000050800000018114, 1.979734913925816908, -2.936190332390367086 ) ) ;
#24611 = CARTESIAN_POINT ( 'NONE',  ( 2.281627749324421028, -0.2935656086769635187, -1.757435426329174710 ) ) ;
#24612 = VERTEX_POINT ( 'NONE', #23166 ) ;
#24614 = CARTESIAN_POINT ( 'NONE',  ( 7.249760686538667009, 6.940565734314597002, 4.007137495034836405 ) ) ;
#24613 = AXIS2_PLACEMENT_3D ( 'NONE', #5597, #20642, #30696 ) ;
#24615 = ORIENTED_EDGE ( 'NONE', *, *, #28428, .F. ) ;
#24616 = AXIS2_PLACEMENT_3D ( 'NONE', #13092, #20630, #30838 ) ;
#24617 = VECTOR ( 'NONE', #30048, 1000.000000000000000 ) ;
#24618 = ADVANCED_FACE ( 'NONE', ( #18470 ), #23464, .T. ) ;
#24619 = VERTEX_POINT ( 'NONE', #3108 ) ;
#24620 = LINE ( 'NONE', #17097, #15595 ) ;
#24621 = COORDINATED_UNIVERSAL_TIME_OFFSET ( 0, 0, .AHEAD. ) ;
#24623 = ORIENTED_EDGE ( 'NONE', *, *, #30900, .T. ) ;
#24622 = CARTESIAN_POINT ( 'NONE',  ( 20.55463713078643195, -21.58103817311708283, -1.582345582279491847 ) ) ;
#24624 = ORIENTED_EDGE ( 'NONE', *, *, #13121, .T. ) ;
#24625 = CARTESIAN_POINT ( 'NONE',  ( 23.98500000136559507, -2.892927487894331406, 1.570731468192932523 ) ) ;
#24626 = VERTEX_POINT ( 'NONE', #762 ) ;
#24627 = B_SPLINE_CURVE_WITH_KNOTS ( 'NONE', 3,
 ( #31563, #646, #28720, #8647, #26404, #29067, #3161, #15993, #6154, #3505 ),
 .UNSPECIFIED., .F., .F.,
 ( 4, 2, 2, 2, 4 ),
 ( 4.336808689942017736E-18, 0.0001594250696560639969, 0.0003188501393121236571, 0.0006377002786242324606, 0.001275400557248461235 ),
 .UNSPECIFIED. ) ;
#24628 = CARTESIAN_POINT ( 'NONE',  ( 0.1574692253523927998, -2.132217800985108269, 10.40622129948746810 ) ) ;
#24629 = CARTESIAN_POINT ( 'NONE',  ( 5.489321606599601999, -7.593050043411094130, -2.874206582856486669 ) ) ;
#24631 = ORIENTED_EDGE ( 'NONE', *, *, #30019, .F. ) ;
#24630 = DIRECTION ( 'NONE',  ( 0.000000000000000000, -0.000000000000000000, -1.000000000000000000 ) ) ;
#24632 = DIRECTION ( 'NONE',  ( -0.000000000000000000, 0.000000000000000000, 1.000000000000000000 ) ) ;
#24633 = CARTESIAN_POINT ( 'NONE',  ( 2.970200414845727277, 2.288523046052883814, -8.870914041987591148 ) ) ;
#24634 = AXIS2_PLACEMENT_3D ( 'NONE', #25795, #12408, #7892 ) ;
#24635 = CARTESIAN_POINT ( 'NONE',  ( -56.69506688323772892, 0.2173071790064931286, 1.574469351512994386 ) ) ;
#24636 = CARTESIAN_POINT ( 'NONE',  ( 21.42250000136559507, -0.3178988483021076838, -3.024605502323848949 ) ) ;
#24637 = DIRECTION ( 'NONE',  ( 3.471561733563293027E-15, 0.000000000000000000, -1.000000000000000000 ) ) ;
#24638 = CIRCLE ( 'NONE', #28920, 6.248999999999999666 ) ;
#24639 = AXIS2_PLACEMENT_3D ( 'NONE', #6087, #1056, #13741 ) ;
#24640 = AXIS2_PLACEMENT_3D ( 'NONE', #28883, #26698, #1326 ) ;
#24641 = CARTESIAN_POINT ( 'NONE',  ( -2.223027892448373510, -2.927336879246196677, -4.522129901861166701 ) ) ;
#24642 = CARTESIAN_POINT ( 'NONE',  ( -12.44989959798873791, 19.51744974835125035, -12.99999999999999645 ) ) ;
#24643 = DIRECTION ( 'NONE',  ( -1.000000000000000000, 0.000000000000000000, 0.000000000000000000 ) ) ;
#24644 = CIRCLE ( 'NONE', #30020, 2.999999999999999112 ) ;
#24645 = AXIS2_PLACEMENT_3D ( 'NONE', #26773, #13572, #3567 ) ;
#24646 = AXIS2_PLACEMENT_3D ( 'NONE', #17521, #22556, #27899 ) ;
#24647 = CARTESIAN_POINT ( 'NONE',  ( -23.35000000000000142, -10.96966150227469505, 1.500000000000000000 ) ) ;
#24648 = CARTESIAN_POINT ( 'NONE',  ( -5.699736881468957961, 11.99440202994180993, -2.572806452144713152 ) ) ;
#24649 = DIRECTION ( 'NONE',  ( -1.000000000000000000, -0.000000000000000000, -0.000000000000000000 ) ) ;
#24650 = EDGE_CURVE ( 'NONE', #31589, #17452, #32740, .T. ) ;
#24651 = DIRECTION ( 'NONE',  ( 0.000000000000000000, 0.000000000000000000, -1.000000000000000000 ) ) ;
#24652 = CARTESIAN_POINT ( 'NONE',  ( -6.150050802731187538, 0.3135853898029611342, -2.983565686104819648 ) ) ;
#24653 = ORIENTED_EDGE ( 'NONE', *, *, #23710, .T. ) ;
#24654 = CARTESIAN_POINT ( 'NONE',  ( -4.800050800000000173, -2.331437884370912705, 1.887961173149512062 ) ) ;
#24655 = CIRCLE ( 'NONE', #10260, 300.7453860596896220 ) ;
#24656 = EDGE_CURVE ( 'NONE', #10967, #5620, #2056, .T. ) ;
#24657 = AXIS2_PLACEMENT_3D ( 'NONE', #15253, #15403, #10062 ) ;
#24658 = CARTESIAN_POINT ( 'NONE',  ( 25.75999999999999801, -1.902510934646483477E-15, 2.499999999999997780 ) ) ;
#24659 = CARTESIAN_POINT ( 'NONE',  ( 7.249760686538667009, 7.135485519861997972, 5.064320921489847471 ) ) ;
#24661 = VERTEX_POINT ( 'NONE', #5616 ) ;
#24660 = AXIS2_PLACEMENT_3D ( 'NONE', #134, #20354, #3479 ) ;
#24662 = CARTESIAN_POINT ( 'NONE',  ( -1.807304909706596519, 1.062355717592091686, 3.000000000000001332 ) ) ;
#24663 = FACE_OUTER_BOUND ( 'NONE', #22788, .T. ) ;
#24664 = CIRCLE ( 'NONE', #5486, 2.999999999999999556 ) ;
#24665 = CIRCLE ( 'NONE', #30575, 0.5000000000000000000 ) ;
#24666 = VECTOR ( 'NONE', #5788, 1000.000000000000000 ) ;
#24667 = ORIENTED_EDGE ( 'NONE', *, *, #13079, .T. ) ;
#24668 = CARTESIAN_POINT ( 'NONE',  ( 14.73511782699088357, -15.74768507728505362, 1.499999999999998668 ) ) ;
#24669 = PERSON_AND_ORGANIZATION_ROLE ( 'creator' ) ;
#24670 = DIRECTION ( 'NONE',  ( -1.000000000000000000, 0.000000000000000000, 0.000000000000000000 ) ) ;
#24672 = EDGE_CURVE ( 'NONE', #25199, #31261, #11338, .T. ) ;
#24671 = ORIENTED_EDGE ( 'NONE', *, *, #24325, .F. ) ;
#24673 = LINE ( 'NONE', #14651, #9694 ) ;
#24674 = CIRCLE ( 'NONE', #31640, 297.0265809045899346 ) ;
#24675 = ADVANCED_FACE ( 'NONE', ( #10763 ), #27382, .F. ) ;
#24676 = AXIS2_PLACEMENT_3D ( 'NONE', #31811, #16069, #8882 ) ;
#24677 = FACE_OUTER_BOUND ( 'NONE', #7366, .T. ) ;
#24678 = CARTESIAN_POINT ( 'NONE',  ( 40.88399151333042170, -6.896594116923616014, -3.993433839952781117 ) ) ;
#24679 = CARTESIAN_POINT ( 'NONE',  ( 5.612974044843318744, -1.622927203279397101, 8.054452210044754423 ) ) ;
#24680 = DIRECTION ( 'NONE',  ( 0.000000000000000000, -0.9659258262890662028, -0.2588190451025284000 ) ) ;
#24681 = ORIENTED_EDGE ( 'NONE', *, *, #14276, .T. ) ;
#24682 = EDGE_CURVE ( 'NONE', #17637, #22462, #1205, .T. ) ;
#24683 = FACE_OUTER_BOUND ( 'NONE', #12385, .T. ) ;
#24684 = CARTESIAN_POINT ( 'NONE',  ( 23.22564502775743378, -21.93932300456764040, -1.023882905581262825 ) ) ;
#24685 = DIRECTION ( 'NONE',  ( -1.000000000000000000, -5.361488761196502513E-16, 0.000000000000000000 ) ) ;
#24687 = ORIENTED_EDGE ( 'NONE', *, *, #3062, .T. ) ;
#24686 = CARTESIAN_POINT ( 'NONE',  ( 25.74353197755034373, 2.942305264091934713, 0.6717076152027443570 ) ) ;
#24688 = VECTOR ( 'NONE', #215, 1000.000000000000114 ) ;
#24689 = CARTESIAN_POINT ( 'NONE',  ( 6.883866357751288412, -8.704251636488463006, -0.6899766464187978565 ) ) ;
#24690 = AXIS2_PLACEMENT_3D ( 'NONE', #28774, #31313, #32308 ) ;
#24691 = CARTESIAN_POINT ( 'NONE',  ( 23.95058674323790271, -2.449331254364353949, 0.07017451552781951707 ) ) ;
#24692 = FACE_OUTER_BOUND ( 'NONE', #23016, .T. ) ;
#24693 = PLANE ( 'NONE',  #17677 ) ;
#24694 = CARTESIAN_POINT ( 'NONE',  ( -23.54713438637982748, 8.275374457817616047, 8.599999999999999645 ) ) ;
#24695 = AXIS2_PLACEMENT_3D ( 'NONE', #19372, #19186, #29886 ) ;
#24697 = EDGE_CURVE ( 'NONE', #299, #26246, #19147, .T. ) ;
#24696 = VECTOR ( 'NONE', #11434, 1000.000000000000000 ) ;
#24698 = CARTESIAN_POINT ( 'NONE',  ( -4.962942409646514008, 3.284080845023683730E-15, 3.000000000000000000 ) ) ;
#24699 = FACE_OUTER_BOUND ( 'NONE', #10986, .T. ) ;
#24700 = CARTESIAN_POINT ( 'NONE',  ( 24.36000000273118715, 1.942864903642424146, 1.573300977624592534 ) ) ;
#24701 = DIRECTION ( 'NONE',  ( -1.000000000000000000, 8.574039729943018344E-17, -0.000000000000000000 ) ) ;
#24702 = ORIENTED_EDGE ( 'NONE', *, *, #1309, .T. ) ;
#24703 = CIRCLE ( 'NONE', #18822, 5.009999999999999787 ) ;
#24704 = CARTESIAN_POINT ( 'NONE',  ( 20.99290772595112387, -0.1310194482076047495, -2.499999999999998668 ) ) ;
#24705 = VERTEX_POINT ( 'NONE', #28511 ) ;
#24706 = AXIS2_PLACEMENT_3D ( 'NONE', #3845, #29096, #31777 ) ;
#24707 = CARTESIAN_POINT ( 'NONE',  ( -6.254531657079159146, -2.846291840500172921, -1.545410377633947618 ) ) ;
#24708 = CARTESIAN_POINT ( 'NONE',  ( 24.97738509828242925, 18.93945643846228677, -1.491740999229418829 ) ) ;
#24709 = DIRECTION ( 'NONE',  ( -1.000000000000000000, 0.000000000000000000, -0.000000000000000000 ) ) ;
#24710 = CARTESIAN_POINT ( 'NONE',  ( 2.864531114197726769, 8.105385692883681159, -5.073635298885059264 ) ) ;
#24711 = CARTESIAN_POINT ( 'NONE',  ( -0.2059365608663963898, 0.000000000000000000, 4.148259000770580407 ) ) ;
#24712 = ORIENTED_EDGE ( 'NONE', *, *, #7278, .T. ) ;
#24713 = DIRECTION ( 'NONE',  ( -0.000000000000000000, -0.000000000000000000, 1.000000000000000000 ) ) ;
#24714 = EDGE_CURVE ( 'NONE', #22010, #16013, #10600, .T. ) ;
#24715 = AXIS2_PLACEMENT_3D ( 'NONE', #26691, #9127, #6800 ) ;
#24716 = ORIENTED_EDGE ( 'NONE', *, *, #7167, .F. ) ;
#24718 = AXIS2_PLACEMENT_3D ( 'NONE', #12165, #6818, #7171 ) ;
#24717 = COORDINATED_UNIVERSAL_TIME_OFFSET ( 0, 0, .AHEAD. ) ;
#24719 = EDGE_CURVE ( 'NONE', #19305, #4647, #5758, .T. ) ;
#24720 = CARTESIAN_POINT ( 'NONE',  ( 102.4226167450245697, -3.990043124566273303, 4.008637373575834495 ) ) ;
#24721 = AXIS2_PLACEMENT_3D ( 'NONE', #1560, #1248, #11743 ) ;
#24722 = EDGE_CURVE ( 'NONE', #20542, #7771, #29895, .T. ) ;
#24723 = AXIS2_PLACEMENT_3D ( 'NONE', #19428, #29621, #1879 ) ;
#24724 = AXIS2_PLACEMENT_3D ( 'NONE', #10231, #7895, #10721 ) ;
#24726 = CARTESIAN_POINT ( 'NONE',  ( 5.612717990268488499, -0.1993707932845431574, -8.213645783354287744 ) ) ;
#24725 = CARTESIAN_POINT ( 'NONE',  ( -50.81000000000000227, -10.96999999999998643, 9.000000000000000000 ) ) ;
#24727 = ORIENTED_EDGE ( 'NONE', *, *, #20160, .T. ) ;
#24728 = VERTEX_POINT ( 'NONE', #11741 ) ;
#24729 =( GEOMETRIC_REPRESENTATION_CONTEXT ( 3 ) GLOBAL_UNCERTAINTY_ASSIGNED_CONTEXT ( ( #25193 ) ) GLOBAL_UNIT_ASSIGNED_CONTEXT ( ( #24765, #13757, #30796 ) ) REPRESENTATION_CONTEXT ( 'NONE', 'WORKASPACE' ) );
#24730 = CARTESIAN_POINT ( 'NONE',  ( 0.6791197464446973031, -0.5477823182330034957, -9.138998021039025588 ) ) ;
#24731 = CARTESIAN_POINT ( 'NONE',  ( -2.412550801365592967, 1.828967928396027398, -3.368539882008727115 ) ) ;
#24732 = CARTESIAN_POINT ( 'NONE',  ( 22.98500000000000298, 2.486304738420679783, -0.2613211581691337604 ) ) ;
#24733 = CARTESIAN_POINT ( 'NONE',  ( 10.91170924523349584, -15.11896097446722464, -1.500000000000279110 ) ) ;
#24735 = ORIENTED_EDGE ( 'NONE', *, *, #27240, .T. ) ;
#24734 = CARTESIAN_POINT ( 'NONE',  ( -61.56966150227469114, -10.96966150227468972, -1.000000000000000000 ) ) ;
#24736 = CARTESIAN_POINT ( 'NONE',  ( -3.937550801365593323, 3.368539882008727115, 1.828967928396026954 ) ) ;
#24737 = CARTESIAN_POINT ( 'NONE',  ( 33.81874022276150527, 19.50000000000000000, -1.977928362984232802 ) ) ;
#24738 = CARTESIAN_POINT ( 'NONE',  ( 2.661997753583457360, -10.09011512947411937, -0.9074203448823074947 ) ) ;
#24739 = CARTESIAN_POINT ( 'NONE',  ( 108.0285590637735851, -18.48060553035694653, -4.343942861249384002 ) ) ;
#24740 = VERTEX_POINT ( 'NONE', #32169 ) ;
#24742 = ORIENTED_EDGE ( 'NONE', *, *, #13191, .F. ) ;
#24741 = DIRECTION ( 'NONE',  ( -1.000000000000000000, 8.574039729943018344E-17, -0.000000000000000000 ) ) ;
#24743 = EDGE_CURVE ( 'NONE', #26011, #6812, #5487, .T. ) ;
#24744 = CC_DESIGN_PERSON_AND_ORGANIZATION_ASSIGNMENT ( #30911, #30764, ( #31711 ) ) ;
#24745 = AXIS2_PLACEMENT_3D ( 'NONE', #14777, #7266, #22311 ) ;
#24746 = CARTESIAN_POINT ( 'NONE',  ( 107.3709349538546007, 17.48268201568652813, 3.822938398868985566 ) ) ;
#24747 =( BOUNDED_CURVE ( )  B_SPLINE_CURVE ( 3, ( #15825, #18501, #23680, #23347 ),
 .UNSPECIFIED., .F., .F. ) 
 B_SPLINE_CURVE_WITH_KNOTS ( ( 4, 4 ),
 ( 5.654238798699126711, 7.043025911564681607 ),
 .UNSPECIFIED. ) 
 CURVE ( )  GEOMETRIC_REPRESENTATION_ITEM ( )  RATIONAL_B_SPLINE_CURVE ( ( 1.000000000000000000, 0.8456279454424002751, 0.8456279454424002751, 1.000000000000000000 ) ) 
 REPRESENTATION_ITEM ( '' )  );
#24748 = AXIS2_PLACEMENT_3D ( 'NONE', #21116, #16056, #3707 ) ;
#24749 = DIRECTION ( 'NONE',  ( 1.000000000000000000, -0.000000000000000000, -0.000000000000000000 ) ) ;
#24750 = VECTOR ( 'NONE', #2491, 1000.000000000000114 ) ;
#24751 = AXIS2_PLACEMENT_3D ( 'NONE', #23324, #428, #5766 ) ;
#24752 = DIRECTION ( 'NONE',  ( 0.000000000000000000, -0.3090169943749350168, -0.9510565162951576390 ) ) ;
#24753 = VECTOR ( 'NONE', #13331, 1000.000000000000000 ) ;
#24754 = DIRECTION ( 'NONE',  ( -0.000000000000000000, -0.000000000000000000, -1.000000000000000000 ) ) ;
#24755 = CARTESIAN_POINT ( 'NONE',  ( -2.574540400785382044, -12.71128672357123968, -1.499999999999999556 ) ) ;
#24756 = CARTESIAN_POINT ( 'NONE',  ( 10.56870887191539587, -1.946309384392624464, 4.616489984850525197 ) ) ;
#24757 = LOCAL_TIME ( 16, 7, 10.00000000000000000, #7477 ) ;
#24758 = CARTESIAN_POINT ( 'NONE',  ( 18.96091535642496240, -3.614110606601101949, 2.184956778829998836 ) ) ;
#24759 = CARTESIAN_POINT ( 'NONE',  ( -3.087550801365593234, 2.228590825266444142, 2.752080473201636845 ) ) ;
#24760 = VERTEX_POINT ( 'NONE', #8575 ) ;
#24761 = CARTESIAN_POINT ( 'NONE',  ( 41.45135008765517881, -9.497951668093163491, -0.07017451552783579571 ) ) ;
#24762 = ORIENTED_EDGE ( 'NONE', *, *, #13166, .T. ) ;
#24763 = EDGE_CURVE ( 'NONE', #25765, #22691, #28986, .T. ) ;
#24764 = CARTESIAN_POINT ( 'NONE',  ( 21.21813830868136463, -21.75718202030616055, 1.395944860341482796 ) ) ;
#24765 =( LENGTH_UNIT ( ) NAMED_UNIT ( * ) SI_UNIT ( .MILLI., .METRE. ) );
#24766 = LINE ( 'NONE', #30585, #32570 ) ;
#24767 = CARTESIAN_POINT ( 'NONE',  ( -18.06457975862740284, -25.93932300454937945, 14.13101917082694392 ) ) ;
#24768 = ORIENTED_EDGE ( 'NONE', *, *, #9236, .T. ) ;
#24769 = AXIS2_PLACEMENT_3D ( 'NONE', #378, #12574, #7739 ) ;
#24770 = DIRECTION ( 'NONE',  ( -1.000000000000000000, -0.000000000000000000, -0.000000000000000000 ) ) ;
#24771 = ORIENTED_EDGE ( 'NONE', *, *, #6697, .F. ) ;
#24772 = CYLINDRICAL_SURFACE ( 'NONE', #694, 6.000000000000000888 ) ;
#24774 = ORIENTED_EDGE ( 'NONE', *, *, #18307, .F. ) ;
#24773 = CARTESIAN_POINT ( 'NONE',  ( 18.86036632877896935, -4.738046936575775803, -3.996604665406715107 ) ) ;
#24775 = ORIENTED_EDGE ( 'NONE', *, *, #29211, .T. ) ;
#24776 = CARTESIAN_POINT ( 'NONE',  ( 23.67250000000000298, -1.291182301015472600, -2.378061970571982098 ) ) ;
#24777 = DIRECTION ( 'NONE',  ( 1.000000000000000000, 0.000000000000000000, 0.000000000000000000 ) ) ;
#24779 = ORIENTED_EDGE ( 'NONE', *, *, #21248, .F. ) ;
#24778 = DIRECTION ( 'NONE',  ( 0.000000000000000000, 0.000000000000000000, 1.000000000000000000 ) ) ;
#24780 = CARTESIAN_POINT ( 'NONE',  ( 24.29583315733998816, 18.19363606257105914, -1.049999999999941425 ) ) ;
#24781 = CARTESIAN_POINT ( 'NONE',  ( -15.60935834747760609, -25.43932300454937945, 1.500000000000000000 ) ) ;
#24782 = CARTESIAN_POINT ( 'NONE',  ( 5.612974259723586989, -2.996912441296229801, 7.650268724902049122 ) ) ;
#24783 = APPROVAL_PERSON_ORGANIZATION ( #31359, #27393, #20674 ) ;
#24784 = CARTESIAN_POINT ( 'NONE',  ( 0.000000000000000000, -6.106419733534973027, -3.518755179752868223 ) ) ;
#24787 = EDGE_CURVE ( 'NONE', #8864, #32058, #26630, .T. ) ;
#24786 = ORIENTED_EDGE ( 'NONE', *, *, #16281, .F. ) ;
#24785 = CARTESIAN_POINT ( 'NONE',  ( 107.9564799961608941, -17.44268488772687675, -4.756047278368655817 ) ) ;
#24788 = CARTESIAN_POINT ( 'NONE',  ( 2.592584925146038888, -7.731606906650699607, 6.844296717724891010 ) ) ;
#24789 = CARTESIAN_POINT ( 'NONE',  ( 107.4385791398478744, 17.85938043952733878, 4.629213727441584325 ) ) ;
#24790 = CARTESIAN_POINT ( 'NONE',  ( -83.35439080561378944, -0.0003384977252891612984, 1.500000000000000000 ) ) ;
#24791 = DIRECTION ( 'NONE',  ( 0.000000000000000000, 0.000000000000000000, 1.000000000000000000 ) ) ;
#24792 = CARTESIAN_POINT ( 'NONE',  ( 10.00000000000000178, -8.574039729943018837E-16, 0.000000000000000000 ) ) ;
#24793 = LINE ( 'NONE', #21626, #28952 ) ;
#24794 = CIRCLE ( 'NONE', #31219, 5.010000000000000675 ) ;
#24795 = EDGE_LOOP ( 'NONE', ( #23965, #11625, #21037, #4198 ) ) ;
#24796 = CARTESIAN_POINT ( 'NONE',  ( 3.499999999999999556, 0.000000000000000000, 0.000000000000000000 ) ) ;
#24797 = DIRECTION ( 'NONE',  ( 0.000000000000000000, 0.000000000000000000, -1.000000000000000000 ) ) ;
#24798 = EDGE_CURVE ( 'NONE', #12771, #19976, #32191, .T. ) ;
#24799 = CARTESIAN_POINT ( 'NONE',  ( -5.487550801365593145, 2.228590825266444142, 2.752080473201636845 ) ) ;
#24800 = VERTEX_POINT ( 'NONE', #29482 ) ;
#24801 = EDGE_CURVE ( 'NONE', #30416, #7918, #11365, .T. ) ;
#24802 = EDGE_CURVE ( 'NONE', #7955, #2302, #24118, .T. ) ;
#24803 = CYLINDRICAL_SURFACE ( 'NONE', #9277, 0.5000000000000000000 ) ;
#24804 = CARTESIAN_POINT ( 'NONE',  ( 71.53201042710830393, -18.09776336787419382, -0.9788672205888330202 ) ) ;
#24805 = VERTEX_POINT ( 'NONE', #16929 ) ;
#24806 = CARTESIAN_POINT ( 'NONE',  ( 7.300970717157576395, -8.296229357995484222, 1.000000000000000000 ) ) ;
#24807 = ORIENTED_EDGE ( 'NONE', *, *, #5919, .T. ) ;
#24808 = ORIENTED_EDGE ( 'NONE', *, *, #23466, .T. ) ;
#24809 = DIRECTION ( 'NONE',  ( -1.000000000000000000, 0.000000000000000000, 0.000000000000000000 ) ) ;
#24811 = ORIENTED_EDGE ( 'NONE', *, *, #6044, .T. ) ;
#24810 = DIRECTION ( 'NONE',  ( 0.8660254037844409281, -0.4999999999999960587, 0.000000000000000000 ) ) ;
#24812 = ORIENTED_EDGE ( 'NONE', *, *, #19281, .F. ) ;
#24813 = CARTESIAN_POINT ( 'NONE',  ( 21.86000000136559507, -0.9349337715887247047, 3.156283516753367824 ) ) ;
#24814 = VERTEX_POINT ( 'NONE', #1733 ) ;
#24815 = CARTESIAN_POINT ( 'NONE',  ( 108.1300413742128228, -19.95926608421481063, -1.392287898180229133 ) ) ;
#24816 = AXIS2_PLACEMENT_3D ( 'NONE', #26793, #24289, #16419 ) ;
#24818 = ORIENTED_EDGE ( 'NONE', *, *, #25443, .T. ) ;
#24817 = CARTESIAN_POINT ( 'NONE',  ( 18.99190826319341596, -3.267672110760019510, -1.529339877370962553 ) ) ;
#24819 = CARTESIAN_POINT ( 'NONE',  ( -56.37268996909460128, 0.008707415260527892262, -1.007559461241812837 ) ) ;
#24820 = LINE ( 'NONE', #75, #2692 ) ;
#24821 = CARTESIAN_POINT ( 'NONE',  ( 24.42250000136559507, 1.913930629741522838, -2.363507492473150062 ) ) ;
#24822 = FACE_OUTER_BOUND ( 'NONE', #10566, .T. ) ;
#24823 = B_SPLINE_CURVE_WITH_KNOTS ( 'NONE', 3,
 ( #5974, #31078, #23858, #15502, #31253, #965, #642, #25719, #15989, #823 ),
 .UNSPECIFIED., .F., .F.,
 ( 4, 2, 2, 2, 4 ),
 ( 1.968338519003762927E-07, 0.0005467928198071716301, 0.001093388805762442921, 0.001639984791717713887, 0.002186580777672985070 ),
 .UNSPECIFIED. ) ;
#24824 = CARTESIAN_POINT ( 'NONE',  ( -2.461002521556598488, -6.738986457086101112, -5.485967528433938867 ) ) ;
#24825 = FACE_OUTER_BOUND ( 'NONE', #1212, .T. ) ;
#24826 = CARTESIAN_POINT ( 'NONE',  ( 10.00000000000000178, -8.574039729943018837E-16, 0.000000000000000000 ) ) ;
#24827 = EDGE_CURVE ( 'NONE', #27475, #24998, #1246, .T. ) ;
#24828 = CARTESIAN_POINT ( 'NONE',  ( 2.274274201625316572, -7.958834565716716547, -7.593217523260693547 ) ) ;
#24829 = CARTESIAN_POINT ( 'NONE',  ( 73.25280475360474952, -21.01694209586349515, 5.485967528433935314 ) ) ;
#24830 = CARTESIAN_POINT ( 'NONE',  ( 3.499999999999999556, 0.000000000000000000, 0.000000000000000000 ) ) ;
#24831 = CARTESIAN_POINT ( 'NONE',  ( 23.55656763645045615, -0.8852964313267484009, 2.499999999999997780 ) ) ;
#24832 = ADVANCED_FACE ( 'NONE', ( #27123 ), #17242, .T. ) ;
#24833 = CARTESIAN_POINT ( 'NONE',  ( -7.200050802731187360, -3.113457007523259268, 0.9222479816126455399 ) ) ;
#24834 = EDGE_LOOP ( 'NONE', ( #19588, #19900, #16793, #31017, #27467, #727, #27706, #20294, #24178, #22124, #22821, #12023 ) ) ;
#24835 = EDGE_CURVE ( 'NONE', #32538, #16234, #18403, .T. ) ;
#24836 = CARTESIAN_POINT ( 'NONE',  ( -3.250050800000000795, -1.549418761218565477, 2.853674364686380471 ) ) ;
#24837 = CARTESIAN_POINT ( 'NONE',  ( -50.81000000000000227, 4.402097243136370963, 5.049999999999999822 ) ) ;
#24838 = DIRECTION ( 'NONE',  ( -1.000000000000000000, 0.000000000000000000, 0.000000000000000000 ) ) ;
#24839 = VERTEX_POINT ( 'NONE', #16276 ) ;
#24840 = PLANE ( 'NONE',  #15451 ) ;
#24841 = CARTESIAN_POINT ( 'NONE',  ( 0.000000000000000000, 0.000000000000000000, 0.000000000000000000 ) ) ;
#24842 = EDGE_LOOP ( 'NONE', ( #21278, #4735, #18976, #5991 ) ) ;
#24843 = B_SPLINE_CURVE_WITH_KNOTS ( 'NONE', 3,
 ( #11078, #18602, #3574, #31476, #3239, #11234, #16262, #21442, #13734, #16409, #745, #28494, #1224 ),
 .UNSPECIFIED., .F., .F.,
 ( 4, 3, 3, 3, 4 ),
 ( 0.000000000000000000, 0.0008924174835303601240, 0.001784834967102757585, 0.002677252450717581070, 0.003341508248895443296 ),
 .UNSPECIFIED. ) ;
#24844 = CARTESIAN_POINT ( 'NONE',  ( 2.680481146936424253, 8.652652323859461703, 5.199347632287054211 ) ) ;
#24845 = PERSON_AND_ORGANIZATION ( #6766, #25292 ) ;
#24846 = CARTESIAN_POINT ( 'NONE',  ( -2.700050800000000084, 2.983565686104819648, 0.3135853898029609677 ) ) ;
#24847 = ORIENTED_EDGE ( 'NONE', *, *, #3865, .T. ) ;
#24848 = FACE_OUTER_BOUND ( 'NONE', #4632, .T. ) ;
#24849 = CARTESIAN_POINT ( 'NONE',  ( 108.0281772836523544, -18.47510799158657591, -4.365046262023239976 ) ) ;
#24850 = CARTESIAN_POINT ( 'NONE',  ( 54.97722363750290953, -6.506539134337329777, -3.993434333351804977 ) ) ;
#24851 = DIRECTION ( 'NONE',  ( 0.000000000000000000, -0.8191520442889833609, -0.5735764363510580388 ) ) ;
#24852 = FACE_OUTER_BOUND ( 'NONE', #13887, .T. ) ;
#24853 = ORIENTED_EDGE ( 'NONE', *, *, #19417, .F. ) ;
#24854 = CARTESIAN_POINT ( 'NONE',  ( 23.27353278736382691, -21.94187821002792660, -1.030224486531079453 ) ) ;
#24855 = CARTESIAN_POINT ( 'NONE',  ( 22.95054569172171099, -21.90694603883951785, -1.257390168162247246 ) ) ;
#24856 = CARTESIAN_POINT ( 'NONE',  ( 0.000000000000000000, 7.347880794884119736E-16, -6.000000000000000000 ) ) ;
#24858 = EDGE_LOOP ( 'NONE', ( #18558, #33095, #11012, #4089 ) ) ;
#24857 = CARTESIAN_POINT ( 'NONE',  ( 110.6444052656891301, 21.58830278953161752, 0.4463807625372899768 ) ) ;
#24859 = CARTESIAN_POINT ( 'NONE',  ( 3.499999999999999556, 3.771202944355777298, -4.982773259188332027 ) ) ;
#24860 = EDGE_CURVE ( 'NONE', #6329, #21228, #31667, .T. ) ;
#24861 = FACE_OUTER_BOUND ( 'NONE', #13973, .T. ) ;
#24862 = CARTESIAN_POINT ( 'NONE',  ( -1.694237876702965329, -1.500727999663087564, -4.522129901861166701 ) ) ;
#24863 = CARTESIAN_POINT ( 'NONE',  ( 17.41559371906256004, 18.02474698348863669, -1.491740999229419273 ) ) ;
#24864 = CARTESIAN_POINT ( 'NONE',  ( 0.000000000000000000, -2.834406817834851378, -8.013497238472808704 ) ) ;
#24865 = B_SPLINE_CURVE_WITH_KNOTS ( 'NONE', 3,
 ( #5162, #20208, #9207, #4050, #21753, #31960, #9025, #16744, #14217, #24415 ),
 .UNSPECIFIED., .F., .F.,
 ( 4, 2, 2, 2, 4 ),
 ( 3.032460776717885298E-07, 0.0005479053915603963095, 0.001095507537043120816, 0.001643109682525845322, 0.002190711828008569829 ),
 .UNSPECIFIED. ) ;
#24866 = EDGE_CURVE ( 'NONE', #1564, #15750, #21460, .T. ) ;
#24867 = CARTESIAN_POINT ( 'NONE',  ( 5.489343555808769537, 0.1039150536218459431, 8.118190043691528857 ) ) ;
#24868 = CARTESIAN_POINT ( 'NONE',  ( 5.489321708267612898, -6.152096559282798083, -5.297846913781757650 ) ) ;
#24869 = CARTESIAN_POINT ( 'NONE',  ( -31.57659242536668742, -27.93932300454937590, -1.000000000000000000 ) ) ;
#24871 = CARTESIAN_POINT ( 'NONE',  ( 68.79832465279001497, -7.861404707920833346, 0.07017451552781736601 ) ) ;
#24870 = DESIGN_CONTEXT ( 'detailed design', #28512, 'design' ) ;
#24872 = VERTEX_POINT ( 'NONE', #11583 ) ;
#24873 = EDGE_CURVE ( 'NONE', #19567, #7768, #24144, .T. ) ;
#24874 = EDGE_CURVE ( 'NONE', #17188, #24705, #6238, .T. ) ;
#24875 = CARTESIAN_POINT ( 'NONE',  ( -2.950050802731187360, 0.3135853898029611342, -2.983565686104819648 ) ) ;
#24876 = ORIENTED_EDGE ( 'NONE', *, *, #27688, .T. ) ;
#24877 = CARTESIAN_POINT ( 'NONE',  ( -5.404531657079157725, -1.883076972206379818, -2.325406398514292761 ) ) ;
#24878 = CARTESIAN_POINT ( 'NONE',  ( -29.02642725384296440, 4.820254766716771222, 1.500000000000000000 ) ) ;
#24879 = ADVANCED_FACE ( 'NONE', ( #2410 ), #30316, .F. ) ;
#24880 = CARTESIAN_POINT ( 'NONE',  ( 102.8074457324386515, -4.091069046465105608, -5.695980980372493008 ) ) ;
#24881 = CARTESIAN_POINT ( 'NONE',  ( 25.76000000000000512, 2.749440278475487442, 1.299952413566024756 ) ) ;
#24882 = CARTESIAN_POINT ( 'NONE',  ( 2.482257818914018532, 0.000000000000000000, 1.712210361609934672 ) ) ;
#24883 = ORIENTED_EDGE ( 'NONE', *, *, #23782, .F. ) ;
#24884 = CARTESIAN_POINT ( 'NONE',  ( 107.6659035224683407, 16.31777890981063805, -1.490131869724928615 ) ) ;
#24885 = ORIENTED_EDGE ( 'NONE', *, *, #27341, .T. ) ;
#24886 = PERSON_AND_ORGANIZATION ( #6766, #25292 ) ;
#24887 = CARTESIAN_POINT ( 'NONE',  ( 18.75864038940818901, -5.875138777191356354, 3.999773682846184730 ) ) ;
#24888 = ADVANCED_FACE ( 'NONE', ( #12582 ), #7035, .T. ) ;
#24889 = CARTESIAN_POINT ( 'NONE',  ( -56.28351068137280322, -9.529120656610874963E-19, -1.066050254142973275 ) ) ;
#24891 = DIRECTION ( 'NONE',  ( 1.000000000000000000, -0.000000000000000000, -0.000000000000000000 ) ) ;
#24890 = DIRECTION ( 'NONE',  ( -1.000000000000000000, 8.574039729943018344E-17, -0.000000000000000000 ) ) ;
#24892 = ORIENTED_EDGE ( 'NONE', *, *, #31237, .F. ) ;
#24893 = CARTESIAN_POINT ( 'NONE',  ( 7.249760686538667009, 6.226446564517917892, 6.147671362329242051 ) ) ;
#24894 = CARTESIAN_POINT ( 'NONE',  ( -23.54713438637982748, 18.46223496596754288, 1.773004750130224627 ) ) ;
#24895 = CARTESIAN_POINT ( 'NONE',  ( 24.61000000136559862, 2.892927487894327410, -1.570731468192931635 ) ) ;
#24896 = CARTESIAN_POINT ( 'NONE',  ( 0.3144672950280170687, -7.550758264647147833, -1.499999999999964251 ) ) ;
#24898 = ORIENTED_EDGE ( 'NONE', *, *, #21117, .T. ) ;
#24897 = CARTESIAN_POINT ( 'NONE',  ( 3.529609406779910419, -12.17998485103522199, 1.500000000000000444 ) ) ;
#24899 = CARTESIAN_POINT ( 'NONE',  ( -7.912550801365592967, 3.675193018007247403, -1.088641768524161391 ) ) ;
#24900 = DIRECTION ( 'NONE',  ( 0.000000000000000000, 0.2079116908177532919, 0.9781476007338069101 ) ) ;
#24901 = DIRECTION ( 'NONE',  ( -0.000000000000000000, -0.000000000000000000, -1.000000000000000000 ) ) ;
#24902 = DIRECTION ( 'NONE',  ( 0.03488359650710500665, -0.9989355049964836475, -0.03018263660036204013 ) ) ;
#24903 = ORIENTED_EDGE ( 'NONE', *, *, #7824, .F. ) ;
#24905 = ORIENTED_EDGE ( 'NONE', *, *, #23486, .T. ) ;
#24904 = FACE_OUTER_BOUND ( 'NONE', #28917, .T. ) ;
#24906 = CYLINDRICAL_SURFACE ( 'NONE', #19285, 6.000000000000000888 ) ;
#24907 = LINE ( 'NONE', #19571, #31774 ) ;
#24908 = EDGE_CURVE ( 'NONE', #22300, #9606, #31536, .T. ) ;
#24909 = ADVANCED_FACE ( 'NONE', ( #7242 ), #2564, .F. ) ;
#24910 = CARTESIAN_POINT ( 'NONE',  ( -21.76268656866881557, 18.40448632064758527, 1.500000000000000222 ) ) ;
#24911 = CARTESIAN_POINT ( 'NONE',  ( 2.970200448039785002, -3.362738345035427567, -8.521880193013316784 ) ) ;
#24912 = CARTESIAN_POINT ( 'NONE',  ( -2.829285547032501125, -11.58124708880041176, -1.743702903532054371 ) ) ;
#24913 = DIRECTION ( 'NONE',  ( 0.000000000000000000, 0.000000000000000000, -1.000000000000000000 ) ) ;
#24914 = DIRECTION ( 'NONE',  ( -7.472768010110281180E-18, -0.08715574274764813223, -0.9961946980917464334 ) ) ;
#24915 = DIRECTION ( 'NONE',  ( -1.000000000000000000, 8.574039729943022041E-17, -1.232595164407830946E-32 ) ) ;
#24916 = VERTEX_POINT ( 'NONE', #25297 ) ;
#24917 = EDGE_CURVE ( 'NONE', #7166, #10028, #32496, .T. ) ;
#24918 = CARTESIAN_POINT ( 'NONE',  ( -14.63259398290947289, -21.93932300455827544, -0.9045955023117271399 ) ) ;
#24919 = ORIENTED_EDGE ( 'NONE', *, *, #7450, .F. ) ;
#24920 = FACE_OUTER_BOUND ( 'NONE', #17556, .T. ) ;
#24921 = FACE_OUTER_BOUND ( 'NONE', #18550, .T. ) ;
#24922 = ORIENTED_EDGE ( 'NONE', *, *, #24960, .F. ) ;
#24923 = EDGE_CURVE ( 'NONE', #16362, #20158, #7094, .T. ) ;
#24924 = CARTESIAN_POINT ( 'NONE',  ( 0.000000000000000000, -8.497168642645963388, -0.2193742428685781509 ) ) ;
#24925 = VERTEX_POINT ( 'NONE', #15252 ) ;
#24926 = LINE ( 'NONE', #14370, #32203 ) ;
#24928 = ORIENTED_EDGE ( 'NONE', *, *, #26372, .T. ) ;
#24927 = CARTESIAN_POINT ( 'NONE',  ( 84.96597185339788894, -4.065391592161865297, -4.003573871808557172 ) ) ;
#24929 = ORIENTED_EDGE ( 'NONE', *, *, #10601, .T. ) ;
#24930 = CARTESIAN_POINT ( 'NONE',  ( 20.86000000136559507, 0.3178988483021036315, 3.024605502323848949 ) ) ;
#24931 = B_SPLINE_CURVE_WITH_KNOTS ( 'NONE', 3,
 ( #13038, #28584, #23240, #10175, #10518, #25917, #20399, #23383, #5677, #15858, #30615, #7698 ),
 .UNSPECIFIED., .F., .F.,
 ( 4, 2, 2, 2, 2, 4 ),
 ( 3.529906531158615134E-18, 0.0002088350746644245339, 0.0004176701493288455442, 0.0008353402986576876190, 0.001670680597315359192, 0.003341361194630703205 ),
 .UNSPECIFIED. ) ;
#24932 = CARTESIAN_POINT ( 'NONE',  ( 102.5305753040692736, -0.1042037546421131222, 1.010822989962091301 ) ) ;
#24934 = ORIENTED_EDGE ( 'NONE', *, *, #2985, .F. ) ;
#24933 = CARTESIAN_POINT ( 'NONE',  ( -4.181737789223789470, -9.389646197556098528, -1.500000000000000888 ) ) ;
#24935 = CARTESIAN_POINT ( 'NONE',  ( 25.25352962647643906, 18.67320858041093956, -1.050000000000058886 ) ) ;
#24936 = CARTESIAN_POINT ( 'NONE',  ( 9.350000000000028066, 5.584097191983464876E-14, 1.000000000000000000 ) ) ;
#24937 =( BOUNDED_CURVE ( )  B_SPLINE_CURVE ( 2, ( #26511, #21494, #14268, #23973, #18639, #28837, #8601, #11608, #3763, #31705, #24151 ),
 .UNSPECIFIED., .F., .F. ) 
 B_SPLINE_CURVE_WITH_KNOTS ( ( 3, 2, 2, 2, 2, 3 ),
 ( 0.6966116191895003196, 0.6999999999999999556, 0.7249999999999999778, 0.7500000000000000000, 0.7750000000000000222, 0.7966116191895004084 ),
 .UNSPECIFIED. ) 
 CURVE ( )  GEOMETRIC_REPRESENTATION_ITEM ( )  RATIONAL_B_SPLINE_CURVE ( ( 0.9821626249036858880, 0.9896829947469992783, 1.000000000000000000, 0.9238795325112867385, 1.000000000000000000, 0.9238795325112867385, 1.000000000000000000, 0.9238795325112867385, 1.000000000000000000, 0.9341965377642874602, 0.9821626249036858880 ) ) 
 REPRESENTATION_ITEM ( '' )  );
#24938 = CARTESIAN_POINT ( 'NONE',  ( 34.98223484310469900, 0.5000000000000000000, 2.482234843104951239 ) ) ;
#24939 = LINE ( 'NONE', #2554, #8539 ) ;
#24941 = VERTEX_POINT ( 'NONE', #25456 ) ;
#24940 = CARTESIAN_POINT ( 'NONE',  ( 107.9828938048920435, -17.82303716254959980, -4.417089530202084724 ) ) ;
#24942 = CARTESIAN_POINT ( 'NONE',  ( 2.864531019710236048, -8.868883597856992651, -3.575186956654084369 ) ) ;
#24943 = CARTESIAN_POINT ( 'NONE',  ( 23.11000000273118715, 1.573300977624590313, -1.942864903642426144 ) ) ;
#24944 = CARTESIAN_POINT ( 'NONE',  ( 24.36000000136559507, 0.9349337715887185984, -3.156283516753368268 ) ) ;
#24945 = EDGE_CURVE ( 'NONE', #28748, #12752, #12731, .T. ) ;
#24946 = DIRECTION ( 'NONE',  ( 1.000000000000000000, 0.000000000000000000, 0.000000000000000000 ) ) ;
#24947 = PLANE ( 'NONE',  #5450 ) ;
#24948 = CYLINDRICAL_SURFACE ( 'NONE', #11894, 10.97000000000000064 ) ;
#24949 = VERTEX_POINT ( 'NONE', #9405 ) ;
#24950 = CARTESIAN_POINT ( 'NONE',  ( 4.749760686538667009, -7.530955069117495349, -2.741043480755002371 ) ) ;
#24951 = CARTESIAN_POINT ( 'NONE',  ( 101.6441386174529384, -1.774168274679073454, -2.184956718804114573 ) ) ;
#24952 = CARTESIAN_POINT ( 'NONE',  ( -7.737550801365593145, -1.828967928396026732, 3.368539882008728004 ) ) ;
#24953 = ORIENTED_EDGE ( 'NONE', *, *, #2198, .F. ) ;
#24954 = B_SPLINE_CURVE_WITH_KNOTS ( 'NONE', 3,
 ( #19819, #7119, #32380, #22488, #20006, #17463, #9284, #19501 ),
 .UNSPECIFIED., .F., .F.,
 ( 4, 2, 2, 4 ),
 ( 5.099451029784244903E-07, 0.001229189612673438564, 0.001843529446458668647, 0.002457869280243898946 ),
 .UNSPECIFIED. ) ;
#24955 = DIRECTION ( 'NONE',  ( 0.000000000000000000, -0.2079116908177664480, 0.9781476007338041345 ) ) ;
#24956 = CARTESIAN_POINT ( 'NONE',  ( 2.770684449829447615, 0.02953710645924999961, -1.228046178477606443 ) ) ;
#24957 = ORIENTED_EDGE ( 'NONE', *, *, #11670, .T. ) ;
#24958 = CARTESIAN_POINT ( 'NONE',  ( 108.2917183403153274, 19.80256275031683799, 2.320955343329570653 ) ) ;
#24959 = ORIENTED_EDGE ( 'NONE', *, *, #28831, .F. ) ;
#24960 = EDGE_CURVE ( 'NONE', #3463, #14136, #29814, .T. ) ;
#24961 = CC_DESIGN_PERSON_AND_ORGANIZATION_ASSIGNMENT ( #11361, #29240, ( #12467 ) ) ;
#24962 = ORIENTED_EDGE ( 'NONE', *, *, #31521, .T. ) ;
#24963 = FACE_OUTER_BOUND ( 'NONE', #10778, .T. ) ;
#24965 = VERTEX_POINT ( 'NONE', #14753 ) ;
#24964 = CARTESIAN_POINT ( 'NONE',  ( 4.749760686538667009, 6.139290821770257089, 5.151476664237498504 ) ) ;
#24966 = ORIENTED_EDGE ( 'NONE', *, *, #31283, .F. ) ;
#24967 = CARTESIAN_POINT ( 'NONE',  ( 21.11000000136559507, -3.156283516753370488, -0.9349337715887220401 ) ) ;
#24968 = ORIENTED_EDGE ( 'NONE', *, *, #28424, .T. ) ;
#24969 = DIRECTION ( 'NONE',  ( -6.062761635205554800E-17, -0.7071067811865441310, -0.7071067811865510144 ) ) ;
#24971 = VERTEX_POINT ( 'NONE', #17082 ) ;
#24970 = CARTESIAN_POINT ( 'NONE',  ( 35.33570769239872789, -4.203675997508360851, -1.873789188777423176 ) ) ;
#24972 = DIRECTION ( 'NONE',  ( -1.000000000000000000, 0.000000000000000000, 0.000000000000000000 ) ) ;
#24973 = PLANE ( 'NONE',  #11217 ) ;
#24974 = CARTESIAN_POINT ( 'NONE',  ( 20.92250000136559507, 0.3178988483021036315, 3.024605502323848949 ) ) ;
#24975 = CARTESIAN_POINT ( 'NONE',  ( 33.81874022276151237, 19.50000000000000000, -1.977928362984232802 ) ) ;
#24976 = EDGE_CURVE ( 'NONE', #30996, #16442, #27292, .T. ) ;
#24977 = EDGE_CURVE ( 'NONE', #20879, #6075, #25231, .T. ) ;
#24978 = DIRECTION ( 'NONE',  ( 1.000000000000000000, 0.000000000000000000, 0.000000000000000000 ) ) ;
#24979 = CARTESIAN_POINT ( 'NONE',  ( 10.00000000000000178, -4.971152295393308940, 0.6226916219171868550 ) ) ;
#24980 = CARTESIAN_POINT ( 'NONE',  ( -23.35000000000000142, -10.96966150227469505, 1.500000000000000000 ) ) ;
#24981 = DIRECTION ( 'NONE',  ( 5.361488761196516318E-16, -1.000000000000000000, 0.000000000000000000 ) ) ;
#24982 = CARTESIAN_POINT ( 'NONE',  ( 35.16139127360178662, -8.400504373793673096, -0.02339150517595086839 ) ) ;
#24983 = CYLINDRICAL_SURFACE ( 'NONE', #10237, 6.248999999999999666 ) ;
#24984 = CARTESIAN_POINT ( 'NONE',  ( 23.84714171513466141, -3.444070612163574463, -0.02339150518254430253 ) ) ;
#24985 = DIRECTION ( 'NONE',  ( -0.000000000000000000, 0.000000000000000000, 1.000000000000000000 ) ) ;
#24986 = CARTESIAN_POINT ( 'NONE',  ( -2.600050802731188160, 0.9222479816126443186, 3.113457007523260156 ) ) ;
#24987 = VERTEX_POINT ( 'NONE', #19772 ) ;
#24988 = CARTESIAN_POINT ( 'NONE',  ( -3.000050799999999906, -1.887961173149512062, -2.331437884370912261 ) ) ;
#24989 = CARTESIAN_POINT ( 'NONE',  ( -50.60000000000000142, -21.93932300454937945, 1.000000000000000000 ) ) ;
#24990 = CARTESIAN_POINT ( 'NONE',  ( -4.450050800000000528, 1.549418761218566143, -2.853674364686379583 ) ) ;
#24991 = ORIENTED_EDGE ( 'NONE', *, *, #23043, .T. ) ;
#24992 = FACE_OUTER_BOUND ( 'NONE', #12149, .T. ) ;
#24993 = CARTESIAN_POINT ( 'NONE',  ( 5.885541838704148709, -5.674471607902398240, -6.185046950422377066 ) ) ;
#24994 = ORIENTED_EDGE ( 'NONE', *, *, #11569, .T. ) ;
#24995 = CARTESIAN_POINT ( 'NONE',  ( 101.7539452112899170, -3.355355909486178234, -4.312047644358228737 ) ) ;
#24996 = DATE_AND_TIME ( #22833, #28015 ) ;
#24997 = FACE_OUTER_BOUND ( 'NONE', #19226, .T. ) ;
#24998 = VERTEX_POINT ( 'NONE', #22630 ) ;
#24999 = LINE ( 'NONE', #17480, #28363 ) ;
#25000 = ORIENTED_EDGE ( 'NONE', *, *, #6609, .F. ) ;
#25001 = CARTESIAN_POINT ( 'NONE',  ( -34.57258968893669504, -0.01303574654798582769, 3.062543865805540388 ) ) ;
#25002 = CARTESIAN_POINT ( 'NONE',  ( 8.924027012814292448, 0.4017312525919723987, -1.500000000000001776 ) ) ;
#25003 = FACE_OUTER_BOUND ( 'NONE', #32753, .T. ) ;
#25004 = CARTESIAN_POINT ( 'NONE',  ( -1.444447458290426890E-30, -1.659765939693074585E-14, 4.753758587302147731 ) ) ;
#25005 = ORIENTED_EDGE ( 'NONE', *, *, #21394, .F. ) ;
#25006 = ADVANCED_FACE ( 'NONE', ( #27631 ), #2223, .F. ) ;
#25007 = CARTESIAN_POINT ( 'NONE',  ( -50.81000000000000227, -10.96999999999998643, 8.549999999999998934 ) ) ;
#25008 = DIRECTION ( 'NONE',  ( 1.000000000000000000, 0.000000000000000000, 0.000000000000000000 ) ) ;
#25009 = EDGE_CURVE ( 'NONE', #1852, #17100, #22443, .T. ) ;
#25011 = VERTEX_POINT ( 'NONE', #10906 ) ;
#25010 = DIRECTION ( 'NONE',  ( 0.000000000000000000, 0.000000000000000000, 1.000000000000000000 ) ) ;
#25012 = CARTESIAN_POINT ( 'NONE',  ( 6.356382477965130562, -6.209963745178052719, 5.959271875177131861 ) ) ;
#25013 = B_SPLINE_CURVE_WITH_KNOTS ( 'NONE', 3,
 ( #21256, #11392, #18737, #18927, #13224, #23591, #26109, #16241, #3553, #3698 ),
 .UNSPECIFIED., .F., .F.,
 ( 4, 3, 3, 4 ),
 ( 0.000000000000000000, 0.0005352024010578549252, 0.001070404802115705514, 0.002130599829431759334 ),
 .UNSPECIFIED. ) ;
#25014 = SPHERICAL_SURFACE ( 'NONE', #6983, 0.4500000000000000111 ) ;
#25015 = FACE_OUTER_BOUND ( 'NONE', #8437, .T. ) ;
#25016 = DIRECTION ( 'NONE',  ( 0.1908089953765452762, 0.000000000000000000, -0.9816271834476639757 ) ) ;
#25017 = CARTESIAN_POINT ( 'NONE',  ( 6.880159790065807357, -0.8322990769132998512, 8.691376398188698005 ) ) ;
#25018 = DIRECTION ( 'NONE',  ( 0.000000000000000000, 0.000000000000000000, 1.000000000000000000 ) ) ;
#25019 = CARTESIAN_POINT ( 'NONE',  ( -56.30671226373046778, 0.08474811141987699525, -1.285380615603192611 ) ) ;
#25020 = DIRECTION ( 'NONE',  ( -7.770718973608957703E-17, -0.9063077870366483824, -0.4226182617407029940 ) ) ;
#25021 = VERTEX_POINT ( 'NONE', #8054 ) ;
#25022 = CARTESIAN_POINT ( 'NONE',  ( -7.012550801365593500, 3.368539882008727115, 1.828967928396026954 ) ) ;
#25023 = ORIENTED_EDGE ( 'NONE', *, *, #12949, .F. ) ;
#25024 = CARTESIAN_POINT ( 'NONE',  ( -8.254531657079157370, 2.846291840500173365, 1.545410377633946952 ) ) ;
#25025 = CARTESIAN_POINT ( 'NONE',  ( 25.79750000136559507, 2.363507492473148286, 1.913930629741525058 ) ) ;
#25026 = CARTESIAN_POINT ( 'NONE',  ( 41.44346753120585447, -6.883984642623638628, -5.695980980372493008 ) ) ;
#25027 = DIRECTION ( 'NONE',  ( 1.000000000000000000, 0.000000000000000000, 0.000000000000000000 ) ) ;
#25028 = DIRECTION ( 'NONE',  ( -0.000000000000000000, -0.000000000000000000, -1.000000000000000000 ) ) ;
#25029 = ORIENTED_EDGE ( 'NONE', *, *, #9536, .T. ) ;
#25030 = CARTESIAN_POINT ( 'NONE',  ( 19.01015279934141589, -3.063734813013466951, 0.8134928201657850577 ) ) ;
#25031 = EDGE_LOOP ( 'NONE', ( #27346, #19718, #26772, #1579 ) ) ;
#25032 = CARTESIAN_POINT ( 'NONE',  ( 4.749760686538667009, 6.139290821770327256, -5.151476664237414127 ) ) ;
#25033 = APPROVAL_STATUS ( 'not_yet_approved' ) ;
#25034 = CARTESIAN_POINT ( 'NONE',  ( 69.06980207411518791, -6.103400497572641470, 4.013698489646581713 ) ) ;
#25035 = EDGE_CURVE ( 'NONE', #11109, #10411, #2923, .T. ) ;
#25036 = CARTESIAN_POINT ( 'NONE',  ( -56.30880873598355407, 0.09981903777915809850, -1.306826643672643673 ) ) ;
#25038 = DIRECTION ( 'NONE',  ( -0.1027947991993878596, 0.9947025833170223263, 0.000000000000000000 ) ) ;
#25037 = FACE_OUTER_BOUND ( 'NONE', #28915, .T. ) ;
#25039 = VERTEX_POINT ( 'NONE', #28470 ) ;
#25040 = CARTESIAN_POINT ( 'NONE',  ( 10.56183597391177464, 4.888740217817763464E-14, -4.753758587302147731 ) ) ;
#25041 = DIRECTION ( 'NONE',  ( 0.4999999999999978351, 0.8660254037844398178, 0.000000000000000000 ) ) ;
#25042 = CARTESIAN_POINT ( 'NONE',  ( 23.86000000136559507, 1.570731468192929858, 2.892927487894329186 ) ) ;
#25043 = CARTESIAN_POINT ( 'NONE',  ( 9.054745842343928430, -14.53181015844465129, -1.499999999999859668 ) ) ;
#25045 = ORIENTED_EDGE ( 'NONE', *, *, #25772, .T. ) ;
#25044 = CARTESIAN_POINT ( 'NONE',  ( 108.4615897723380868, -15.55450498649102720, 0.9788672205888330202 ) ) ;
#25046 = CARTESIAN_POINT ( 'NONE',  ( -3.637550801365593944, -3.675193018007246071, 1.088641768524163167 ) ) ;
#25047 = CARTESIAN_POINT ( 'NONE',  ( 12.44989959798878587, 19.50000000000000000, 1.818740222761551451 ) ) ;
#25048 = EDGE_CURVE ( 'NONE', #22885, #24805, #7748, .T. ) ;
#25049 = CARTESIAN_POINT ( 'NONE',  ( 7.064632951172269415, -7.135485519862033499, 5.064320921489798621 ) ) ;
#25050 = DIRECTION ( 'NONE',  ( 0.000000000000000000, 0.000000000000000000, 1.000000000000000000 ) ) ;
#25051 = ORIENTED_EDGE ( 'NONE', *, *, #3348, .T. ) ;
#25053 = ORIENTED_EDGE ( 'NONE', *, *, #23066, .F. ) ;
#25052 = CARTESIAN_POINT ( 'NONE',  ( 109.7606186995332536, 16.66703046365059393, -0.4463807625373608645 ) ) ;
#25054 = CARTESIAN_POINT ( 'NONE',  ( 3.499999999999999556, 7.008469740302810891, -0.7425307242147067832 ) ) ;
#25055 = CARTESIAN_POINT ( 'NONE',  ( 107.8972572759871866, 20.45595522325154647, -2.263373122311984176 ) ) ;
#25056 = B_SPLINE_CURVE_WITH_KNOTS ( 'NONE', 3,
 ( #7317, #17507, #11836, #24522, #7169, #22047, #17362, #27702, #6665, #14678 ),
 .UNSPECIFIED., .F., .F.,
 ( 4, 2, 2, 2, 4 ),
 ( 0.000000000000000000, 0.0004294301529276467965, 0.0008588603058552935930, 0.001288290458782940335, 0.001717720611710587186 ),
 .UNSPECIFIED. ) ;
#25057 = DIRECTION ( 'NONE',  ( 0.000000000000000000, 0.9063077870366497146, -0.4226182617406998299 ) ) ;
#25058 = ADVANCED_FACE ( 'NONE', ( #20772 ), #3396, .F. ) ;
#25059 = APPLICATION_CONTEXT ( 'configuration controlled 3d designs of mechanical parts and assemblies' ) ;
#25060 = CARTESIAN_POINT ( 'NONE',  ( -19.37241134977605128, 17.09829073722516668, 1.500000000000000000 ) ) ;
#25061 = CARTESIAN_POINT ( 'NONE',  ( 69.01291188534348464, -4.970031385439517280, 3.993434827421580735 ) ) ;
#25062 = CARTESIAN_POINT ( 'NONE',  ( -1.691706751995829539, -13.40606180584711993, -1.500000000000239364 ) ) ;
#25063 = DIRECTION ( 'NONE',  ( -1.000000000000000000, -0.000000000000000000, 0.000000000000000000 ) ) ;
#25064 = EDGE_CURVE ( 'NONE', #23391, #2520, #18583, .T. ) ;
#25065 = CARTESIAN_POINT ( 'NONE',  ( 84.86779539659983129, -2.484919561749620698, 1.169950239652608914 ) ) ;
#25066 = LINE ( 'NONE', #3, #7122 ) ;
#25067 = ORIENTED_EDGE ( 'NONE', *, *, #12013, .F. ) ;
#25068 = CARTESIAN_POINT ( 'NONE',  ( 26.44001828968094259, 18.17676778675653892, -2.806473568333506474 ) ) ;
#25069 = ORIENTED_EDGE ( 'NONE', *, *, #12328, .F. ) ;
#25070 = VECTOR ( 'NONE', #31160, 1000.000000000000000 ) ;
#25071 = CIRCLE ( 'NONE', #10666, 0.4999999999999997780 ) ;
#25072 = CARTESIAN_POINT ( 'NONE',  ( -39.83999999999998920, -10.96999999999998643, 1.500000000000000000 ) ) ;
#25073 = EDGE_CURVE ( 'NONE', #12812, #10072, #8148, .T. ) ;
#25074 =( NAMED_UNIT ( * ) PLANE_ANGLE_UNIT ( ) SI_UNIT ( $, .RADIAN. ) );
#25075 = DIRECTION ( 'NONE',  ( -0.000000000000000000, -0.000000000000000000, -1.000000000000000000 ) ) ;
#25076 = VERTEX_POINT ( 'NONE', #23427 ) ;
#25077 = VECTOR ( 'NONE', #23309, 1000.000000000000114 ) ;
#25078 = CARTESIAN_POINT ( 'NONE',  ( 107.6765350359755615, 19.22395582067604991, -4.843906566570527872 ) ) ;
#25079 = EDGE_LOOP ( 'NONE', ( #12902, #7223, #27698, #12491 ) ) ;
#25080 = DIRECTION ( 'NONE',  ( -1.000000000000000000, -0.000000000000000000, -0.000000000000000000 ) ) ;
#25082 = EDGE_LOOP ( 'NONE', ( #1709, #14214, #24712, #24357 ) ) ;
#25081 = CARTESIAN_POINT ( 'NONE',  ( 102.3453678278643508, -2.874915557871456251, -4.023790184234727896 ) ) ;
#25083 = ORIENTED_EDGE ( 'NONE', *, *, #22766, .F. ) ;
#25084 = EDGE_CURVE ( 'NONE', #28105, #28295, #12407, .T. ) ;
#25085 = EDGE_CURVE ( 'NONE', #26215, #27222, #1783, .T. ) ;
#25086 = FACE_OUTER_BOUND ( 'NONE', #30000, .T. ) ;
#25087 = CARTESIAN_POINT ( 'NONE',  ( 19.08086296608604826, -2.273337061837033879, 1.915219082070892531 ) ) ;
#25089 = ORIENTED_EDGE ( 'NONE', *, *, #5006, .F. ) ;
#25088 = CARTESIAN_POINT ( 'NONE',  ( 0.5032040568826982030, 5.109302080990191897, 8.283195248915165010 ) ) ;
#25090 = CARTESIAN_POINT ( 'NONE',  ( 22.43659417803347722, 17.13630711828444575, -1.500000000000000000 ) ) ;
#25091 = CARTESIAN_POINT ( 'NONE',  ( 22.41270750065876172, 17.13964222952529681, 1.050000000000000044 ) ) ;
#25092 = CARTESIAN_POINT ( 'NONE',  ( 8.870145747188287189, 0.000000000000000000, 1.000000000000000000 ) ) ;
#25093 = CARTESIAN_POINT ( 'NONE',  ( 7.845473912039718556, -1.949903631126105097, -1.500000000000000000 ) ) ;
#25095 = VERTEX_POINT ( 'NONE', #17939 ) ;
#25094 = CARTESIAN_POINT ( 'NONE',  ( 107.5618622547647334, -18.98489936157325175, -4.518577578190647870 ) ) ;
#25096 = CARTESIAN_POINT ( 'NONE',  ( 3.063284526839887167, -8.152713396088739017, -3.174628368996162298 ) ) ;
#25097 = AXIS2_PLACEMENT_3D ( 'NONE', #14029, #13847, #31784 ) ;
#25098 = VECTOR ( 'NONE', #4597, 1000.000000000000000 ) ;
#25099 = LINE ( 'NONE', #2216, #2791 ) ;
#25100 = CARTESIAN_POINT ( 'NONE',  ( 25.29750000136559507, -0.3178988483021076838, -3.024605502323848949 ) ) ;
#25101 = CARTESIAN_POINT ( 'NONE',  ( 107.8757006204448459, 20.33592830970491150, -2.519365258488940107 ) ) ;
#25102 = EDGE_CURVE ( 'NONE', #4552, #32925, #534, .T. ) ;
#25103 = CARTESIAN_POINT ( 'NONE',  ( 34.99740252253902639, 0.5174497483512504603, -2.982117921349399570 ) ) ;
#25104 = CARTESIAN_POINT ( 'NONE',  ( 20.66542725970890260, -21.74162791314452647, -1.399019267719719295 ) ) ;
#25105 = VECTOR ( 'NONE', #15565, 1000.000000000000000 ) ;
#25106 = ORIENTED_EDGE ( 'NONE', *, *, #16487, .T. ) ;
#25107 = CARTESIAN_POINT ( 'NONE',  ( -3.529825581556942343E-16, -4.116875700062099241, 2.376879293651050329 ) ) ;
#25108 = CARTESIAN_POINT ( 'NONE',  ( 4.592425496802574958E-16, 0.000000000000000000, 3.750000000000000444 ) ) ;
#25109 = CARTESIAN_POINT ( 'NONE',  ( -7.587550801365593678, -3.521866450007987037, -0.3701630799359323931 ) ) ;
#25110 = EDGE_LOOP ( 'NONE', ( #29301, #31962, #25783, #23852 ) ) ;
#25111 = CARTESIAN_POINT ( 'NONE',  ( -50.60000000000000142, -10.96966150227468972, 1.500000000000000000 ) ) ;
#25112 = AXIS2_PLACEMENT_3D ( 'NONE', #28928, #3056, #31787 ) ;
#25113 = CARTESIAN_POINT ( 'NONE',  ( 7.249760686538667009, 8.385837730238846314E-14, -8.014274990069656823 ) ) ;
#25114 = CIRCLE ( 'NONE', #25651, 5.000000000000001776 ) ;
#25115 = CARTESIAN_POINT ( 'NONE',  ( 2.363212477606322359, -0.1552069907123501680, -1.757289734063390396 ) ) ;
#25116 = ORIENTED_EDGE ( 'NONE', *, *, #8833, .T. ) ;
#25117 = CARTESIAN_POINT ( 'NONE',  ( 9.350000000000001421, 0.000000000000000000, 1.000000000000000000 ) ) ;
#25118 = EDGE_CURVE ( 'NONE', #22307, #17664, #16702, .T. ) ;
#25119 = ORIENTED_EDGE ( 'NONE', *, *, #18951, .T. ) ;
#25120 = CIRCLE ( 'NONE', #10713, 9.713116299512234875 ) ;
#25121 = CARTESIAN_POINT ( 'NONE',  ( -40.71733131760397129, -12.43974741078717372, 5.871858320049880398 ) ) ;
#25122 = AXIS2_PLACEMENT_3D ( 'NONE', #13360, #10699, #20754 ) ;
#25123 = EDGE_LOOP ( 'NONE', ( #363, #3742, #1001, #25455 ) ) ;
#25124 = CARTESIAN_POINT ( 'NONE',  ( 107.1772993348646281, 16.40207914262226296, 1.508259000770581615 ) ) ;
#25126 = ORIENTED_EDGE ( 'NONE', *, *, #13264, .F. ) ;
#25125 = CARTESIAN_POINT ( 'NONE',  ( -2.984394142476101575, -0.2504768897242942161, 1.438806226522167497 ) ) ;
#25127 = ORIENTED_EDGE ( 'NONE', *, *, #161, .T. ) ;
#25128 = DIRECTION ( 'NONE',  ( 1.735780866781622650E-15, -0.000000000000000000, -1.000000000000000000 ) ) ;
#25129 = EDGE_CURVE ( 'NONE', #5578, #8757, #31893, .T. ) ;
#25130 = EDGE_CURVE ( 'NONE', #4070, #23722, #3591, .T. ) ;
#25131 = ORIENTED_EDGE ( 'NONE', *, *, #32787, .F. ) ;
#25133 = AXIS2_PLACEMENT_3D ( 'NONE', #27602, #1888, #32962 ) ;
#25132 = CARTESIAN_POINT ( 'NONE',  ( 10.56183597391177464, -1.750323540954535505E-14, 4.753758587302147731 ) ) ;
#25135 = ORIENTED_EDGE ( 'NONE', *, *, #9159, .T. ) ;
#25134 = CARTESIAN_POINT ( 'NONE',  ( 21.33742408005302593, -21.80181733053987614, 1.346293739633778852 ) ) ;
#25136 = DIRECTION ( 'NONE',  ( 0.000000000000000000, 0.000000000000000000, 1.000000000000000000 ) ) ;
#25137 = PLANE ( 'NONE',  #25643 ) ;
#25138 = CARTESIAN_POINT ( 'NONE',  ( 108.0285590637734430, -18.48060553035487530, 4.343942861253616172 ) ) ;
#25139 = AXIS2_PLACEMENT_3D ( 'NONE', #20152, #4111, #12760 ) ;
#25140 = CARTESIAN_POINT ( 'NONE',  ( 0.000000000000000000, 0.000000000000000000, 0.000000000000000000 ) ) ;
#25141 = CARTESIAN_POINT ( 'NONE',  ( 107.4514419172549680, -17.38041855283392678, -4.563595182958755991 ) ) ;
#25142 = CARTESIAN_POINT ( 'NONE',  ( 25.42756288599179726, -17.55292975162311464, 1.197473197312291404 ) ) ;
#25143 = AXIS2_PLACEMENT_3D ( 'NONE', #32364, #29835, #31130 ) ;
#25144 = VECTOR ( 'NONE', #18538, 1000.000000000000000 ) ;
#25146 = EDGE_CURVE ( 'NONE', #14230, #31255, #22595, .T. ) ;
#25145 = VECTOR ( 'NONE', #17700, 1000.000000000000114 ) ;
#25147 = PLANE ( 'NONE',  #25139 ) ;
#25148 = DIRECTION ( 'NONE',  ( -0.08910563629484180570, -0.9960221812693186294, 0.000000000000000000 ) ) ;
#25149 = APPROVAL ( #25033, 'UNSPECIFIED' ) ;
#25150 = CARTESIAN_POINT ( 'NONE',  ( 0.6903270996310453267, 7.668283427123773421, 4.902115053686892487 ) ) ;
#25151 = CARTESIAN_POINT ( 'NONE',  ( 0.000000000000000000, 0.000000000000000000, 0.000000000000000000 ) ) ;
#25152 = AXIS2_PLACEMENT_3D ( 'NONE', #1465, #11641, #24004 ) ;
#25153 = CARTESIAN_POINT ( 'NONE',  ( 0.000000000000000000, -5.848742439617878652, -6.167836887841045446 ) ) ;
#25154 = CARTESIAN_POINT ( 'NONE',  ( -4.100050802731187716, -1.549418761218565477, 2.853674364686380471 ) ) ;
#25155 = VERTEX_POINT ( 'NONE', #8387 ) ;
#25156 = CARTESIAN_POINT ( 'NONE',  ( -7.837550801365593678, 1.088641768524161613, 3.675193018007247403 ) ) ;
#25157 = VECTOR ( 'NONE', #2430, 1000.000000000000114 ) ;
#25158 = DIRECTION ( 'NONE',  ( 0.000000000000000000, -0.000000000000000000, 1.000000000000000000 ) ) ;
#25159 = FACE_OUTER_BOUND ( 'NONE', #3745, .T. ) ;
#25160 = ORIENTED_EDGE ( 'NONE', *, *, #5859, .T. ) ;
#25161 = CARTESIAN_POINT ( 'NONE',  ( -1.147381204815053790, 0.5174497483512505713, 7.899033294795724025 ) ) ;
#25162 =( LENGTH_UNIT ( ) NAMED_UNIT ( * ) SI_UNIT ( .MILLI., .METRE. ) );
#25163 = ADVANCED_FACE ( 'NONE', ( #5864 ), #240, .F. ) ;
#25164 = CARTESIAN_POINT ( 'NONE',  ( 108.0213121623446000, -18.37625195254145893, 5.107626725122443645 ) ) ;
#25165 = ORIENTED_EDGE ( 'NONE', *, *, #18345, .T. ) ;
#25166 = CARTESIAN_POINT ( 'NONE',  ( 8.438303502872338768, -14.31955465834176522, 1.499999999999858780 ) ) ;
#25167 = DATE_AND_TIME ( #27676, #2397 ) ;
#25168 = VECTOR ( 'NONE', #7744, 999.9999999999998863 ) ;
#25169 = DIRECTION ( 'NONE',  ( 1.000000000000000000, 0.000000000000000000, 0.000000000000000000 ) ) ;
#25170 = ORIENTED_EDGE ( 'NONE', *, *, #12628, .T. ) ;
#25171 = CARTESIAN_POINT ( 'NONE',  ( -1.427519812010940470, -14.09177734493767531, 1.500000000000000222 ) ) ;
#25172 = CIRCLE ( 'NONE', #15021, 0.5000000000000000000 ) ;
#25173 = AXIS2_PLACEMENT_3D ( 'NONE', #7268, #15281, #9432 ) ;
#25174 = VERTEX_POINT ( 'NONE', #23915 ) ;
#25175 = CARTESIAN_POINT ( 'NONE',  ( 108.1300413742128228, -19.95926608421463300, 1.392287898181946426 ) ) ;
#25176 = CARTESIAN_POINT ( 'NONE',  ( 54.97374409962333175, -6.380816387357196362, -4.155404937707912971 ) ) ;
#25177 = CIRCLE ( 'NONE', #10764, 10.94895958125474245 ) ;
#25178 = CARTESIAN_POINT ( 'NONE',  ( 24.37505892579753208, -17.33881490880284204, -1.312584468236271062 ) ) ;
#25179 = FACE_OUTER_BOUND ( 'NONE', #25944, .T. ) ;
#25180 = CIRCLE ( 'NONE', #14469, 10.94895958125474245 ) ;
#25181 = CARTESIAN_POINT ( 'NONE',  ( 21.51848342574702500, -21.75572564449080559, -1.472637297274180357 ) ) ;
#25182 = LINE ( 'NONE', #24856, #16694 ) ;
#25183 = AXIS2_PLACEMENT_3D ( 'NONE', #18590, #5874, #16061 ) ;
#25184 = AXIS2_PLACEMENT_3D ( 'NONE', #14838, #22224, #2345 ) ;
#25185 = VERTEX_POINT ( 'NONE', #29266 ) ;
#25186 = CARTESIAN_POINT ( 'NONE',  ( 2.632061376486628301, -0.4999999999999981681, 1.949999999999999956 ) ) ;
#25187 = FACE_OUTER_BOUND ( 'NONE', #14422, .T. ) ;
#25188 = CARTESIAN_POINT ( 'NONE',  ( -33.81874022276151237, 19.50000000000000000, 1.977928362984241017 ) ) ;
#25189 = CARTESIAN_POINT ( 'NONE',  ( 101.6702787251852698, -2.150579323183733571, -2.790733426243898752 ) ) ;
#25190 = EDGE_CURVE ( 'NONE', #22098, #15174, #7651, .T. ) ;
#25191 = CARTESIAN_POINT ( 'NONE',  ( 7.064423600674403225, -0.8180878109953999555, 8.711672189282626988 ) ) ;
#25192 = CARTESIAN_POINT ( 'NONE',  ( 10.00000000000000000, -3.055657119358826446, 3.641590349731918863 ) ) ;
#25194 = CARTESIAN_POINT ( 'NONE',  ( 22.95054569172093650, -21.90694603883944325, 1.257390168162776378 ) ) ;
#25193 = UNCERTAINTY_MEASURE_WITH_UNIT (LENGTH_MEASURE( 1.000000000000000082E-05 ), #24765, 'distance_accuracy_value', 'NONE');
#25195 = ORIENTED_EDGE ( 'NONE', *, *, #22518, .F. ) ;
#25196 = B_SPLINE_CURVE_WITH_KNOTS ( 'NONE', 3,
 ( #20770, #18252, #25961, #23119, #3070, #238 ),
 .UNSPECIFIED., .F., .F.,
 ( 4, 2, 4 ),
 ( 0.009531916414649947711, 0.5047659582073249496, 1.000000000000000000 ),
 .UNSPECIFIED. ) ;
#25197 = AXIS2_PLACEMENT_3D ( 'NONE', #11255, #19114, #3259 ) ;
#25198 = CARTESIAN_POINT ( 'NONE',  ( -6.612550801365593145, -3.368539882008727115, -1.828967928396028064 ) ) ;
#25199 = VERTEX_POINT ( 'NONE', #29619 ) ;
#25200 = AXIS2_PLACEMENT_3D ( 'NONE', #15792, #15625, #6092 ) ;
#25201 = VECTOR ( 'NONE', #5479, 1000.000000000000227 ) ;
#25202 = CARTESIAN_POINT ( 'NONE',  ( -6.554531657079158080, 0.9198621039125853827, 3.105402419394639235 ) ) ;
#25203 =( BOUNDED_CURVE ( )  B_SPLINE_CURVE ( 2, ( #12838, #30271, #18043, #22740, #12685, #32604, #2014, #5179, #7343, #28232, #9677 ),
 .UNSPECIFIED., .F., .F. ) 
 B_SPLINE_CURVE_WITH_KNOTS ( ( 3, 2, 2, 2, 2, 3 ),
 ( 0.7966116191895004084, 0.8000000000000000444, 0.8249999999999999556, 0.8499999999999999778, 0.8750000000000000000, 0.8966116191895003862 ),
 .UNSPECIFIED. ) 
 CURVE ( )  GEOMETRIC_REPRESENTATION_ITEM ( )  RATIONAL_B_SPLINE_CURVE ( ( 0.9821626249036858880, 0.9896829947469992783, 1.000000000000000000, 0.9238795325112867385, 1.000000000000000000, 0.9238795325112867385, 1.000000000000000000, 0.9238795325112867385, 1.000000000000000000, 0.9341965377642874602, 0.9821626249036858880 ) ) 
 REPRESENTATION_ITEM ( '' )  );
#25204 = CARTESIAN_POINT ( 'NONE',  ( 25.67250000136559507, 3.024605502323846729, -0.3178988483021056854 ) ) ;
#25205 = AXIS2_PLACEMENT_3D ( 'NONE', #22235, #7194, #4680 ) ;
#25206 = CARTESIAN_POINT ( 'NONE',  ( 108.1300413742128228, -19.95926608421463300, 1.392287898181946426 ) ) ;
#25207 = CARTESIAN_POINT ( 'NONE',  ( 2.542833796814050640, -3.270102266984055818E-17, -1.603032409779283407 ) ) ;
#25208 = CARTESIAN_POINT ( 'NONE',  ( 3.249999999999999556, 8.152713396088806519, -3.174628368995990879 ) ) ;
#25209 = AXIS2_PLACEMENT_3D ( 'NONE', #22099, #14719, #32621 ) ;
#25210 = VERTEX_POINT ( 'NONE', #26938 ) ;
#25211 = EDGE_CURVE ( 'NONE', #22521, #14763, #31692, .T. ) ;
#25212 = CARTESIAN_POINT ( 'NONE',  ( 0.7082655507077595392, -8.722704248566902407, 2.275631959094134515 ) ) ;
#25213 = EDGE_CURVE ( 'NONE', #7687, #7219, #30303, .T. ) ;
#25214 = VECTOR ( 'NONE', #12430, 1000.000000000000000 ) ;
#25215 = VERTEX_POINT ( 'NONE', #26599 ) ;
#25216 = CARTESIAN_POINT ( 'NONE',  ( -3.400050800000000262, 1.887961173149511618, 2.331437884370912705 ) ) ;
#25217 = ADVANCED_FACE ( 'NONE', ( #4040 ), #13863, .T. ) ;
#25218 = COORDINATED_UNIVERSAL_TIME_OFFSET ( 0, 0, .AHEAD. ) ;
#25219 = CARTESIAN_POINT ( 'NONE',  ( 54.97715759724685824, -6.504152965876262016, 3.997238534709005364 ) ) ;
#25220 = CARTESIAN_POINT ( 'NONE',  ( 1.624999999999999778, 1.464956435139694646, -10.90201369670497122 ) ) ;
#25221 = VECTOR ( 'NONE', #32412, 1000.000000000000114 ) ;
#25223 = CARTESIAN_POINT ( 'NONE',  ( 3.499999999999999556, -7.673322273190700926, -3.656518192455154193 ) ) ;
#25222 = DIRECTION ( 'NONE',  ( -0.000000000000000000, 0.9961946980917455452, -0.08715574274765797158 ) ) ;
#25224 = TOROIDAL_SURFACE ( 'NONE', #7613, 298.6457063863958865, 5.000000000000000888 ) ;
#25225 = VERTEX_POINT ( 'NONE', #21593 ) ;
#25226 = CIRCLE ( 'NONE', #28947, 5.010000000000000675 ) ;
#25227 = CARTESIAN_POINT ( 'NONE',  ( 10.00000000000000000, -3.055657119358825557, 3.641590349731918863 ) ) ;
#25228 = CARTESIAN_POINT ( 'NONE',  ( 21.75111450864415730, -1.283275288181523244E-15, -2.499999999999998668 ) ) ;
#25229 = AXIS2_PLACEMENT_3D ( 'NONE', #6236, #19111, #6887 ) ;
#25230 = CARTESIAN_POINT ( 'NONE',  ( 21.29750000000000654, -0.7685399846772070775, 2.594547506269381465 ) ) ;
#25231 = CIRCLE ( 'NONE', #9204, 0.4999999999999996669 ) ;
#25232 = CARTESIAN_POINT ( 'NONE',  ( 18.46868857681155163, -16.82956153233909546, -1.753327331145430934 ) ) ;
#25234 = ORIENTED_EDGE ( 'NONE', *, *, #4230, .T. ) ;
#25233 = CARTESIAN_POINT ( 'NONE',  ( 6.220890055307039646, -15.20372210278347680, 4.522129901861157819 ) ) ;
#25235 = CARTESIAN_POINT ( 'NONE',  ( -4.237550801365593145, -1.088641768524163389, -3.675193018007246071 ) ) ;
#25236 = CYLINDRICAL_SURFACE ( 'NONE', #6976, 4.000000000000001776 ) ;
#25237 = AXIS2_PLACEMENT_3D ( 'NONE', #30812, #10889, #30956 ) ;
#25238 = CARTESIAN_POINT ( 'NONE',  ( 7.249760686538667009, 6.139290821770257089, 5.151476664237498504 ) ) ;
#25239 = DIRECTION ( 'NONE',  ( 0.000000000000000000, 1.000000000000000000, 0.000000000000000000 ) ) ;
#25240 = AXIS2_PLACEMENT_3D ( 'NONE', #13308, #13485, #10647 ) ;
#25241 = ORIENTED_EDGE ( 'NONE', *, *, #8931, .T. ) ;
#25243 = ORIENTED_EDGE ( 'NONE', *, *, #8383, .T. ) ;
#25242 = CARTESIAN_POINT ( 'NONE',  ( 21.60307794872815279, -17.26039173292174311, 1.753143643191834355 ) ) ;
#25244 = AXIS2_PLACEMENT_3D ( 'NONE', #30945, #209, #10691 ) ;
#25245 = CARTESIAN_POINT ( 'NONE',  ( 21.16269079926919972, 16.85597784695825752, 1.500000000000000222 ) ) ;
#25246 = LINE ( 'NONE', #345, #32031 ) ;
#25247 = CARTESIAN_POINT ( 'NONE',  ( 23.29750000136559862, -2.363507492473152283, -1.913930629741525280 ) ) ;
#25248 = CARTESIAN_POINT ( 'NONE',  ( 28.71260074196063528, -4.863490077431325886, 2.787782631230470543 ) ) ;
#25249 = CARTESIAN_POINT ( 'NONE',  ( -0.3078811530705855004, -15.09896951176102498, -1.499999999999999556 ) ) ;
#25250 = EDGE_CURVE ( 'NONE', #27372, #28120, #6047, .T. ) ;
#25251 = AXIS2_PLACEMENT_3D ( 'NONE', #27370, #17159, #19849 ) ;
#25252 = CARTESIAN_POINT ( 'NONE',  ( 1.668773398854356759E-16, 1.946309384392655106, -4.616489984850511874 ) ) ;
#25253 = PRODUCT ( 'MAS-163', 'MAS-163', '', ( #27937 ) ) ;
#25254 = VECTOR ( 'NONE', #25299, 999.9999999999998863 ) ;
#25255 = AXIS2_PLACEMENT_3D ( 'NONE', #28589, #667, #3661 ) ;
#25256 = DIRECTION ( 'NONE',  ( 1.000000000000000000, -0.000000000000000000, -0.000000000000000000 ) ) ;
#25257 = DIRECTION ( 'NONE',  ( 0.000000000000000000, 0.000000000000000000, -1.000000000000000000 ) ) ;
#25258 = ORIENTED_EDGE ( 'NONE', *, *, #11475, .F. ) ;
#25259 = DIRECTION ( 'NONE',  ( 8.574039729943018344E-17, 1.000000000000000000, 0.000000000000000000 ) ) ;
#25260 = AXIS2_PLACEMENT_3D ( 'NONE', #23914, #13862, #11883 ) ;
#25261 = COORDINATED_UNIVERSAL_TIME_OFFSET ( 0, 0, .AHEAD. ) ;
#25263 = DIRECTION ( 'NONE',  ( -1.000000000000000000, 0.000000000000000000, 0.000000000000000000 ) ) ;
#25262 = AXIS2_PLACEMENT_3D ( 'NONE', #17406, #27601, #18973 ) ;
#25264 = EDGE_LOOP ( 'NONE', ( #3856, #19974 ) ) ;
#25265 = CARTESIAN_POINT ( 'NONE',  ( 108.0492715581498118, 18.45252340228810795, -4.624728054639414943 ) ) ;
#25266 = ORIENTED_EDGE ( 'NONE', *, *, #12254, .F. ) ;
#25267 = CARTESIAN_POINT ( 'NONE',  ( -17.73806761126738607, 14.75113368127120772, 1.863483178821739417 ) ) ;
#25269 = ORIENTED_EDGE ( 'NONE', *, *, #5186, .T. ) ;
#25268 = CARTESIAN_POINT ( 'NONE',  ( 54.94560668507518386, -5.364169883902320635, -4.001040679979973369 ) ) ;
#25270 = EDGE_LOOP ( 'NONE', ( #19100, #28792, #21844 ) ) ;
#25271 = CARTESIAN_POINT ( 'NONE',  ( -2.962992063741595405, -11.77309494928644185, 1.500000000000000000 ) ) ;
#25272 = CARTESIAN_POINT ( 'NONE',  ( -7.812550801365593323, 3.368539882008727115, 1.828967928396027176 ) ) ;
#25273 = DIRECTION ( 'NONE',  ( 0.000000000000000000, 0.000000000000000000, 1.000000000000000000 ) ) ;
#25274 = CARTESIAN_POINT ( 'NONE',  ( 69.13057415542958495, -2.987362752442198843, 2.713652344655541615 ) ) ;
#25276 = ORIENTED_EDGE ( 'NONE', *, *, #10611, .T. ) ;
#25275 = CARTESIAN_POINT ( 'NONE',  ( 107.6996442589674103, 19.35565155597529596, 4.629213727441584325 ) ) ;
#25277 = CARTESIAN_POINT ( 'NONE',  ( 25.73836023340068380, 18.89938647776750003, -1.050000000000000044 ) ) ;
#25278 = CARTESIAN_POINT ( 'NONE',  ( -1.170068671574867158, -6.059534462705557623, 4.522129901861156931 ) ) ;
#25279 = AXIS2_PLACEMENT_3D ( 'NONE', #3632, #25891, #3309 ) ;
#25280 = CARTESIAN_POINT ( 'NONE',  ( 6.357667873252799140, -3.476490553296904373, 7.873899671211479045 ) ) ;
#25281 = VECTOR ( 'NONE', #23846, 1000.000000000000000 ) ;
#25282 = CARTESIAN_POINT ( 'NONE',  ( -4.262285728429958207E-16, -4.971152295393298282, -0.6226916219172566880 ) ) ;
#25283 = EDGE_CURVE ( 'NONE', #21466, #21064, #3872, .T. ) ;
#25285 = EDGE_LOOP ( 'NONE', ( #16489, #9357, #17435, #6724 ) ) ;
#25284 = CARTESIAN_POINT ( 'NONE',  ( 18.65791233782715963, -7.001076235476726417, -2.184956778830003277 ) ) ;
#25286 = CARTESIAN_POINT ( 'NONE',  ( 5.377543748152551650, -7.892520144992426268, -1.391664247347309535 ) ) ;
#25287 = AXIS2_PLACEMENT_3D ( 'NONE', #6354, #27089, #6534 ) ;
#25288 = AXIS2_PLACEMENT_3D ( 'NONE', #20882, #18879, #29078 ) ;
#25289 = EDGE_CURVE ( 'NONE', #19049, #19482, #24256, .T. ) ;
#25290 = DIRECTION ( 'NONE',  ( -0.4999999999999981126, -0.8660254037844395958, 0.000000000000000000 ) ) ;
#25291 = CARTESIAN_POINT ( 'NONE',  ( 24.61000000136559862, 3.156283516753366047, 0.9349337715887203748 ) ) ;
#25292 = ORGANIZATION ( 'UNSPECIFIED', 'UNSPECIFIED', '' ) ;
#25293 = PLANE ( 'NONE',  #23625 ) ;
#25294 = CARTESIAN_POINT ( 'NONE',  ( 18.75828436641558028, -5.879118399717574661, -3.993434336035625254 ) ) ;
#25295 = CYLINDRICAL_SURFACE ( 'NONE', #18843, 0.5000000000000004441 ) ;
#25296 = ORIENTED_EDGE ( 'NONE', *, *, #32790, .T. ) ;
#25297 = CARTESIAN_POINT ( 'NONE',  ( 0.000000000000000000, -1.179494851233859887, -6.136676046192499179 ) ) ;
#25298 = EDGE_CURVE ( 'NONE', #12740, #32977, #2315, .T. ) ;
#25299 = DIRECTION ( 'NONE',  ( 0.7071067811865467956, 0.000000000000000000, 0.7071067811865483499 ) ) ;
#25300 = EDGE_CURVE ( 'NONE', #18479, #18222, #18317, .T. ) ;
#25301 = CARTESIAN_POINT ( 'NONE',  ( -7.087550801365593678, 2.228590825266444142, 2.752080473201636845 ) ) ;
#25302 = VERTEX_POINT ( 'NONE', #16243 ) ;
#25303 = AXIS2_PLACEMENT_3D ( 'NONE', #29376, #19687, #4304 ) ;
#25304 = TOROIDAL_SURFACE ( 'NONE', #28510, 9.269952810656748809, 0.4500000000000000111 ) ;
#25305 = CARTESIAN_POINT ( 'NONE',  ( 3.499999999999999556, 0.000000000000000000, 0.000000000000000000 ) ) ;
#25306 = DIRECTION ( 'NONE',  ( -1.000000000000000000, 0.000000000000000000, 0.000000000000000000 ) ) ;
#25307 = CARTESIAN_POINT ( 'NONE',  ( 17.36028307726380504, -18.11957666779667875, -4.522129901861164925 ) ) ;
#25309 = VERTEX_POINT ( 'NONE', #1373 ) ;
#25308 = AXIS2_PLACEMENT_3D ( 'NONE', #27481, #5233, #14758 ) ;
#25310 = CARTESIAN_POINT ( 'NONE',  ( 108.0120102303167613, 18.24503762629559489, -4.459921598894291961 ) ) ;
#25311 = EDGE_CURVE ( 'NONE', #2976, #10505, #32120, .T. ) ;
#25312 = ORIENTED_EDGE ( 'NONE', *, *, #20020, .T. ) ;
#25313 = DIRECTION ( 'NONE',  ( 0.000000000000000000, -0.2588190451025252914, 0.9659258262890669799 ) ) ;
#25314 = ORIENTED_EDGE ( 'NONE', *, *, #30826, .F. ) ;
#25315 = DIRECTION ( 'NONE',  ( -0.000000000000000000, -0.000000000000000000, -1.000000000000000000 ) ) ;
#25317 = VERTEX_POINT ( 'NONE', #11210 ) ;
#25316 = DIRECTION ( 'NONE',  ( 0.000000000000000000, 1.224646799147353207E-16, 1.000000000000000000 ) ) ;
#25318 = ORIENTED_EDGE ( 'NONE', *, *, #25949, .T. ) ;
#25319 = CARTESIAN_POINT ( 'NONE',  ( 5.612718761614564400, -4.279483796478976920, -7.013540705848223311 ) ) ;
#25320 = APPROVAL_PERSON_ORGANIZATION ( #27174, #28639, #27025 ) ;
#25321 = EDGE_CURVE ( 'NONE', #24925, #19839, #13502, .T. ) ;
#25322 = EDGE_LOOP ( 'NONE', ( #17603, #1759, #3512, #8369, #21124, #24919, #2645, #26688, #26022, #20603 ) ) ;
#25323 = DIRECTION ( 'NONE',  ( 0.9896144216807899463, -0.000000000000000000, 0.1437473352845038410 ) ) ;
#25325 = EDGE_LOOP ( 'NONE', ( #4090, #28670, #27570, #13692 ) ) ;
#25324 = CARTESIAN_POINT ( 'NONE',  ( 3.499999999999999556, -4.724769925181146135, -4.089810527897805414 ) ) ;
#25326 = CARTESIAN_POINT ( 'NONE',  ( 2.602069235114819801, -11.36561507724872833, -1.760364443161137826 ) ) ;
#25327 = CARTESIAN_POINT ( 'NONE',  ( 3.249999999999999556, -9.241976615262146311, -1.699438267350472209 ) ) ;
#25328 = CARTESIAN_POINT ( 'NONE',  ( 10.57125986779756843, 4.681538312723528605, -0.8254815157534771686 ) ) ;
#25329 = AXIS2_PLACEMENT_3D ( 'NONE', #5610, #10596, #20800 ) ;
#25330 = CARTESIAN_POINT ( 'NONE',  ( -29.24402871571406237, -27.93932300454937590, 11.00000000000000000 ) ) ;
#25331 = CARTESIAN_POINT ( 'NONE',  ( 0.04285674552576868024, -9.518400180040705649, 5.235784774550934273 ) ) ;
#25332 = CARTESIAN_POINT ( 'NONE',  ( 25.38393466668192744, -17.54878733605304220, 1.232996826557162251 ) ) ;
#25333 = CARTESIAN_POINT ( 'NONE',  ( 3.568565220189130027, -17.77020640688392916, 0.9788672205877712029 ) ) ;
#25334 = DIRECTION ( 'NONE',  ( -1.000000000000000000, 8.574039729943018344E-17, -0.000000000000000000 ) ) ;
#25335 = DIRECTION ( 'NONE',  ( 0.000000000000000000, 1.224646799147353207E-16, 1.000000000000000000 ) ) ;
#25336 = CARTESIAN_POINT ( 'NONE',  ( 35.23476908784418526, -3.791088091780328906, 0.02339150516272998567 ) ) ;
#25337 = EDGE_CURVE ( 'NONE', #24271, #10493, #20481, .T. ) ;
#25338 = LOCAL_TIME ( 16, 7, 10.00000000000000000, #16117 ) ;
#25339 = CARTESIAN_POINT ( 'NONE',  ( 69.32965659118902124, -6.955028994473984483, 4.522129901861163148 ) ) ;
#25340 = EDGE_CURVE ( 'NONE', #9839, #14852, #9017, .T. ) ;
#25341 = CARTESIAN_POINT ( 'NONE',  ( -4.300050802731186117, 2.853674364686379583, 1.549418761218565921 ) ) ;
#25342 = ORIENTED_EDGE ( 'NONE', *, *, #9393, .F. ) ;
#25343 = CARTESIAN_POINT ( 'NONE',  ( -4.937550801365593323, 1.828967928396027176, -3.368539882008727115 ) ) ;
#25344 = CARTESIAN_POINT ( 'NONE',  ( -33.81874022276151237, 19.50000000000000000, 13.00000000000004441 ) ) ;
#25345 = LINE ( 'NONE', #4465, #9231 ) ;
#25346 = ORIENTED_EDGE ( 'NONE', *, *, #25657, .F. ) ;
#25347 = LINE ( 'NONE', #28330, #17044 ) ;
#25348 = CARTESIAN_POINT ( 'NONE',  ( 2.357330058169020415, 7.915524238820739633, 7.401770933800242425 ) ) ;
#25349 = EDGE_CURVE ( 'NONE', #30676, #23697, #5191, .T. ) ;
#25350 = VECTOR ( 'NONE', #1910, 1000.000000000000000 ) ;
#25351 = ORIENTED_EDGE ( 'NONE', *, *, #32513, .F. ) ;
#25352 = LINE ( 'NONE', #2460, #28934 ) ;
#25353 = PERSON_AND_ORGANIZATION ( #6766, #25292 ) ;
#25355 = ORIENTED_EDGE ( 'NONE', *, *, #25035, .T. ) ;
#25354 = CARTESIAN_POINT ( 'NONE',  ( 23.58234648083524121, -8.048792613698569909, 0.07017451552781736601 ) ) ;
#25356 = VERTEX_POINT ( 'NONE', #6204 ) ;
#25357 = CARTESIAN_POINT ( 'NONE',  ( -1.487372016167590738, -13.44698662728717764, 1.744337752715020340 ) ) ;
#25358 = EDGE_CURVE ( 'NONE', #5275, #31435, #9696, .T. ) ;
#25359 = ORIENTED_EDGE ( 'NONE', *, *, #17871, .T. ) ;
#25360 = CC_DESIGN_PERSON_AND_ORGANIZATION_ASSIGNMENT ( #25353, #9612, ( #1824 ) ) ;
#25361 = CARTESIAN_POINT ( 'NONE',  ( 24.89403984153603488, 18.93045399291958475, -1.497243178805399921 ) ) ;
#25363 = ORIENTED_EDGE ( 'NONE', *, *, #24801, .T. ) ;
#25362 = CARTESIAN_POINT ( 'NONE',  ( -2.476225935960405966, -0.3178988483021057410, 3.024605502323848949 ) ) ;
#25364 = DIRECTION ( 'NONE',  ( -4.917867153433105649E-17, -0.5735764363510581498, 0.8191520442889834719 ) ) ;
#25365 = DIRECTION ( 'NONE',  ( 0.4999999999999981126, 0.8660254037844395958, -0.000000000000000000 ) ) ;
#25366 = CARTESIAN_POINT ( 'NONE',  ( 21.36297440260807790, -21.76512774916147208, -1.415548493914890793 ) ) ;
#25367 = CARTESIAN_POINT ( 'NONE',  ( 3.063284526839887167, 0.000000000000000000, 0.000000000000000000 ) ) ;
#25368 = ORIENTED_EDGE ( 'NONE', *, *, #32657, .T. ) ;
#25369 = CARTESIAN_POINT ( 'NONE',  ( 21.11000000273118715, 1.573300977624590313, -1.942864903642426144 ) ) ;
#25370 = CARTESIAN_POINT ( 'NONE',  ( 18.68265047573912341, -6.724553502642427461, 4.522129901861162260 ) ) ;
#25371 = CARTESIAN_POINT ( 'NONE',  ( 56.97280603064898941, -277.2763395528616002, -1.491740999229417941 ) ) ;
#25372 = DIRECTION ( 'NONE',  ( -1.000000000000000000, 0.000000000000000000, 0.000000000000000000 ) ) ;
#25373 = CARTESIAN_POINT ( 'NONE',  ( 24.39840143146020068, -17.41297703074901193, 1.421218545007173040 ) ) ;
#25374 = LINE ( 'NONE', #25192, #2259 ) ;
#25375 = CARTESIAN_POINT ( 'NONE',  ( -56.60872035989488893, 0.09018158751379945492, -1.329259193462423827 ) ) ;
#25376 = CARTESIAN_POINT ( 'NONE',  ( 23.27353278736381981, -21.94187821002792660, 1.000000000000000000 ) ) ;
#25377 = ORIENTED_EDGE ( 'NONE', *, *, #17033, .F. ) ;
#25378 = EDGE_CURVE ( 'NONE', #13143, #6245, #30101, .T. ) ;
#25379 = CARTESIAN_POINT ( 'NONE',  ( -6.862550801365594033, -0.3701630799359326152, 3.521866450007987037 ) ) ;
#25380 = ORIENTED_EDGE ( 'NONE', *, *, #25903, .T. ) ;
#25381 = CARTESIAN_POINT ( 'NONE',  ( -7.654531657079158613, 1.545410377633947174, -2.846291840500173365 ) ) ;
#25382 = CARTESIAN_POINT ( 'NONE',  ( 22.17250000136559507, -3.024605502323851169, 0.3178988483021052969 ) ) ;
#25383 = CARTESIAN_POINT ( 'NONE',  ( 108.0255836577191246, 18.32061982589471327, 5.125284668028994517 ) ) ;
#25384 = CARTESIAN_POINT ( 'NONE',  ( 19.72181367955163012, -17.01552588882587713, 1.753252306182963238 ) ) ;
#25385 = CARTESIAN_POINT ( 'NONE',  ( -23.54713438637982748, 8.763231220430828472, 1.786631099142472534 ) ) ;
#25386 = ORIENTED_EDGE ( 'NONE', *, *, #15588, .T. ) ;
#25387 = CARTESIAN_POINT ( 'NONE',  ( 18.96091535642496240, -3.614110606601101949, 2.184956778829998836 ) ) ;
#25388 = CARTESIAN_POINT ( 'NONE',  ( 69.18703749905368738, -4.112663945013685485, -4.522129901861162260 ) ) ;
#25389 = ORIENTED_EDGE ( 'NONE', *, *, #10839, .F. ) ;
#25390 = LINE ( 'NONE', #11556, #26779 ) ;
#25391 = APPROVAL_STATUS ( 'not_yet_approved' ) ;
#25392 = CARTESIAN_POINT ( 'NONE',  ( 28.66601932953619425, -6.689973454712867529, 4.093303788750745298 ) ) ;
#25393 = EDGE_CURVE ( 'NONE', #31349, #25757, #18337, .T. ) ;
#25394 = CARTESIAN_POINT ( 'NONE',  ( 0.7632845268398871230, 6.772677083992467928, -5.538577986808824960 ) ) ;
#25396 = CARTESIAN_POINT ( 'NONE',  ( 6.524594682510450383, -0.6222547417165948946, -8.636529731786351860 ) ) ;
#25395 = FACE_OUTER_BOUND ( 'NONE', #29661, .T. ) ;
#25397 = ORIENTED_EDGE ( 'NONE', *, *, #31821, .T. ) ;
#25398 = CARTESIAN_POINT ( 'NONE',  ( 0.1574692247322762029, -1.187839595764517142, -10.55579611470083634 ) ) ;
#25399 = CARTESIAN_POINT ( 'NONE',  ( 7.249760686538667009, 4.007137495034909236, -6.940565734314555257 ) ) ;
#25400 = CARTESIAN_POINT ( 'NONE',  ( 22.86000000136559507, 1.570731468192929858, 2.892927487894329186 ) ) ;
#25401 = CARTESIAN_POINT ( 'NONE',  ( 102.8580990270160385, -4.820463887425400884, -4.522129901861164036 ) ) ;
#25403 = ORIENTED_EDGE ( 'NONE', *, *, #29041, .T. ) ;
#25402 = CARTESIAN_POINT ( 'NONE',  ( -0.3880080537174173672, -2.647099810594272906, 4.522129901861157819 ) ) ;
#25404 = CARTESIAN_POINT ( 'NONE',  ( -7.062550801365593323, 3.521866450007987037, 0.3701630799359328372 ) ) ;
#25405 = CARTESIAN_POINT ( 'NONE',  ( 107.9842833020718444, 18.09064314930442308, -4.129529848691289473 ) ) ;
#25406 = CARTESIAN_POINT ( 'NONE',  ( -23.35000000000000142, -10.96966150227469505, -11.09540449768827308 ) ) ;
#25407 = CARTESIAN_POINT ( 'NONE',  ( -4.187842409712531875E-16, -4.884328206559829688, -1.115095498423360310 ) ) ;
#25408 = ORIENTED_EDGE ( 'NONE', *, *, #28300, .T. ) ;
#25410 = ORIENTED_EDGE ( 'NONE', *, *, #10902, .T. ) ;
#25409 = CARTESIAN_POINT ( 'NONE',  ( 24.34295195636289222, -17.38504247894183408, 1.375705049360312460 ) ) ;
#25411 = ADVANCED_FACE ( 'NONE', ( #19576 ), #17272, .F. ) ;
#25412 =( BOUNDED_SURFACE ( )  B_SPLINE_SURFACE ( 3, 2, ( 
 ( #23358, #20706, #5158 ),
 ( #13005, #10492, #3310 ),
 ( #26045, #28560, #31063 ),
 ( #25705, #15835, #8154 ),
 ( #5655, #28209, #2832 ),
 ( #28376, #5801, #20853 ),
 ( #23025, #5493, #7977 ),
 ( #18171, #5311, #3005 ),
 ( #18361, #147, #10333 ),
 ( #3147, #31245, #15490 ),
 ( #8318, #13306, #15333 ),
 ( #23514, #23696, #626 ),
 ( #13158, #2644, #466 ),
 ( #10821, #23216, #25892 ),
 ( #20548, #13482, #10645 ),
 ( #30756, #21036, #18515 ),
 ( #15683, #28708, #15979 ),
 ( #26202, #320, #814 ),
 ( #10991, #21192, #31390 ),
 ( #30906, #8465, #18662 ),
 ( #25538, #12811, #7829 ),
 ( #18022, #26853, #29539 ),
 ( #6140, #5961, #11480 ),
 ( #16468, #11792, #21996 ),
 ( #6437, #31730, #13790 ),
 ( #1452, #29050, #24340 ),
 ( #19156, #21674, #16324 ),
 ( #24483, #3970, #32224 ),
 ( #9290, #18849, #26532 ),
 ( #11310, #28861, #3633 ),
 ( #1115, #27018, #23994 ),
 ( #21518, #16641, #14288 ),
 ( #8806, #4121, #16159 ),
 ( #24176, #6626, #19010 ),
 ( #13956, #26387, #3489 ),
 ( #11629, #8628, #1603 ),
 ( #13645, #31544, #31881 ),
 ( #23849, #14140, #958 ) ),
 .UNSPECIFIED., .F., .F., .F. ) 
 B_SPLINE_SURFACE_WITH_KNOTS ( ( 4, 2, 2, 2, 2, 2, 2, 2, 2, 2, 2, 2, 2, 2, 2, 2, 2, 2, 4 ),
 ( 3, 3 ),
 ( 0.01025725344258522978, 0.01409333659602417070, 0.01792941974946311162, 0.02176550290290205428, 0.02368354447962152387, 0.02560158605634099693, 0.02656060684470073346, 0.02751962763306047000, 0.02847864842142020653, 0.02943766920977993959, 0.03135571078649940918, 0.03231473157485914571, 0.03327375236321888224, 0.03423277315157861878, 0.03519179393993834837, 0.03710983551665782143, 0.03902787709337729449, 0.03998689788173703102, 0.04094591867009676756 ),
 ( 0.000000000000000000, 1.000000000000000000 ),
 .UNSPECIFIED. ) 
 GEOMETRIC_REPRESENTATION_ITEM ( )  RATIONAL_B_SPLINE_SURFACE ( (
 ( 1.000000000000000000, 0.7071067811865475727, 1.000000000000000000),
 ( 1.000000000000000000, 0.7071067811865475727, 1.000000000000000000),
 ( 1.000000000000000000, 0.7071067811865475727, 1.000000000000000000),
 ( 1.000000000000000000, 0.7071067811865475727, 1.000000000000000000),
 ( 1.000000000000000000, 0.7071067811865475727, 1.000000000000000000),
 ( 1.000000000000000000, 0.7071067811865475727, 1.000000000000000000),
 ( 1.000000000000000000, 0.7071067811865475727, 1.000000000000000000),
 ( 1.000000000000000000, 0.7071067811865475727, 1.000000000000000000),
 ( 1.000000000000000000, 0.7071067811865471286, 1.000000000000000000),
 ( 1.000000000000000000, 0.7071067811865471286, 1.000000000000000000),
 ( 1.000000000000000000, 0.7071067811865475727, 1.000000000000000000),
 ( 1.000000000000000000, 0.7071067811865475727, 1.000000000000000000),
 ( 1.000000000000000000, 0.7071067811865465735, 1.000000000000000000),
 ( 1.000000000000000000, 0.7071067811865465735, 1.000000000000000000),
 ( 1.000000000000000000, 0.7071067811865475727, 1.000000000000000000),
 ( 1.000000000000000000, 0.7071067811865475727, 1.000000000000000000),
 ( 1.000000000000000000, 0.7071067811865483499, 1.000000000000000000),
 ( 1.000000000000000000, 0.7071067811865483499, 1.000000000000000000),
 ( 1.000000000000000000, 0.7071067811865475727, 1.000000000000000000),
 ( 1.000000000000000000, 0.7071067811865475727, 1.000000000000000000),
 ( 1.000000000000000000, 0.7071067811865475727, 1.000000000000000000),
 ( 1.000000000000000000, 0.7071067811865475727, 1.000000000000000000),
 ( 1.000000000000000000, 0.7071067811865475727, 1.000000000000000000),
 ( 1.000000000000000000, 0.7071067811865475727, 1.000000000000000000),
 ( 1.000000000000000000, 0.7071067811865481278, 1.000000000000000000),
 ( 1.000000000000000000, 0.7071067811865481278, 1.000000000000000000),
 ( 1.000000000000000000, 0.7071067811865476838, 1.000000000000000000),
 ( 1.000000000000000000, 0.7071067811865476838, 1.000000000000000000),
 ( 1.000000000000000000, 0.7071067811865475727, 1.000000000000000000),
 ( 1.000000000000000000, 0.7071067811865475727, 1.000000000000000000),
 ( 1.000000000000000000, 0.7071067811865476838, 1.000000000000000000),
 ( 1.000000000000000000, 0.7071067811865476838, 1.000000000000000000),
 ( 1.000000000000000000, 0.7071067811865476838, 1.000000000000000000),
 ( 1.000000000000000000, 0.7071067811865476838, 1.000000000000000000),
 ( 1.000000000000000000, 0.7071067811865475727, 1.000000000000000000),
 ( 1.000000000000000000, 0.7071067811865475727, 1.000000000000000000),
 ( 1.000000000000000000, 0.7071067811865475727, 1.000000000000000000),
 ( 1.000000000000000000, 0.7071067811865475727, 1.000000000000000000) ) ) 
 REPRESENTATION_ITEM ( '' )  SURFACE ( )  );
#25413 = DIRECTION ( 'NONE',  ( 0.000000000000000000, 1.000000000000000000, 0.000000000000000000 ) ) ;
#25414 = CARTESIAN_POINT ( 'NONE',  ( 10.00000000000000178, -8.574039729943018837E-16, 0.000000000000000000 ) ) ;
#25415 = EDGE_CURVE ( 'NONE', #20676, #18033, #14586, .T. ) ;
#25416 = CARTESIAN_POINT ( 'NONE',  ( 21.73500000136559507, 3.156283516753366047, 0.9349337715887203748 ) ) ;
#25417 = CARTESIAN_POINT ( 'NONE',  ( 40.87760899950266946, -5.748707280015221244, 3.993433839266994578 ) ) ;
#25418 = CARTESIAN_POINT ( 'NONE',  ( -2.249829636652692866, -12.47730163696535932, -1.743879033398587408 ) ) ;
#25419 = CARTESIAN_POINT ( 'NONE',  ( 41.19430503358938012, -3.886431767412240390, -0.07017451552781626967 ) ) ;
#25420 = DIRECTION ( 'NONE',  ( 1.000000000000000000, -8.574039729943018344E-17, -0.000000000000000000 ) ) ;
#25421 = CARTESIAN_POINT ( 'NONE',  ( 48.06508596181272708, -7.548662730762578654, 4.522129901861162260 ) ) ;
#25422 = ORIENTED_EDGE ( 'NONE', *, *, #8961, .T. ) ;
#25423 = CARTESIAN_POINT ( 'NONE',  ( 2.970200582150003932, 7.065646041994371629, -5.831559621433123120 ) ) ;
#25424 = B_SPLINE_CURVE_WITH_KNOTS ( 'NONE', 3,
 ( #30892, #12646, #23200, #15317, #20691, #17494, #20348, #25370 ),
 .UNSPECIFIED., .F., .F.,
 ( 4, 2, 2, 4 ),
 ( 0.000000000000000000, 0.5000000000000000000, 0.7500000000000000000, 1.000000000000000000 ),
 .UNSPECIFIED. ) ;
#25425 = PERSON_AND_ORGANIZATION_ROLE ( 'design_owner' ) ;
#25426 = DIRECTION ( 'NONE',  ( -2.219124775574841595E-17, -0.2588190451025108030, -0.9659258262890709767 ) ) ;
#25427 = ORIENTED_EDGE ( 'NONE', *, *, #27110, .F. ) ;
#25428 = DIRECTION ( 'NONE',  ( -0.000000000000000000, -0.000000000000000000, -1.000000000000000000 ) ) ;
#25429 = ORIENTED_EDGE ( 'NONE', *, *, #19148, .T. ) ;
#25430 = DIRECTION ( 'NONE',  ( 1.000000000000000000, -8.574039729943018344E-17, -0.000000000000000000 ) ) ;
#25432 = VERTEX_POINT ( 'NONE', #7354 ) ;
#25431 = CARTESIAN_POINT ( 'NONE',  ( 84.96680598075437274, -4.078993907564744781, -4.023789378516497983 ) ) ;
#25433 = VERTEX_POINT ( 'NONE', #2026 ) ;
#25434 = CARTESIAN_POINT ( 'NONE',  ( 43.74661801760413482, -24.08792321988613594, -1.500000000000000000 ) ) ;
#25435 = CARTESIAN_POINT ( 'NONE',  ( -6.312550801365593323, 3.675193018007246959, -1.088641768524161391 ) ) ;
#25436 = CARTESIAN_POINT ( 'NONE',  ( 0.000000000000000000, 3.771202944355777298, -4.982773259188332027 ) ) ;
#25437 = CARTESIAN_POINT ( 'NONE',  ( 0.000000000000000000, -6.106419733535023653, 3.518755179752782958 ) ) ;
#25439 = ORIENTED_EDGE ( 'NONE', *, *, #28198, .T. ) ;
#25438 = PLANE ( 'NONE',  #9095 ) ;
#25440 = CARTESIAN_POINT ( 'NONE',  ( 15.28872660057388799, 20.76088595412472060, 4.629213727441584325 ) ) ;
#25441 = FACE_OUTER_BOUND ( 'NONE', #30083, .T. ) ;
#25442 = CARTESIAN_POINT ( 'NONE',  ( 5.539187815124529735, -17.99452416398525045, 1.748481376116554742 ) ) ;
#25443 = EDGE_CURVE ( 'NONE', #26609, #32682, #19920, .T. ) ;
#25444 = CARTESIAN_POINT ( 'NONE',  ( 9.437548970008963423, 0.1642588933130686435, -1.500000000000000000 ) ) ;
#25445 = ADVANCED_FACE ( 'NONE', ( #27742 ), #19733, .F. ) ;
#25447 = ORIENTED_EDGE ( 'NONE', *, *, #4921, .F. ) ;
#25446 = CARTESIAN_POINT ( 'NONE',  ( 5.520790571833095406, 0.5174497483512504603, 5.764727407554761207 ) ) ;
#25448 = CARTESIAN_POINT ( 'NONE',  ( 7.077711312404847644E-17, 0.8254815157535873027, -4.681538312723508177 ) ) ;
#25449 = EDGE_CURVE ( 'NONE', #5453, #5774, #30130, .T. ) ;
#25450 = CARTESIAN_POINT ( 'NONE',  ( 56.97280603064898941, -277.2763395528616002, 4.999054092451785891 ) ) ;
#25451 = CARTESIAN_POINT ( 'NONE',  ( 24.04750000273118360, 0.7685399846772009713, -2.594547506269381909 ) ) ;
#25452 = PLANE ( 'NONE',  #6016 ) ;
#25453 = CARTESIAN_POINT ( 'NONE',  ( 7.249760686538667009, 7.199384779417189684, -4.973063321323801134 ) ) ;
#25454 = CARTESIAN_POINT ( 'NONE',  ( 0.5664946525141408840, -9.241976615262153416, 2.300561732649529567 ) ) ;
#25455 = ORIENTED_EDGE ( 'NONE', *, *, #20186, .F. ) ;
#25456 = CARTESIAN_POINT ( 'NONE',  ( 3.499999999999999556, 7.003298780661491918, -4.817032923780495857 ) ) ;
#25457 = CARTESIAN_POINT ( 'NONE',  ( 25.75999999999999801, -1.902510934646483477E-15, 2.499999999999997780 ) ) ;
#25458 = CARTESIAN_POINT ( 'NONE',  ( -6.287550801365593856, 2.228590825266444142, 2.752080473201636845 ) ) ;
#25459 = VERTEX_POINT ( 'NONE', #22398 ) ;
#25460 = CARTESIAN_POINT ( 'NONE',  ( -23.35000000000000142, -10.96966150227469505, -11.00000000000000000 ) ) ;
#25461 = CARTESIAN_POINT ( 'NONE',  ( 6.883866601413089370, 7.883091392499370187, -3.754588506078523569 ) ) ;
#25462 = CARTESIAN_POINT ( 'NONE',  ( 0.1610798642962581184, -10.72944008624797974, -4.522129901861164925 ) ) ;
#25463 = EDGE_LOOP ( 'NONE', ( #6355, #14413, #835 ) ) ;
#25464 = CARTESIAN_POINT ( 'NONE',  ( 11.02666429642763646, -12.67048613693261672, 1.000000000000000222 ) ) ;
#25465 = ORIENTED_EDGE ( 'NONE', *, *, #11618, .T. ) ;
#25466 = CARTESIAN_POINT ( 'NONE',  ( 0.7632845268398876781, -3.174628368996014860, -8.152713396088786979 ) ) ;
#25467 = ORIENTED_EDGE ( 'NONE', *, *, #30694, .F. ) ;
#25468 = DIRECTION ( 'NONE',  ( 0.9896144216807899463, -0.000000000000000000, 0.1437473352845038410 ) ) ;
#25470 = ORIENTED_EDGE ( 'NONE', *, *, #19494, .T. ) ;
#25469 = CARTESIAN_POINT ( 'NONE',  ( 108.1288400433390393, -19.92462668933126579, 3.636029349014985090 ) ) ;
#25471 = ORIENTED_EDGE ( 'NONE', *, *, #25708, .F. ) ;
#25472 = DIRECTION ( 'NONE',  ( -0.4999999999999978906, -0.8660254037844399289, -0.000000000000000000 ) ) ;
#25473 = VERTEX_POINT ( 'NONE', #14863 ) ;
#25474 = DIRECTION ( 'NONE',  ( -0.6916610887771488247, 0.000000000000000000, -0.7222222222222250965 ) ) ;
#25475 = ADVANCED_FACE ( 'NONE', ( #4849 ), #29772, .T. ) ;
#25477 = VERTEX_POINT ( 'NONE', #25252 ) ;
#25476 = CARTESIAN_POINT ( 'NONE',  ( 0.2678094507063553675, -7.640026513854723866, -1.500000000000000000 ) ) ;
#25478 = CARTESIAN_POINT ( 'NONE',  ( 0.1161733546981892212, -6.474819093472221176, -1.773743352647767502 ) ) ;
#25479 = FACE_OUTER_BOUND ( 'NONE', #30061, .T. ) ;
#25480 = CARTESIAN_POINT ( 'NONE',  ( 69.42401195566040428, -8.835509274236315491, 0.07017451552781736601 ) ) ;
#25481 = CARTESIAN_POINT ( 'NONE',  ( 0.3997463082871472451, -9.773321362167809667, 2.273557229425371418 ) ) ;
#25482 = EDGE_CURVE ( 'NONE', #8736, #72, #22749, .T. ) ;
#25483 = CARTESIAN_POINT ( 'NONE',  ( -56.27770248097862549, 0.4996615022747108448, -1.050000000000000044 ) ) ;
#25484 = ADVANCED_FACE ( 'NONE', ( #17398 ), #24564, .T. ) ;
#25485 = DIRECTION ( 'NONE',  ( 0.000000000000000000, 1.000000000000000000, 0.000000000000000000 ) ) ;
#25486 = CARTESIAN_POINT ( 'NONE',  ( 25.43628628520003687, -17.54453570558172260, 1.030327512441693516 ) ) ;
#25487 = CARTESIAN_POINT ( 'NONE',  ( 6.655951778521610684, -18.71196003547629516, 1.500000000000000000 ) ) ;
#25488 = CARTESIAN_POINT ( 'NONE',  ( 13.13178786250159469, -17.31629153505179275, 4.522129901861156931 ) ) ;
#25489 = CARTESIAN_POINT ( 'NONE',  ( 23.75111450864416440, -1.283275288181523244E-15, -2.499999999999998668 ) ) ;
#25490 = CARTESIAN_POINT ( 'NONE',  ( 68.56906952848913761, -3.255983411058662291, 0.02339150516273700783 ) ) ;
#25491 = EDGE_CURVE ( 'NONE', #27630, #19954, #24116, .T. ) ;
#25492 = FACE_OUTER_BOUND ( 'NONE', #18087, .T. ) ;
#25493 = CARTESIAN_POINT ( 'NONE',  ( 3.063284526839887167, 7.360373001730918574, 4.729683950898899703 ) ) ;
#25494 = ORIENTED_EDGE ( 'NONE', *, *, #20031, .F. ) ;
#25495 = CARTESIAN_POINT ( 'NONE',  ( -6.387550801365593500, 3.521866450007987037, 0.3701630799359328372 ) ) ;
#25496 = DIRECTION ( 'NONE',  ( 1.387778780781445676E-14, -1.000000000000000000, 0.000000000000000000 ) ) ;
#25497 = EDGE_CURVE ( 'NONE', #24488, #10254, #12052, .T. ) ;
#25498 = CARTESIAN_POINT ( 'NONE',  ( 18.02407935480697532, -21.25192265502663247, -1.530583967965385650 ) ) ;
#25499 = ORIENTED_EDGE ( 'NONE', *, *, #29625, .T. ) ;
#25500 = CARTESIAN_POINT ( 'NONE',  ( 1.750000000000000222, -5.848742439617962141, 6.167836887840968174 ) ) ;
#25501 = DIRECTION ( 'NONE',  ( 0.000000000000000000, 0.000000000000000000, 1.000000000000000000 ) ) ;
#25502 = EDGE_LOOP ( 'NONE', ( #32174, #23382, #11661, #16518 ) ) ;
#25503 = CYLINDRICAL_SURFACE ( 'NONE', #12388, 8.749000000000002331 ) ;
#25504 = EDGE_CURVE ( 'NONE', #14880, #17821, #5348, .T. ) ;
#25505 = DATE_TIME_ROLE ( 'classification_date' ) ;
#25507 = ORIENTED_EDGE ( 'NONE', *, *, #16049, .T. ) ;
#25506 = CARTESIAN_POINT ( 'NONE',  ( 18.53175858344379634, -21.44524224917989130, -1.499999999999999556 ) ) ;
#25508 = ORIENTED_EDGE ( 'NONE', *, *, #30669, .F. ) ;
#25509 = CARTESIAN_POINT ( 'NONE',  ( -3.657583913946364174, -9.739478672526409753, 1.743552423778348182 ) ) ;
#25510 = ORIENTED_EDGE ( 'NONE', *, *, #5077, .T. ) ;
#25511 = CARTESIAN_POINT ( 'NONE',  ( 108.0291781248180598, -18.48951985539477505, -4.325670280508457921 ) ) ;
#25513 = EDGE_LOOP ( 'NONE', ( #33025, #3646, #7585, #841 ) ) ;
#25512 = DIRECTION ( 'NONE',  ( 1.000000000000000000, -0.000000000000000000, -0.000000000000000000 ) ) ;
#25514 = CARTESIAN_POINT ( 'NONE',  ( 41.44907012423725234, -8.741883605793594469, 2.713652344655544724 ) ) ;
#25515 = CARTESIAN_POINT ( 'NONE',  ( 108.0980302657043239, -19.48097355589947810, 2.293520641443586250 ) ) ;
#25516 = EDGE_CURVE ( 'NONE', #6718, #22462, #12330, .T. ) ;
#25517 = CARTESIAN_POINT ( 'NONE',  ( 107.6641948605100083, -20.45809826282308208, 1.500000000000000000 ) ) ;
#25518 = EDGE_CURVE ( 'NONE', #6857, #15836, #31107, .T. ) ;
#25519 = CARTESIAN_POINT ( 'NONE',  ( 101.7699140880832402, -3.585303762756002932, 4.312047644407677183 ) ) ;
#25520 = EDGE_LOOP ( 'NONE', ( #17360, #21608 ) ) ;
#25521 = PRODUCT_DEFINITION_SHAPE ( 'NONE', 'NONE',  #1036 ) ;
#25522 = CARTESIAN_POINT ( 'NONE',  ( 4.499760686538666121, 0.000000000000000000, 0.000000000000000000 ) ) ;
#25523 = CARTESIAN_POINT ( 'NONE',  ( -32.08053788975120568, -0.0003384977252905707612, 1.500000000000000000 ) ) ;
#25524 = CARTESIAN_POINT ( 'NONE',  ( 0.000000000000000000, 1.425064293572489094, -10.85582367538892790 ) ) ;
#25525 = DIRECTION ( 'NONE',  ( 0.000000000000000000, 1.000000000000000000, 0.000000000000000000 ) ) ;
#25526 = EDGE_CURVE ( 'NONE', #11659, #4124, #28692, .T. ) ;
#25527 = LINE ( 'NONE', #131, #11359 ) ;
#25528 = CARTESIAN_POINT ( 'NONE',  ( -23.35000000000000142, -10.96966150227469505, -11.50000000000000000 ) ) ;
#25529 = CARTESIAN_POINT ( 'NONE',  ( -56.33942387371224214, 0.003472127128727200539, -1.004056851832535235 ) ) ;
#25530 = CARTESIAN_POINT ( 'NONE',  ( -56.27770248097862549, 0.4996615022747108448, -1.500000000000000000 ) ) ;
#25531 = ORIENTED_EDGE ( 'NONE', *, *, #23840, .T. ) ;
#25532 = CARTESIAN_POINT ( 'NONE',  ( -5.512550801365595277, 3.675193018007247403, -1.088641768524161391 ) ) ;
#25533 = ORIENTED_EDGE ( 'NONE', *, *, #32867, .F. ) ;
#25534 = EDGE_CURVE ( 'NONE', #25039, #15781, #15217, .T. ) ;
#25535 = CARTESIAN_POINT ( 'NONE',  ( -8.250050800000000351, 2.853674364686379583, 1.549418761218565921 ) ) ;
#25536 = CARTESIAN_POINT ( 'NONE',  ( 108.0552541750404174, 18.48583697376223967, 4.648293729490854176 ) ) ;
#25537 = CARTESIAN_POINT ( 'NONE',  ( 8.808801416188583033, -14.57828162013994344, 1.754901028757273496 ) ) ;
#25538 = CARTESIAN_POINT ( 'NONE',  ( 7.650166299107816315, -9.403575859904028889, 1.000000000000000000 ) ) ;
#25539 = ORIENTED_EDGE ( 'NONE', *, *, #854, .T. ) ;
#25540 = DIRECTION ( 'NONE',  ( 0.000000000000000000, 0.000000000000000000, 1.000000000000000000 ) ) ;
#25541 = VERTEX_POINT ( 'NONE', #7859 ) ;
#25542 = DIRECTION ( 'NONE',  ( 0.000000000000000000, 0.000000000000000000, 1.000000000000000000 ) ) ;
#25543 = DATE_TIME_ROLE ( 'creation_date' ) ;
#25544 = CARTESIAN_POINT ( 'NONE',  ( 54.97561860524439936, -6.448546075709844949, 4.073741752267325822 ) ) ;
#25545 = EDGE_CURVE ( 'NONE', #14768, #9701, #4461, .T. ) ;
#25546 = CARTESIAN_POINT ( 'NONE',  ( 18.96091535642496240, -3.614110606601104614, -2.184956778830005053 ) ) ;
#25548 = LINE ( 'NONE', #2655, #2243 ) ;
#25547 = CARTESIAN_POINT ( 'NONE',  ( 0.000000000000000000, 9.620177616658057929, -5.227991826303984624 ) ) ;
#25549 = B_SPLINE_CURVE_WITH_KNOTS ( 'NONE', 3,
 ( #16858, #16691, #29087, #4008, #24375, #21711, #26902, #19197 ),
 .UNSPECIFIED., .F., .F.,
 ( 4, 2, 2, 4 ),
 ( 5.099451029798772576E-07, 0.001229189835650483162, 0.001843529780924232616, 0.002457869726197984238 ),
 .UNSPECIFIED. ) ;
#25550 = EDGE_LOOP ( 'NONE', ( #6782, #15515, #12529, #14412, #13855 ) ) ;
#25551 = EDGE_CURVE ( 'NONE', #24705, #32504, #8712, .T. ) ;
#25552 = CARTESIAN_POINT ( 'NONE',  ( 0.08034252266852319468, -1.301095883299200562, -10.71005054582364302 ) ) ;
#25553 = EDGE_CURVE ( 'NONE', #32816, #9958, #10522, .T. ) ;
#25554 = DIRECTION ( 'NONE',  ( 0.000000000000000000, 0.000000000000000000, 1.000000000000000000 ) ) ;
#25555 = CARTESIAN_POINT ( 'NONE',  ( 24.42250000136559507, -0.3178988483021076838, -3.024605502323848949 ) ) ;
#25556 = PLANE ( 'NONE',  #14501 ) ;
#25558 = ORIENTED_EDGE ( 'NONE', *, *, #17464, .T. ) ;
#25557 = CARTESIAN_POINT ( 'NONE',  ( 5.887529755120530339, 8.323904922804413076, -1.089605374054287701 ) ) ;
#25559 = CARTESIAN_POINT ( 'NONE',  ( -7.412550801365592967, -3.368539882008727115, -1.828967928396028064 ) ) ;
#25560 = DIRECTION ( 'NONE',  ( -0.000000000000000000, -1.000000000000000000, -0.000000000000000000 ) ) ;
#25561 = CARTESIAN_POINT ( 'NONE',  ( 3.249999999999999556, -5.538577986808848941, -6.772677083992448388 ) ) ;
#25562 = DIRECTION ( 'NONE',  ( -0.000000000000000000, -1.000000000000000000, 0.000000000000000000 ) ) ;
#25563 = ORIENTED_EDGE ( 'NONE', *, *, #28766, .F. ) ;
#25565 = VERTEX_POINT ( 'NONE', #30622 ) ;
#25564 = CARTESIAN_POINT ( 'NONE',  ( 23.03249562537846984, -17.15537757201845181, 1.465178982930523066 ) ) ;
#25566 = LINE ( 'NONE', #18200, #1679 ) ;
#25567 = DIRECTION ( 'NONE',  ( 1.000000000000000000, -0.000000000000000000, -0.000000000000000000 ) ) ;
#25568 = CARTESIAN_POINT ( 'NONE',  ( 23.92250000136559507, 0.3178988483021036315, 3.024605502323848949 ) ) ;
#25569 = ADVANCED_FACE ( 'NONE', ( #15533 ), #21071, .T. ) ;
#25570 = CARTESIAN_POINT ( 'NONE',  ( 102.3175034158304015, -2.480357097896682905, 3.390608474933819672 ) ) ;
#25571 = CARTESIAN_POINT ( 'NONE',  ( 2.661997913519438264, 2.255009087902927867, 9.876677602395371736 ) ) ;
#25572 = CARTESIAN_POINT ( 'NONE',  ( 25.75999999999999801, -2.208672634433321348E-15, 0.000000000000000000 ) ) ;
#25573 = CARTESIAN_POINT ( 'NONE',  ( 8.886976913778033449, 2.271465516421269619E-16, 1.168311665897490581 ) ) ;
#25574 = CARTESIAN_POINT ( 'NONE',  ( 1.624999999999999778, -9.680994141368733708, -5.222868219166961978 ) ) ;
#25575 = ORIENTED_EDGE ( 'NONE', *, *, #19097, .T. ) ;
#25576 = CARTESIAN_POINT ( 'NONE',  ( 3.499999999999999556, -0.1221666339524086348, 6.247805719894683918 ) ) ;
#25577 = DATE_AND_TIME ( #12860, #5543 ) ;
#25578 = CARTESIAN_POINT ( 'NONE',  ( 69.13057415542958495, -2.987362752442197955, 2.713652344655542503 ) ) ;
#25579 = ORIENTED_EDGE ( 'NONE', *, *, #24923, .F. ) ;
#25580 = EDGE_CURVE ( 'NONE', #30676, #3168, #26849, .T. ) ;
#25581 = CARTESIAN_POINT ( 'NONE',  ( 108.0672442999933196, 18.55260272057762094, -4.631666742912559975 ) ) ;
#25582 = ORIENTED_EDGE ( 'NONE', *, *, #6078, .T. ) ;
#25583 = CARTESIAN_POINT ( 'NONE',  ( -16.91631469035494462, 11.69557288659533434, 1.940592563500735501 ) ) ;
#25584 = EDGE_CURVE ( 'NONE', #30847, #13402, #17901, .T. ) ;
#25586 = EDGE_LOOP ( 'NONE', ( #28819, #4082, #18700, #1485 ) ) ;
#25585 = CARTESIAN_POINT ( 'NONE',  ( 102.3446554920049465, -2.864632698915883235, -4.008637373583407992 ) ) ;
#25587 = VERTEX_POINT ( 'NONE', #5190 ) ;
#25588 = CARTESIAN_POINT ( 'NONE',  ( -0.1366093623685602776, -14.96249823008941604, -1.500000000000000000 ) ) ;
#25589 = CARTESIAN_POINT ( 'NONE',  ( -7.162550801365593856, 2.752080473201636845, -2.228590825266444142 ) ) ;
#25590 = DIRECTION ( 'NONE',  ( -1.000000000000000000, -0.000000000000000000, -0.000000000000000000 ) ) ;
#25591 = CARTESIAN_POINT ( 'NONE',  ( 4.749760686538667009, 7.892520144992435149, 1.391664247347255134 ) ) ;
#25592 = AXIS2_PLACEMENT_3D ( 'NONE', #24321, #26826, #3948 ) ;
#25593 =( BOUNDED_CURVE ( )  B_SPLINE_CURVE ( 2, ( #13907, #17281, #7393, #27975, #22287, #15254, #17583, #24952, #30319, #27478, #25109, #2566, #30172, #27786, #12416, #20276, #7244, #9557, #22633, #4734, #25301, #19968, #4898, #30479, #12091, #14756, #7562, #2227, #9743, #2412, #14903, #27634, #32841, #9912, #49, #5079, #25458, #12733, #29981, #4580, #20125, #15084, #22936, #12584, #10235, #20459, #22787, #32991, #19776, #22446, #2065, #30675, #24799, #32498, #10063, #12237, #1919, #17434, #7076, #17767, #32660, #7751, #17943, #28131, #5230, #8672, #13678, #31766, #990, #23125, #13824, #18696, #11172, #29390, #19042, #3665, #21374, #31585, #18890, #14004, #3354, #21555, #11352, #26714, #26241, #21709, #24029, #16505, #23732, #13520, #25614, #29085, #3523, #23880, #1156, #26421, #846, #6006, #11022, #21222, #31421, #6171, #28899, #28736, #16357, #26565, #16009, #8838, #29234, #3831, #7897, #242, #6317, #10414, #24219, #31919, #1339, #11515, #8497 ),
 .UNSPECIFIED., .F., .F. ) 
 B_SPLINE_CURVE_WITH_KNOTS ( ( 3, 2, 2, 2, 2, 2, 2, 2, 2, 2, 2, 2, 2, 2, 2, 2, 2, 2, 2, 2, 2, 2, 2, 2, 2, 2, 2, 2, 2, 2, 2, 2, 2, 2, 2, 2, 2, 2, 2, 2, 2, 2, 2, 2, 2, 2, 2, 2, 2, 2, 2, 2, 2, 2, 2, 2, 2, 2, 2, 3 ),
 ( 0.02919498387531501912, 0.03125000000000000000, 0.04687500000000000000, 0.06250000000000000000, 0.07812499999999998612, 0.09375000000000000000, 0.1093749999999999861, 0.1250000000000000000, 0.1406250000000000000, 0.1562500000000000000, 0.1718749999999999722, 0.1875000000000000000, 0.2031250000000000000, 0.2187500000000000000, 0.2343750000000000000, 0.2500000000000000000, 0.2656250000000000000, 0.2812500000000000000, 0.2968750000000000000, 0.3125000000000000000, 0.3281250000000000000, 0.3437500000000000000, 0.3593750000000000000, 0.3750000000000000555, 0.3906250000000000000, 0.4062500000000000000, 0.4218750000000000000, 0.4375000000000000000, 0.4531250000000000000, 0.4687500000000000000, 0.4843750000000000000, 0.5000000000000000000, 0.5156250000000000000, 0.5312500000000000000, 0.5468750000000000000, 0.5625000000000000000, 0.5781250000000000000, 0.5937500000000000000, 0.6093750000000000000, 0.6250000000000000000, 0.6406250000000000000, 0.6562500000000000000, 0.6718750000000000000, 0.6875000000000000000, 0.7031250000000000000, 0.7187500000000000000, 0.7343750000000000000, 0.7500000000000000000, 0.7656250000000000000, 0.7812500000000000000, 0.7968750000000001110, 0.8125000000000000000, 0.8281250000000000000, 0.8437500000000000000, 0.8593750000000000000, 0.8750000000000000000, 0.8906250000000000000, 0.9062500000000000000, 0.9218750000000000000, 0.9278186525000968743 ),
 .UNSPECIFIED. ) 
 CURVE ( )  GEOMETRIC_REPRESENTATION_ITEM ( )  RATIONAL_B_SPLINE_CURVE ( ( 0.9826105456045359787, 0.9899885575610967159, 1.000000000000000000, 0.9238795325112867385, 1.000000000000000000, 0.9238795325112867385, 1.000000000000000000, 0.9238795325112867385, 1.000000000000000000, 0.9238795325112867385, 1.000000000000000000, 0.9238795325112867385, 1.000000000000000000, 0.9238795325112867385, 1.000000000000000000, 0.9238795325112867385, 1.000000000000000000, 0.9238795325112867385, 1.000000000000000000, 0.9238795325112867385, 1.000000000000000000, 0.9238795325112867385, 1.000000000000000000, 0.9238795325112867385, 1.000000000000000000, 0.9238795325112867385, 1.000000000000000000, 0.9238795325112867385, 1.000000000000000000, 0.9238795325112867385, 1.000000000000000000, 0.9238795325112867385, 1.000000000000000000, 0.9238795325112867385, 1.000000000000000000, 0.9238795325112867385, 1.000000000000000000, 0.9238795325112867385, 1.000000000000000000, 0.9238795325112867385, 1.000000000000000000, 0.9238795325112867385, 1.000000000000000000, 0.9238795325112867385, 1.000000000000000000, 0.9238795325112867385, 1.000000000000000000, 0.9238795325112867385, 1.000000000000000000, 0.9238795325112867385, 1.000000000000000000, 0.9238795325112867385, 1.000000000000000000, 0.9238795325112867385, 1.000000000000000000, 0.9238795325112867385, 1.000000000000000000, 0.9238795325112867385, 1.000000000000000000, 0.9238795325112867385, 1.000000000000000000, 0.9238795325112867385, 1.000000000000000000, 0.9238795325112867385, 1.000000000000000000, 0.9238795325112867385, 1.000000000000000000, 0.9238795325112867385, 1.000000000000000000, 0.9238795325112867385, 1.000000000000000000, 0.9238795325112867385, 1.000000000000000000, 0.9238795325112867385, 1.000000000000000000, 0.9238795325112867385, 1.000000000000000000, 0.9238795325112867385, 1.000000000000000000, 0.9238795325112867385, 1.000000000000000000, 0.9238795325112867385, 1.000000000000000000, 0.9238795325112867385, 1.000000000000000000, 0.9238795325112867385, 1.000000000000000000, 0.9238795325112867385, 1.000000000000000000, 0.9238795325112867385, 1.000000000000000000, 0.9238795325112867385, 1.000000000000000000, 0.9238795325112867385, 1.000000000000000000, 0.9238795325112867385, 1.000000000000000000, 0.9238795325112867385, 1.000000000000000000, 0.9238795325112867385, 1.000000000000000000, 0.9238795325112867385, 1.000000000000000000, 0.9238795325112867385, 1.000000000000000000, 0.9238795325112867385, 1.000000000000000000, 0.9238795325112867385, 1.000000000000000000, 0.9238795325112867385, 1.000000000000000000, 0.9238795325112867385, 1.000000000000000000, 0.9238795325112867385, 1.000000000000000000, 0.9238795325112867385, 1.000000000000000000, 0.9710442491585387081, 0.9641176721898496726 ) ) 
 REPRESENTATION_ITEM ( '' )  );
#25595 = ORIENTED_EDGE ( 'NONE', *, *, #30965, .T. ) ;
#25594 = CARTESIAN_POINT ( 'NONE',  ( 22.36000000273118715, 1.942864903642424146, 1.573300977624592534 ) ) ;
#25596 = CARTESIAN_POINT ( 'NONE',  ( 23.22564588060107482, -21.93932300456764040, 1.500000000000000000 ) ) ;
#25597 = CARTESIAN_POINT ( 'NONE',  ( 0.9232102171129904500, 0.000000000000000000, 4.522129901861156931 ) ) ;
#25598 = CARTESIAN_POINT ( 'NONE',  ( -0.3253503806707769841, -14.55949634428441009, 1.745204865412639306 ) ) ;
#25599 = CARTESIAN_POINT ( 'NONE',  ( 24.29750000136559507, -0.3178988483021076838, -3.024605502323848949 ) ) ;
#25600 = CARTESIAN_POINT ( 'NONE',  ( 24.80306213860341558, -17.49230408913766865, 1.499999999999999778 ) ) ;
#25602 = EDGE_LOOP ( 'NONE', ( #20519, #20103, #31314, #14683 ) ) ;
#25601 = DIRECTION ( 'NONE',  ( 0.000000000000000000, 0.000000000000000000, 1.000000000000000000 ) ) ;
#25603 = CARTESIAN_POINT ( 'NONE',  ( 2.274274201625327230, 7.593217523260696211, -7.958834565716686349 ) ) ;
#25604 = DIRECTION ( 'NONE',  ( 0.000000000000000000, -0.08715574274764813223, -0.9961946980917464334 ) ) ;
#25605 = CARTESIAN_POINT ( 'NONE',  ( 22.79750000136559862, 0.3178988483021036315, 3.024605502323848949 ) ) ;
#25606 = CARTESIAN_POINT ( 'NONE',  ( 10.00000000000000000, 4.681538312723516171, 0.8254815157535410064 ) ) ;
#25607 = AXIS2_PLACEMENT_3D ( 'NONE', #18315, #28671, #31209 ) ;
#25608 = FACE_OUTER_BOUND ( 'NONE', #23203, .T. ) ;
#25609 = CARTESIAN_POINT ( 'NONE',  ( 0.000000000000000000, 0.000000000000000000, 0.000000000000000000 ) ) ;
#25610 = ORIENTED_EDGE ( 'NONE', *, *, #11546, .F. ) ;
#25611 = CARTESIAN_POINT ( 'NONE',  ( 23.04481819307356005, -21.91824019632980836, 1.500000000000000000 ) ) ;
#25612 = CIRCLE ( 'NONE', #21335, 6.000000000000000888 ) ;
#25613 = CARTESIAN_POINT ( 'NONE',  ( -40.16771308880407076, -10.96999999999998643, 5.949999999999999289 ) ) ;
#25614 = CARTESIAN_POINT ( 'NONE',  ( -3.587550801365593678, -3.521866450007987037, -0.3701630799359323931 ) ) ;
#25615 = EDGE_LOOP ( 'NONE', ( #3169, #9254, #14199, #3844 ) ) ;
#25616 = CIRCLE ( 'NONE', #19726, 5.010000000000000675 ) ;
#25617 = CARTESIAN_POINT ( 'NONE',  ( 25.59254563806580762, 1.901228607813702398, 2.157594591774798509 ) ) ;
#25618 = DIRECTION ( 'NONE',  ( -1.000000000000000000, 0.000000000000000000, -0.000000000000000000 ) ) ;
#25619 = CARTESIAN_POINT ( 'NONE',  ( -0.3880080537174158128, -2.647099810593990465, -4.522129901861164925 ) ) ;
#25620 = CARTESIAN_POINT ( 'NONE',  ( 23.57316428367674277, -9.051964865549241068, 0.07017451552781736601 ) ) ;
#25621 = ADVANCED_FACE ( 'NONE', ( #28419 ), #15366, .T. ) ;
#25622 = EDGE_LOOP ( 'NONE', ( #3385, #10897, #26797, #31912 ) ) ;
#25623 = EDGE_CURVE ( 'NONE', #15369, #12234, #29870, .T. ) ;
#25624 = DIRECTION ( 'NONE',  ( -1.000000000000000000, -0.000000000000000000, -0.000000000000000000 ) ) ;
#25625 = VERTEX_POINT ( 'NONE', #12851 ) ;
#25626 = CARTESIAN_POINT ( 'NONE',  ( 29.21519671786122885, -8.552672223064927692, 2.713652344655544724 ) ) ;
#25627 = EDGE_CURVE ( 'NONE', #16073, #4298, #10371, .T. ) ;
#25629 = ORIENTED_EDGE ( 'NONE', *, *, #613, .T. ) ;
#25628 = DIRECTION ( 'NONE',  ( 1.000000000000000000, -0.000000000000000000, -0.000000000000000000 ) ) ;
#25630 = ORIENTED_EDGE ( 'NONE', *, *, #30040, .F. ) ;
#25631 = CARTESIAN_POINT ( 'NONE',  ( 5.377543748152549874, 5.151476664237477188, 6.139290821770273077 ) ) ;
#25632 = VERTEX_POINT ( 'NONE', #13043 ) ;
#25633 = FACE_OUTER_BOUND ( 'NONE', #1655, .T. ) ;
#25635 = ORIENTED_EDGE ( 'NONE', *, *, #18364, .F. ) ;
#25634 = CARTESIAN_POINT ( 'NONE',  ( 16.80274661516410006, -16.53680364986711737, 1.500000000000000000 ) ) ;
#25636 = LINE ( 'NONE', #2752, #14528 ) ;
#25637 = CIRCLE ( 'NONE', #14971, 10.96966150227469328 ) ;
#25638 = CARTESIAN_POINT ( 'NONE',  ( 0.3941402309825520200, -8.465515007537584680, -1.772213618796667722 ) ) ;
#25639 = CARTESIAN_POINT ( 'NONE',  ( 1.624999999999999778, -1.975651141462315907, 10.82112760146735475 ) ) ;
#25640 = CARTESIAN_POINT ( 'NONE',  ( 17.02282544784375418, -15.06900748075850416, -1.000000000000138556 ) ) ;
#25641 = DIRECTION ( 'NONE',  ( -1.000000000000000000, 8.574039729943019576E-17, 1.232595164407830946E-32 ) ) ;
#25642 = CARTESIAN_POINT ( 'NONE',  ( 5.612718622971679672, 2.996580135471525796, 7.650113768151185489 ) ) ;
#25643 = AXIS2_PLACEMENT_3D ( 'NONE', #12446, #7594, #22960 ) ;
#25644 = CARTESIAN_POINT ( 'NONE',  ( 109.6329156864505165, 19.01855260168436246, -4.612695725900421984 ) ) ;
#25645 = LINE ( 'NONE', #15789, #11292 ) ;
#25646 = LINE ( 'NONE', #20654, #14643 ) ;
#25647 = CARTESIAN_POINT ( 'NONE',  ( 43.89586892125095119, -24.33975351994666525, 0.9788672205877712029 ) ) ;
#25648 = CARTESIAN_POINT ( 'NONE',  ( -1.047937531484013585, -4.989690239015236450, 4.522129901861156931 ) ) ;
#25649 = DIRECTION ( 'NONE',  ( 0.000000000000000000, 0.000000000000000000, 1.000000000000000000 ) ) ;
#25650 = DIRECTION ( 'NONE',  ( 0.000000000000000000, 0.000000000000000000, 1.000000000000000000 ) ) ;
#25651 = AXIS2_PLACEMENT_3D ( 'NONE', #32771, #30591, #10000 ) ;
#25652 = CARTESIAN_POINT ( 'NONE',  ( 18.87102749435254267, -4.618876501925000433, 5.695980980372492120 ) ) ;
#25653 = DIRECTION ( 'NONE',  ( -0.000000000000000000, -1.000000000000000000, -0.000000000000000000 ) ) ;
#25654 = EDGE_LOOP ( 'NONE', ( #23902, #24527, #32945, #23056, #18445 ) ) ;
#25655 = CARTESIAN_POINT ( 'NONE',  ( -5.487550801365593145, 2.228590825266444142, 2.752080473201636845 ) ) ;
#25656 = VECTOR ( 'NONE', #29610, 1000.000000000000000 ) ;
#25657 = EDGE_CURVE ( 'NONE', #31776, #19352, #15107, .T. ) ;
#25658 = AXIS2_PLACEMENT_3D ( 'NONE', #10394, #27951, #12219 ) ;
#25659 = DIRECTION ( 'NONE',  ( 4.163336342344337027E-14, 0.03489949670250347413, 0.9993908270190957621 ) ) ;
#25660 = EDGE_LOOP ( 'NONE', ( #2196, #28282, #2463, #18974, #20146, #12959, #11278, #4742, #9719, #6900, #27049, #21235, #30839, #2979, #1501, #28368, #23211, #3934, #20394, #2518, #10684, #23815, #19868, #11029, #10693, #28542, #17952, #9047, #5726, #21720, #18980, #6560, #20821, #5371, #32284, #25368, #17879, #31601, #28181, #26618, #28055, #22144, #10312, #25269, #31459, #32847, #23335, #24570, #19891, #13278, #11872, #17009, #32080, #1817, #1961, #16825, #19, #2114, #1068, #31597, #12654, #15730, #12136, #28027 ) ) ;
#25661 = CARTESIAN_POINT ( 'NONE',  ( 7.249760686538667009, -5.064320921489771976, -7.135485519862050374 ) ) ;
#25662 =( NAMED_UNIT ( * ) PLANE_ANGLE_UNIT ( ) SI_UNIT ( $, .RADIAN. ) );
#25663 = AXIS2_PLACEMENT_3D ( 'NONE', #7962, #20531, #2476 ) ;
#25664 = B_SPLINE_CURVE_WITH_KNOTS ( 'NONE', 3,
 ( #18712, #28914, #16519, #14022, #24233, #8213, #23562, #686 ),
 .UNSPECIFIED., .F., .F.,
 ( 4, 2, 2, 4 ),
 ( 9.034501660023095868E-05, 0.009114482626497338522, 0.01362655143144589354, 0.01813862023639444682 ),
 .UNSPECIFIED. ) ;
#25665 = ORIENTED_EDGE ( 'NONE', *, *, #32453, .T. ) ;
#25666 = CARTESIAN_POINT ( 'NONE',  ( 41.43141396789280151, -2.886852813799071438, -0.07017451552781585333 ) ) ;
#25668 = ORIENTED_EDGE ( 'NONE', *, *, #20402, .F. ) ;
#25667 = CARTESIAN_POINT ( 'NONE',  ( 47.75999538435722513, -8.435302152663906483, 0.07017451552781736601 ) ) ;
#25669 = ORIENTED_EDGE ( 'NONE', *, *, #17611, .F. ) ;
#25670 = CARTESIAN_POINT ( 'NONE',  ( 102.5829460782277351, -0.8583298743146007270, 2.713652344655542503 ) ) ;
#25671 = ORIENTED_EDGE ( 'NONE', *, *, #22087, .F. ) ;
#25672 = CARTESIAN_POINT ( 'NONE',  ( 18.60402535543785518, -7.603424548862136589, -0.07017451552783579571 ) ) ;
#25674 = EDGE_LOOP ( 'NONE', ( #27027, #288, #27065 ) ) ;
#25673 = CARTESIAN_POINT ( 'NONE',  ( 33.81874022276145553, 19.50000000000000000, 13.00000000000011902 ) ) ;
#25675 = CARTESIAN_POINT ( 'NONE',  ( 9.302055952193859056, 0.2457637073201327793, 1.049999999999999822 ) ) ;
#25676 = CARTESIAN_POINT ( 'NONE',  ( 1.750000000000000000, -2.417132211460119251, 8.149077976821791580 ) ) ;
#25677 = B_SPLINE_CURVE_WITH_KNOTS ( 'NONE', 3,
 ( #3728, #29144, #13894, #18775, #24106, #5895, #11084, #31664, #21620, #5750, #752, #8895, #29293 ),
 .UNSPECIFIED., .F., .F.,
 ( 4, 3, 3, 3, 4 ),
 ( 8.673617379884035472E-19, 0.0002329468921300049229, 0.001653916346091481061, 0.002601229312345668468, 0.003274063357856006780 ),
 .UNSPECIFIED. ) ;
#25678 = AXIS2_PLACEMENT_3D ( 'NONE', #28080, #2515, #22738 ) ;
#25679 = CYLINDRICAL_SURFACE ( 'NONE', #11881, 0.5000000000000004441 ) ;
#25680 = DIRECTION ( 'NONE',  ( 0.000000000000000000, -0.9063077870366433864, -0.4226182617407134856 ) ) ;
#25681 = AXIS2_PLACEMENT_3D ( 'NONE', #5944, #18341, #26366 ) ;
#25682 = CIRCLE ( 'NONE', #12329, 6.000000000000000888 ) ;
#25683 = EDGE_LOOP ( 'NONE', ( #21760, #6474, #19777, #16508, #12688, #26880 ) ) ;
#25684 = VECTOR ( 'NONE', #18229, 1000.000000000000000 ) ;
#25685 = CARTESIAN_POINT ( 'NONE',  ( 7.064423669210280643, -6.226446564518083093, 6.147671362330662248 ) ) ;
#25686 = CARTESIAN_POINT ( 'NONE',  ( -14.47914180357919989, -28.43932300454937590, -4.314460059828594041 ) ) ;
#25687 = EDGE_CURVE ( 'NONE', #21907, #3071, #27934, .T. ) ;
#25688 = CARTESIAN_POINT ( 'NONE',  ( 23.64680669417294823, -7.447390197414223145, -2.184956778807263689 ) ) ;
#25689 = CARTESIAN_POINT ( 'NONE',  ( 4.749760686538667009, -7.892520144992443143, 1.391664247347202288 ) ) ;
#25690 = VECTOR ( 'NONE', #9708, 1000.000000000000000 ) ;
#25691 = CARTESIAN_POINT ( 'NONE',  ( 23.05582684282763495, -21.92970410991115671, 1.098153529935464778 ) ) ;
#25692 = B_SPLINE_CURVE_WITH_KNOTS ( 'NONE', 3,
 ( #15612, #18113, #28309, #31000, #26316, #411 ),
 .UNSPECIFIED., .F., .F.,
 ( 4, 2, 4 ),
 ( 2.872315617932023530E-05, 0.0004097954672333709329, 0.0007908677782874217084 ),
 .UNSPECIFIED. ) ;
#25693 = DIRECTION ( 'NONE',  ( 0.000000000000000000, 0.000000000000000000, -1.000000000000000000 ) ) ;
#25694 = CARTESIAN_POINT ( 'NONE',  ( -56.65769528877406458, 0.1730602557903761496, -1.037707669418532319 ) ) ;
#25695 = FACE_OUTER_BOUND ( 'NONE', #31493, .T. ) ;
#25696 = VERTEX_POINT ( 'NONE', #26896 ) ;
#25697 = EDGE_CURVE ( 'NONE', #29923, #4178, #16208, .T. ) ;
#25698 = CARTESIAN_POINT ( 'NONE',  ( -6.662550801365592967, -3.521866450007987037, -0.3701630799359323931 ) ) ;
#25699 = ORIENTED_EDGE ( 'NONE', *, *, #11089, .T. ) ;
#25700 = CARTESIAN_POINT ( 'NONE',  ( -4.204531657079157547, 1.883076972206379374, 2.325406398514293205 ) ) ;
#25701 = VECTOR ( 'NONE', #3561, 1000.000000000000000 ) ;
#25702 = CARTESIAN_POINT ( 'NONE',  ( 107.4616540840862768, 17.99089616900343813, 4.860603037907947233 ) ) ;
#25703 = EDGE_CURVE ( 'NONE', #11175, #8263, #5012, .T. ) ;
#25704 = CARTESIAN_POINT ( 'NONE',  ( 6.944655341030708584, -13.87327314716643833, 1.755631441884608623 ) ) ;
#25705 = CARTESIAN_POINT ( 'NONE',  ( 20.69346795569472164, -16.15118080712967696, 0.9999999999998612221 ) ) ;
#25706 = EDGE_LOOP ( 'NONE', ( #31810, #2380, #14244, #32051 ) ) ;
#25707 = CARTESIAN_POINT ( 'NONE',  ( 0.000000000000000000, 4.058600654062949786, -7.468451026206159860 ) ) ;
#25708 = EDGE_CURVE ( 'NONE', #29447, #11755, #13823, .T. ) ;
#25709 = AXIS2_PLACEMENT_3D ( 'NONE', #2676, #20730, #15712 ) ;
#25710 = CIRCLE ( 'NONE', #26239, 5.009999999999999787 ) ;
#25711 = ORIENTED_EDGE ( 'NONE', *, *, #16403, .F. ) ;
#25712 = LINE ( 'NONE', #15688, #9154 ) ;
#25713 = APPROVAL_DATE_TIME ( #2839, #10447 ) ;
#25714 = APPLICATION_CONTEXT ( 'configuration controlled 3d designs of mechanical parts and assemblies' ) ;
#25715 = CARTESIAN_POINT ( 'NONE',  ( 54.97605132184205701, -6.464180995122740470, 4.053847711493757444 ) ) ;
#25716 = ADVANCED_FACE ( 'NONE', ( #28734 ), #16399, .F. ) ;
#25717 = ADVANCED_FACE ( 'NONE', ( #23731 ), #31918, .T. ) ;
#25718 = VECTOR ( 'NONE', #21265, 1000.000000000000114 ) ;
#25719 = CARTESIAN_POINT ( 'NONE',  ( 5.612974044843318744, -8.054452210044752647, -1.622927203279425967 ) ) ;
#25721 = FACE_BOUND ( 'NONE', #24382, .T. ) ;
#25720 = CARTESIAN_POINT ( 'NONE',  ( 25.23499999999999943, 0.2613211581691317065, 2.486304738420681559 ) ) ;
#25722 = ORIENTED_EDGE ( 'NONE', *, *, #15754, .F. ) ;
#25723 = CARTESIAN_POINT ( 'NONE',  ( -7.450050802731187360, 1.887961173149511618, 2.331437884370912705 ) ) ;
#25724 = FACE_OUTER_BOUND ( 'NONE', #3457, .T. ) ;
#25725 = EDGE_CURVE ( 'NONE', #9323, #29074, #3418, .T. ) ;
#25726 = CARTESIAN_POINT ( 'NONE',  ( 14.65314785874341119, -16.14430731538131170, -1.753659771011512269 ) ) ;
#25728 = ORIENTED_EDGE ( 'NONE', *, *, #7611, .F. ) ;
#25727 = FACE_OUTER_BOUND ( 'NONE', #5052, .T. ) ;
#25729 = CARTESIAN_POINT ( 'NONE',  ( -4.812550801365592434, 1.828967928396027176, -3.368539882008727115 ) ) ;
#25730 = CARTESIAN_POINT ( 'NONE',  ( -40.49265397688009216, -13.13403825401228708, 5.499999999999999112 ) ) ;
#25731 = CIRCLE ( 'NONE', #24109, 2.099999999999997868 ) ;
#25732 = CYLINDRICAL_SURFACE ( 'NONE', #3858, 2.999999999999999112 ) ;
#25733 = CARTESIAN_POINT ( 'NONE',  ( 4.888486331236938389E-17, -10.76487093102066517, 1.999317321091457655 ) ) ;
#25734 = ORIENTED_EDGE ( 'NONE', *, *, #6427, .F. ) ;
#25735 = VERTEX_POINT ( 'NONE', #16008 ) ;
#25736 = VECTOR ( 'NONE', #3478, 1000.000000000000000 ) ;
#25737 = AXIS2_PLACEMENT_3D ( 'NONE', #19500, #14133, #31873 ) ;
#25739 = AXIS2_PLACEMENT_3D ( 'NONE', #4349, #30270, #14197 ) ;
#25738 = CARTESIAN_POINT ( 'NONE',  ( 16.36487458112951643, 19.37645981759113312, -4.612695725900422872 ) ) ;
#25740 = CARTESIAN_POINT ( 'NONE',  ( 2.440333710190775829, -10.46055952248794796, -2.130583817698489479 ) ) ;
#25741 = AXIS2_PLACEMENT_3D ( 'NONE', #9020, #29940, #26941 ) ;
#25742 = LINE ( 'NONE', #22746, #3905 ) ;
#25743 = AXIS2_PLACEMENT_3D ( 'NONE', #12776, #25855, #20673 ) ;
#25744 = CIRCLE ( 'NONE', #18793, 2.999999999999999556 ) ;
#25745 = EDGE_CURVE ( 'NONE', #16397, #16840, #2423, .T. ) ;
#25746 = CARTESIAN_POINT ( 'NONE',  ( 7.249760686538667009, -6.940565734314625423, 4.007137495034787555 ) ) ;
#25747 = EDGE_CURVE ( 'NONE', #16362, #21274, #16199, .T. ) ;
#25748 = LINE ( 'NONE', #350, #3902 ) ;
#25749 = CARTESIAN_POINT ( 'NONE',  ( 47.95525692263736062, -8.175714017049896754, 1.529339665918354241 ) ) ;
#25750 = ORIENTED_EDGE ( 'NONE', *, *, #21559, .F. ) ;
#25751 = CARTESIAN_POINT ( 'NONE',  ( 0.7632845268398871230, 0.000000000000000000, 0.000000000000000000 ) ) ;
#25752 = EDGE_CURVE ( 'NONE', #19839, #18491, #2342, .T. ) ;
#25753 = VECTOR ( 'NONE', #9524, 1000.000000000000000 ) ;
#25755 = VECTOR ( 'NONE', #22818, 1000.000000000000000 ) ;
#25754 = PERSON_AND_ORGANIZATION_ROLE ( 'design_owner' ) ;
#25756 = LINE ( 'NONE', #18218, #20376 ) ;
#25757 = VERTEX_POINT ( 'NONE', #12509 ) ;
#25758 = AXIS2_PLACEMENT_3D ( 'NONE', #4942, #276, #17461 ) ;
#25759 = AXIS2_PLACEMENT_3D ( 'NONE', #8795, #6275, #1443 ) ;
#25760 = CARTESIAN_POINT ( 'NONE',  ( 108.0191616597610391, 18.28485960726052539, -4.516253988675255293 ) ) ;
#25761 = VECTOR ( 'NONE', #30742, 1000.000000000000227 ) ;
#25762 = ORIENTED_EDGE ( 'NONE', *, *, #13979, .F. ) ;
#25763 = CARTESIAN_POINT ( 'NONE',  ( -18.18687069758686903, 6.948720673121208335, 2.065371546005595693 ) ) ;
#25765 = VERTEX_POINT ( 'NONE', #12319 ) ;
#25764 = CARTESIAN_POINT ( 'NONE',  ( 84.98546029192083040, -4.383222815415539486, -4.275175582409524999 ) ) ;
#25766 = VERTEX_POINT ( 'NONE', #22211 ) ;
#25767 = VECTOR ( 'NONE', #15184, 1000.000000000000000 ) ;
#25768 = DIRECTION ( 'NONE',  ( 1.387778780781445676E-14, 0.000000000000000000, -1.000000000000000000 ) ) ;
#25769 = CARTESIAN_POINT ( 'NONE',  ( 8.528645601772334217, -0.5000000000000000000, -1.500000000000000000 ) ) ;
#25770 = CARTESIAN_POINT ( 'NONE',  ( 7.611844841314693078, -2.453950335954177220, 1.500000000000000000 ) ) ;
#25771 = CIRCLE ( 'NONE', #24706, 5.010000000000000675 ) ;
#25772 = EDGE_CURVE ( 'NONE', #25587, #14095, #22539, .T. ) ;
#25773 = CARTESIAN_POINT ( 'NONE',  ( 107.6365100547759397, -20.05945961560171753, -2.316983664052866043 ) ) ;
#25774 = PRODUCT_DEFINITION ( 'UNKNOWN', '', #1293, #24290 ) ;
#25776 = VERTEX_POINT ( 'NONE', #27051 ) ;
#25775 = CARTESIAN_POINT ( 'NONE',  ( 25.75999999999999801, 5.000000000000000000, 0.000000000000000000 ) ) ;
#25777 = FACE_OUTER_BOUND ( 'NONE', #4134, .T. ) ;
#25778 = CARTESIAN_POINT ( 'NONE',  ( 25.73747082621204640, 18.89898602765596536, 1.499999999998589573 ) ) ;
#25779 = CARTESIAN_POINT ( 'NONE',  ( -2.249933675096747354, -12.47715805579040982, 1.743879002063110528 ) ) ;
#25780 = CARTESIAN_POINT ( 'NONE',  ( 23.42250000136559862, 1.913930629741522838, -2.363507492473150062 ) ) ;
#25781 = CARTESIAN_POINT ( 'NONE',  ( 3.499999999999999556, -2.652816298622462376, 5.657964889053574531 ) ) ;
#25783 = ORIENTED_EDGE ( 'NONE', *, *, #13201, .T. ) ;
#25782 = DIRECTION ( 'NONE',  ( -0.000000000000000000, 0.000000000000000000, 1.000000000000000000 ) ) ;
#25784 = CARTESIAN_POINT ( 'NONE',  ( 7.249760686538667009, 7.892520144992453801, -1.391664247347147443 ) ) ;
#25785 = B_SPLINE_CURVE_WITH_KNOTS ( 'NONE', 3,
 ( #27429, #19913, #14536, #24746, #1870, #32451, #12045 ),
 .UNSPECIFIED., .F., .F.,
 ( 4, 3, 4 ),
 ( 5.449946885873038238E-17, 0.002561824599199770836, 0.003454325189396755934 ),
 .UNSPECIFIED. ) ;
#25786 = VECTOR ( 'NONE', #18908, 1000.000000000000000 ) ;
#25787 = VECTOR ( 'NONE', #32957, 1000.000000000000227 ) ;
#25788 = CARTESIAN_POINT ( 'NONE',  ( -28.91036633256500465, 15.51073349983545313, 1.844682940529381199 ) ) ;
#25789 = CARTESIAN_POINT ( 'NONE',  ( 25.17250000273118715, 2.378061970571979433, -1.291182301015470824 ) ) ;
#25790 = CIRCLE ( 'NONE', #32214, 5.009999999999999787 ) ;
#25791 = EDGE_CURVE ( 'NONE', #27055, #7787, #10469, .T. ) ;
#25792 = AXIS2_PLACEMENT_3D ( 'NONE', #30671, #15077, #9736 ) ;
#25793 = DIRECTION ( 'NONE',  ( 0.000000000000000000, 0.000000000000000000, -1.000000000000000000 ) ) ;
#25794 = AXIS2_PLACEMENT_3D ( 'NONE', #27476, #17580, #4577 ) ;
#25795 = CARTESIAN_POINT ( 'NONE',  ( -55.09999999999999432, -10.96966150227468972, 6.999999999999999112 ) ) ;
#25796 = DIRECTION ( 'NONE',  ( 0.000000000000000000, -0.000000000000000000, 1.000000000000000000 ) ) ;
#25797 = VERTEX_POINT ( 'NONE', #24708 ) ;
#25798 = DIRECTION ( 'NONE',  ( 0.000000000000000000, 0.9063077870366497146, -0.4226182617406997744 ) ) ;
#25799 = AXIS2_PLACEMENT_3D ( 'NONE', #23254, #14, #357 ) ;
#25800 = AXIS2_PLACEMENT_3D ( 'NONE', #8768, #32466, #32625 ) ;
#25801 = ORIENTED_EDGE ( 'NONE', *, *, #2251, .T. ) ;
#25802 = AXIS2_PLACEMENT_3D ( 'NONE', #26474, #3573, #28972 ) ;
#25803 = FACE_OUTER_BOUND ( 'NONE', #8623, .T. ) ;
#25804 = DIRECTION ( 'NONE',  ( -1.000000000000000000, 0.000000000000000000, -0.000000000000000000 ) ) ;
#25805 = CARTESIAN_POINT ( 'NONE',  ( 0.1517578099452217555, -1.375880305419572514, -4.522129901861164925 ) ) ;
#25807 = CARTESIAN_POINT ( 'NONE',  ( 107.9482911536555605, -17.32476759280069700, 4.518410020412943595 ) ) ;
#25806 = LINE ( 'NONE', #15092, #7576 ) ;
#25808 = ORIENTED_EDGE ( 'NONE', *, *, #19838, .F. ) ;
#25809 = AXIS2_PLACEMENT_3D ( 'NONE', #18152, #18004, #28191 ) ;
#25810 = CARTESIAN_POINT ( 'NONE',  ( -40.85893555729982296, -14.04586516063045210, 5.414538096233425968 ) ) ;
#25811 = VERTEX_POINT ( 'NONE', #9646 ) ;
#25812 = CARTESIAN_POINT ( 'NONE',  ( -3.226940125355896249, -1.840961574400530945E-05, 0.9957093966831336296 ) ) ;
#25813 = AXIS2_PLACEMENT_3D ( 'NONE', #8985, #19196, #16690 ) ;
#25815 = VERTEX_POINT ( 'NONE', #1835 ) ;
#25814 = CARTESIAN_POINT ( 'NONE',  ( 109.2312629696829731, 19.37684342964551476, -4.110854402524426021 ) ) ;
#25816 = ORIENTED_EDGE ( 'NONE', *, *, #31151, .T. ) ;
#25817 = CARTESIAN_POINT ( 'NONE',  ( 3.499999999999999556, 0.000000000000000000, 0.000000000000000000 ) ) ;
#25818 = VECTOR ( 'NONE', #9059, 1000.000000000000000 ) ;
#25819 = ADVANCED_FACE ( 'NONE', ( #4155 ), #1647, .F. ) ;
#25820 = CIRCLE ( 'NONE', #3932, 8.749000000000002331 ) ;
#25821 = VECTOR ( 'NONE', #3072, 1000.000000000000227 ) ;
#25822 = DIRECTION ( 'NONE',  ( 0.000000000000000000, 0.000000000000000000, 1.000000000000000000 ) ) ;
#25824 = ORIENTED_EDGE ( 'NONE', *, *, #19911, .T. ) ;
#25823 = CARTESIAN_POINT ( 'NONE',  ( 6.013832568680315127, -13.53405802968792848, 1.500000000000000000 ) ) ;
#25825 = EDGE_LOOP ( 'NONE', ( #18791, #15772, #8322, #5983 ) ) ;
#25826 = LINE ( 'NONE', #18284, #7981 ) ;
#25827 = DIRECTION ( 'NONE',  ( -1.000000000000000000, 0.000000000000000000, 0.000000000000000000 ) ) ;
#25828 = APPROVAL_PERSON_ORGANIZATION ( #16019, #9628, #18551 ) ;
#25829 = LINE ( 'NONE', #30854, #23488 ) ;
#25830 = CYLINDRICAL_SURFACE ( 'NONE', #3748, 6.000000000000000000 ) ;
#25831 = CARTESIAN_POINT ( 'NONE',  ( 2.440333653308765172, 4.424884217119425145, 9.715096239907426323 ) ) ;
#25832 = CARTESIAN_POINT ( 'NONE',  ( 5.377543748152550762, -1.391664247347281780, 7.892520144992429820 ) ) ;
#25833 = CARTESIAN_POINT ( 'NONE',  ( 3.857446109187582017, -11.79189269903710624, 1.500000000000000222 ) ) ;
#25834 = CARTESIAN_POINT ( 'NONE',  ( 102.4756904796924033, -4.748902435568509439, 2.787782622565551538 ) ) ;
#25835 = EDGE_CURVE ( 'NONE', #7000, #19723, #25056, .T. ) ;
#25836 = EDGE_CURVE ( 'NONE', #17341, #9887, #29896, .T. ) ;
#25837 = CARTESIAN_POINT ( 'NONE',  ( 3.122314033877900197E-16, 3.641590349731971710, -3.055657119358763829 ) ) ;
#25838 = CARTESIAN_POINT ( 'NONE',  ( 3.583596913636438064, -0.01388667853607550469, 1.134179515492628632 ) ) ;
#25839 = CIRCLE ( 'NONE', #20496, 0.4500000000000007327 ) ;
#25840 = CARTESIAN_POINT ( 'NONE',  ( -50.60000000000000142, -10.96966150227468972, 0.9999999999999991118 ) ) ;
#25841 =( BOUNDED_CURVE ( )  B_SPLINE_CURVE ( 3, ( #4396, #2210, #20112, #25092 ),
 .UNSPECIFIED., .F., .F. ) 
 B_SPLINE_CURVE_WITH_KNOTS ( ( 4, 4 ),
 ( 0.6009777071450068675, 1.570796326794896558 ),
 .UNSPECIFIED. ) 
 CURVE ( )  GEOMETRIC_REPRESENTATION_ITEM ( )  RATIONAL_B_SPLINE_CURVE ( ( 1.000000000000000000, 0.9231448173254028777, 0.9231448173254028777, 1.000000000000000000 ) ) 
 REPRESENTATION_ITEM ( '' )  );
#25842 = EDGE_CURVE ( 'NONE', #29122, #2806, #19541, .T. ) ;
#25843 = CIRCLE ( 'NONE', #19446, 297.9387600756452343 ) ;
#25844 = CARTESIAN_POINT ( 'NONE',  ( 29.27825211595694554, -6.695835137279974703, 5.695980980372492120 ) ) ;
#25845 = CARTESIAN_POINT ( 'NONE',  ( 13.44369214246638577, 21.88234542448674702, -1.272551993140566662 ) ) ;
#25846 = ORIENTED_EDGE ( 'NONE', *, *, #489, .F. ) ;
#25847 = AXIS2_PLACEMENT_3D ( 'NONE', #29124, #9024, #21119 ) ;
#25848 = CARTESIAN_POINT ( 'NONE',  ( -4.737550801365593145, 3.368539882008727115, 1.828967928396026954 ) ) ;
#25849 = CARTESIAN_POINT ( 'NONE',  ( -2.562942409646512321, -5.022711880624455567E-15, 2.999999999999999556 ) ) ;
#25850 = CARTESIAN_POINT ( 'NONE',  ( 0.000000000000000000, 0.000000000000000000, -3.750000000000000444 ) ) ;
#25851 = CC_DESIGN_APPROVAL ( #10447, ( #28213 ) ) ;
#25852 = ORIENTED_EDGE ( 'NONE', *, *, #32909, .F. ) ;
#25853 = CARTESIAN_POINT ( 'NONE',  ( 107.1769020805352142, 16.40214705320008903, -1.491740999229418829 ) ) ;
#25854 = ORIENTED_EDGE ( 'NONE', *, *, #31917, .T. ) ;
#25855 = DIRECTION ( 'NONE',  ( 1.000000000000000000, -8.574039729943018344E-17, -0.000000000000000000 ) ) ;
#25856 = DATE_TIME_ROLE ( 'classification_date' ) ;
#25858 = ORIENTED_EDGE ( 'NONE', *, *, #19596, .T. ) ;
#25857 = CARTESIAN_POINT ( 'NONE',  ( 3.554613218822866738, -15.76807188677470073, -4.522129901861166701 ) ) ;
#25859 = ORIENTED_EDGE ( 'NONE', *, *, #30420, .T. ) ;
#25860 = CARTESIAN_POINT ( 'NONE',  ( 7.249760686538667009, -6.147671362329178102, -6.226446564517978288 ) ) ;
#25861 = ORIENTED_EDGE ( 'NONE', *, *, #4723, .T. ) ;
#25862 = CARTESIAN_POINT ( 'NONE',  ( 25.76000000000000512, 0.9672760553990802368, 2.878205665084649478 ) ) ;
#25863 = CONICAL_SURFACE ( 'NONE', #21580, 9.500000000000003553, 0.1919862177193767117 ) ;
#25865 = ORIENTED_EDGE ( 'NONE', *, *, #27142, .F. ) ;
#25864 = CARTESIAN_POINT ( 'NONE',  ( -2.452970694446401811, 0.2355604519343507952, 3.112266013026773859 ) ) ;
#25866 = CARTESIAN_POINT ( 'NONE',  ( 48.08400536259535585, -8.675012021211058411, 2.713652344655544724 ) ) ;
#25867 = CARTESIAN_POINT ( 'NONE',  ( 108.0291781248179177, -18.48951985539285658, 4.325670280512381005 ) ) ;
#25868 = DIRECTION ( 'NONE',  ( -0.9896144216807905014, -0.000000000000000000, -0.1437473352845003161 ) ) ;
#25869 = CARTESIAN_POINT ( 'NONE',  ( 10.00000000000000000, -4.467071865485462645, -1.625881193364742572 ) ) ;
#25870 = VERTEX_POINT ( 'NONE', #19696 ) ;
#25871 = CARTESIAN_POINT ( 'NONE',  ( 0.000000000000000000, 0.000000000000000000, 0.000000000000000000 ) ) ;
#25872 = CARTESIAN_POINT ( 'NONE',  ( 25.75999999999999801, -2.208672634433321348E-15, 0.000000000000000000 ) ) ;
#25873 = DIRECTION ( 'NONE',  ( -1.000000000000000000, 0.000000000000000000, -0.000000000000000000 ) ) ;
#25874 = DIRECTION ( 'NONE',  ( 0.000000000000000000, 0.5735764363510413855, 0.8191520442889951292 ) ) ;
#25875 = SECURITY_CLASSIFICATION ( '', '', #23963 ) ;
#25876 = EDGE_CURVE ( 'NONE', #27844, #11829, #16855, .T. ) ;
#25877 = ADVANCED_FACE ( 'NONE', ( #29579 ), #6169, .T. ) ;
#25878 = ADVANCED_FACE ( 'NONE', ( #28616, #8374 ), #23757, .T. ) ;
#25879 = CARTESIAN_POINT ( 'NONE',  ( -15.60935834747760609, -25.43932300454937945, 1.500000000000000000 ) ) ;
#25880 = CARTESIAN_POINT ( 'NONE',  ( 0.5640491561200821069, -0.6680154998155144463, 9.516580665864458055 ) ) ;
#25881 = CARTESIAN_POINT ( 'NONE',  ( 23.98499999999999943, 2.486304738420679783, -0.2613211581691337604 ) ) ;
#25883 = CARTESIAN_POINT ( 'NONE',  ( 22.54151439274395585, -21.86162235810803267, 1.385141676429126001 ) ) ;
#25882 = UNCERTAINTY_MEASURE_WITH_UNIT (LENGTH_MEASURE( 1.000000000000000082E-05 ), #7029, 'distance_accuracy_value', 'NONE');
#25884 = B_SPLINE_CURVE_WITH_KNOTS ( 'NONE', 3,
 ( #9869, #17032, #2021, #32609, #22085, #4537, #9188, #7016, #29614, #12361 ),
 .UNSPECIFIED., .F., .F.,
 ( 4, 2, 2, 2, 4 ),
 ( 1.968338519003762927E-07, 0.0005467928198071721722, 0.001093388805762444006, 0.001639984791717715839, 0.002186580777672987672 ),
 .UNSPECIFIED. ) ;
#25885 = EDGE_LOOP ( 'NONE', ( #19580, #12283, #28523, #6742 ) ) ;
#25886 = CARTESIAN_POINT ( 'NONE',  ( -3.362550801365593589, -2.228590825266444586, -2.752080473201636401 ) ) ;
#25887 = VERTEX_POINT ( 'NONE', #10893 ) ;
#25888 = CARTESIAN_POINT ( 'NONE',  ( -8.500050800000000351, 0.3135853898029611342, -2.983565686104819648 ) ) ;
#25889 = VECTOR ( 'NONE', #946, 1000.000000000000000 ) ;
#25890 = CARTESIAN_POINT ( 'NONE',  ( 7.249760686538667009, 0.000000000000000000, 0.000000000000000000 ) ) ;
#25891 = DIRECTION ( 'NONE',  ( -1.000000000000000000, 0.000000000000000000, -0.000000000000000000 ) ) ;
#25892 = CARTESIAN_POINT ( 'NONE',  ( 9.827398781245818782, -12.51289689083618129, 1.500000000000000000 ) ) ;
#25893 = ORIENTED_EDGE ( 'NONE', *, *, #29080, .T. ) ;
#25894 = FACE_OUTER_BOUND ( 'NONE', #25082, .T. ) ;
#25895 = B_SPLINE_CURVE_WITH_KNOTS ( 'NONE', 3,
 ( #25466, #2576, #14913, #12592, #12428, #30685, #22946, #28138 ),
 .UNSPECIFIED., .F., .F.,
 ( 4, 2, 2, 4 ),
 ( 2.213836054352509658E-07, 0.001227982086136112207, 0.001841862437401450012, 0.002455742788666787600 ),
 .UNSPECIFIED. ) ;
#25896 = ORIENTED_EDGE ( 'NONE', *, *, #20448, .T. ) ;
#25897 = CARTESIAN_POINT ( 'NONE',  ( 2.795120610037679754, -0.7443816538093332991, -9.728666380661904256 ) ) ;
#25898 = SECURITY_CLASSIFICATION_LEVEL ( 'unclassified' ) ;
#25899 = CARTESIAN_POINT ( 'NONE',  ( 18.76665878146132371, -5.785509246780520698, 4.112224495634847266 ) ) ;
#25900 = CARTESIAN_POINT ( 'NONE',  ( 2.281627749324420140, -0.2935656086769634077, -1.757435426329174710 ) ) ;
#25902 = CARTESIAN_POINT ( 'NONE',  ( 6.524595623740806261, 7.015943501182391628, 5.074779492939314629 ) ) ;
#25901 = CARTESIAN_POINT ( 'NONE',  ( 7.249760686538667009, -6.139290821770289064, 5.151476664237455871 ) ) ;
#25903 = EDGE_CURVE ( 'NONE', #24091, #7488, #16380, .T. ) ;
#25904 = ORIENTED_EDGE ( 'NONE', *, *, #9029, .F. ) ;
#25905 = CARTESIAN_POINT ( 'NONE',  ( -31.91713028529358098, -0.0003384977252905707612, 2.028141679950118625 ) ) ;
#25906 = CARTESIAN_POINT ( 'NONE',  ( 10.57125986779756843, -0.8254815157534942660, -4.681538312723525053 ) ) ;
#25907 = CARTESIAN_POINT ( 'NONE',  ( 3.499999999999999556, -2.834406817834851378, -8.013497238472808704 ) ) ;
#25908 = EDGE_CURVE ( 'NONE', #5049, #32842, #3058, .T. ) ;
#25910 = EDGE_LOOP ( 'NONE', ( #16570, #13059, #12422, #2567, #12869 ) ) ;
#25909 = DIRECTION ( 'NONE',  ( 0.000000000000000000, 0.000000000000000000, 1.000000000000000000 ) ) ;
#25911 = AXIS2_PLACEMENT_3D ( 'NONE', #19610, #7552, #12083 ) ;
#25912 = CARTESIAN_POINT ( 'NONE',  ( -5.412550801365593856, 3.368539882008727115, 1.828967928396026954 ) ) ;
#25914 = EDGE_CURVE ( 'NONE', #72, #15174, #1261, .T. ) ;
#25913 = DIRECTION ( 'NONE',  ( -0.000000000000000000, -0.9063077870366467170, -0.4226182617407066577 ) ) ;
#25915 = VERTEX_POINT ( 'NONE', #1185 ) ;
#25916 = ORIENTED_EDGE ( 'NONE', *, *, #23692, .T. ) ;
#25917 = CARTESIAN_POINT ( 'NONE',  ( 23.81423349025420322, -17.27971345279105719, -1.410233427488536417 ) ) ;
#25918 = CARTESIAN_POINT ( 'NONE',  ( 7.249760686538667009, -6.940565734314625423, 4.007137495034787555 ) ) ;
#25919 = VERTEX_POINT ( 'NONE', #31445 ) ;
#25920 = EDGE_CURVE ( 'NONE', #19637, #30369, #30571, .T. ) ;
#25921 = CARTESIAN_POINT ( 'NONE',  ( 21.17250000136559507, -3.024605502323851169, 0.3178988483021052969 ) ) ;
#25922 = CARTESIAN_POINT ( 'NONE',  ( 3.063284526839889388, 2.223716399045570391, 8.461683424509315543 ) ) ;
#25923 = CARTESIAN_POINT ( 'NONE',  ( 2.274274201625319236, -9.680994141368833183, 5.222868219166820758 ) ) ;
#25924 = B_SPLINE_CURVE_WITH_KNOTS ( 'NONE', 3,
 ( #11350, #16685, #4004, #11835, #21553, #31763, #8836, #32073 ),
 .UNSPECIFIED., .F., .F.,
 ( 4, 2, 2, 4 ),
 ( -5.999999999462396917E-08, 0.0004626438357226977461, 0.0006939957535840434594, 0.0009253476714453893895 ),
 .UNSPECIFIED. ) ;
#25925 = EDGE_CURVE ( 'NONE', #22609, #19221, #9166, .T. ) ;
#25926 = CARTESIAN_POINT ( 'NONE',  ( 102.5401559989745408, -5.675509796545467722, 0.8105616764185750167 ) ) ;
#25927 = ORIENTED_EDGE ( 'NONE', *, *, #15920, .F. ) ;
#25928 = EDGE_CURVE ( 'NONE', #22995, #4279, #29451, .T. ) ;
#25929 = PERSON_AND_ORGANIZATION ( #6766, #25292 ) ;
#25930 = DIRECTION ( 'NONE',  ( 0.4999999999999967804, 0.8660254037844404840, 1.001543065824777131E-14 ) ) ;
#25931 = ORIENTED_EDGE ( 'NONE', *, *, #6222, .F. ) ;
#25932 = EDGE_CURVE ( 'NONE', #15255, #29122, #658, .T. ) ;
#25933 = CARTESIAN_POINT ( 'NONE',  ( 14.29295439700192993, -14.14386588685529489, -1.000000000000000000 ) ) ;
#25934 = VERTEX_POINT ( 'NONE', #13365 ) ;
#25935 = CARTESIAN_POINT ( 'NONE',  ( -22.63686929475232645, 4.062439337332850897, 2.144399907006354855 ) ) ;
#25936 = EDGE_CURVE ( 'NONE', #32347, #19255, #20418, .T. ) ;
#25938 = EDGE_LOOP ( 'NONE', ( #28030, #23770 ) ) ;
#25937 = CARTESIAN_POINT ( 'NONE',  ( 18.85676753365875413, -4.778274243329593496, -4.053847714192347240 ) ) ;
#25939 = ORIENTED_EDGE ( 'NONE', *, *, #31935, .F. ) ;
#25940 = LINE ( 'NONE', #26580, #7641 ) ;
#25941 = CARTESIAN_POINT ( 'NONE',  ( 5.377543748152550762, -7.530955069117533540, 2.741043480754901118 ) ) ;
#25942 = DIRECTION ( 'NONE',  ( -4.917867153433028611E-17, -0.5735764363510496011, 0.8191520442889893561 ) ) ;
#25944 = EDGE_LOOP ( 'NONE', ( #15874, #17501, #8980, #33034 ) ) ;
#25943 = CARTESIAN_POINT ( 'NONE',  ( -33.81874022276151237, 19.50000000000000000, -1.818740222761503045 ) ) ;
#25945 = FACE_OUTER_BOUND ( 'NONE', #26679, .T. ) ;
#25946 = CARTESIAN_POINT ( 'NONE',  ( 8.930755659325141593, 0.5000000000000008882, 1.500000000000000000 ) ) ;
#25947 = CARTESIAN_POINT ( 'NONE',  ( -4.154891947659814733, -6.512605193776770385, 1.745058689288190523 ) ) ;
#25949 = EDGE_CURVE ( 'NONE', #31647, #25934, #23683, .T. ) ;
#25948 = CARTESIAN_POINT ( 'NONE',  ( 22.11000000136559507, -3.156283516753370044, -0.9349337715887220401 ) ) ;
#25950 = DIRECTION ( 'NONE',  ( 0.000000000000000000, 1.000000000000000000, 0.000000000000000000 ) ) ;
#25952 = ORIENTED_EDGE ( 'NONE', *, *, #14642, .F. ) ;
#25951 = DIRECTION ( 'NONE',  ( 0.000000000000000000, 0.000000000000000000, 1.000000000000000000 ) ) ;
#25953 = ADVANCED_FACE ( 'NONE', ( #6342, #19566 ), #14704, .T. ) ;
#25954 = DIRECTION ( 'NONE',  ( 0.000000000000000000, -0.03489949670250135777, -0.9993908270190957621 ) ) ;
#25955 = B_SPLINE_CURVE_WITH_KNOTS ( 'NONE', 3,
 ( #20213, #2002, #24726, #30409, #9851, #5015, #25396, #2505, #14692, #27410 ),
 .UNSPECIFIED., .F., .F.,
 ( 4, 2, 2, 2, 4 ),
 ( 3.512955446118267852E-07, 0.0005479535487287104769, 0.001095555801912809170, 0.001643158055096907971, 0.002190760308281006555 ),
 .UNSPECIFIED. ) ;
#25956 = CARTESIAN_POINT ( 'NONE',  ( -26.59846049200615781, 17.65632644948022190, 1.792369863739132985 ) ) ;
#25957 = CARTESIAN_POINT ( 'NONE',  ( 20.79750000136559507, 0.3178988483021036315, 3.024605502323848949 ) ) ;
#25958 = EDGE_CURVE ( 'NONE', #3558, #31165, #24395, .T. ) ;
#25959 = CARTESIAN_POINT ( 'NONE',  ( 0.000000000000000000, -10.76487093102063319, -1.999317321091613753 ) ) ;
#25960 = CARTESIAN_POINT ( 'NONE',  ( 109.6329156864505165, 19.01855260168436246, 4.629213727441584325 ) ) ;
#25961 = CARTESIAN_POINT ( 'NONE',  ( 68.71221462756291487, -6.131929330199175077, 3.993435576830336231 ) ) ;
#25962 = ORIENTED_EDGE ( 'NONE', *, *, #16311, .T. ) ;
#25963 = DIRECTION ( 'NONE',  ( 1.000000000000000000, -8.574039729943018344E-17, -0.000000000000000000 ) ) ;
#25964 = CARTESIAN_POINT ( 'NONE',  ( -12.44989959798873791, 0.000000000000000000, -12.99999999999999645 ) ) ;
#25965 = ORIENTED_EDGE ( 'NONE', *, *, #26107, .T. ) ;
#25966 = EDGE_CURVE ( 'NONE', #31776, #19663, #19225, .T. ) ;
#25967 = CC_DESIGN_PERSON_AND_ORGANIZATION_ASSIGNMENT ( #7798, #30726, ( #1824 ) ) ;
#25968 = CARTESIAN_POINT ( 'NONE',  ( 2.866494652520772846, -9.241976615239517301, 2.300561732649529123 ) ) ;
#25969 = DIRECTION ( 'NONE',  ( 0.1437473352845037022, 0.000000000000000000, -0.9896144216807900573 ) ) ;
#25970 = CARTESIAN_POINT ( 'NONE',  ( 5.489343555808772201, -8.118190043691528857, 0.1039150536218743925 ) ) ;
#25972 = CARTESIAN_POINT ( 'NONE',  ( 107.9565509429370849, -17.44370650368591313, 4.757555836516734082 ) ) ;
#25971 = CARTESIAN_POINT ( 'NONE',  ( 20.66455810932185955, -16.14294586248262320, 1.000000000000000000 ) ) ;
#25973 = ORIENTED_EDGE ( 'NONE', *, *, #21231, .F. ) ;
#25974 = CARTESIAN_POINT ( 'NONE',  ( 4.749760686538667009, 4.007137495034812424, 6.940565734314612101 ) ) ;
#25975 = ORIENTED_EDGE ( 'NONE', *, *, #22719, .F. ) ;
#25976 = CARTESIAN_POINT ( 'NONE',  ( 102.9361373302715918, -5.944196040818414239, 2.713652344655544724 ) ) ;
#25978 = ORIENTED_EDGE ( 'NONE', *, *, #4476, .T. ) ;
#25977 = LINE ( 'NONE', #3569, #23478 ) ;
#25979 = ORIENTED_EDGE ( 'NONE', *, *, #3941, .T. ) ;
#25980 = CARTESIAN_POINT ( 'NONE',  ( 85.38119660045754244, -6.034158634414237277, -4.522129901861164036 ) ) ;
#25981 = EDGE_CURVE ( 'NONE', #22947, #25870, #21733, .T. ) ;
#25982 = CARTESIAN_POINT ( 'NONE',  ( 7.249760686538667009, -7.892520144992443143, 1.391664247347202288 ) ) ;
#25984 = ORIENTED_EDGE ( 'NONE', *, *, #26141, .T. ) ;
#25983 = CARTESIAN_POINT ( 'NONE',  ( 18.92762145840779553, -3.986269566730710867, 2.784837724132013026 ) ) ;
#25985 = ORIENTED_EDGE ( 'NONE', *, *, #9549, .T. ) ;
#25986 = LINE ( 'NONE', #30852, #19193 ) ;
#25987 = B_SPLINE_CURVE_WITH_KNOTS ( 'NONE', 3,
 ( #348, #5681, #13335, #13516, #20735, #15532, #10521, #8348 ),
 .UNSPECIFIED., .F., .F.,
 ( 4, 2, 2, 4 ),
 ( 5.099451029802972801E-07, 0.001229189612685836199, 0.001843529446477266400, 0.002457869280268696818 ),
 .UNSPECIFIED. ) ;
#25988 = DIRECTION ( 'NONE',  ( -0.000000000000000000, -0.000000000000000000, -1.000000000000000000 ) ) ;
#25989 = ADVANCED_FACE ( 'NONE', ( #11870 ), #9507, .T. ) ;
#25990 = CARTESIAN_POINT ( 'NONE',  ( 0.2409471776115469921, 0.000000000000000000, -5.396302277755718357 ) ) ;
#25991 = CARTESIAN_POINT ( 'NONE',  ( 0.000000000000000000, -6.700937042937072263, 2.183447440113167826 ) ) ;
#25992 = CARTESIAN_POINT ( 'NONE',  ( 107.8981067246555625, -16.60212429951632629, 1.900353104894979772 ) ) ;
#25993 = CARTESIAN_POINT ( 'NONE',  ( -8.000050800000000351, 0.3588475416126519768, -3.414206294404568798 ) ) ;
#25994 = CARTESIAN_POINT ( 'NONE',  ( 1.449903671498899538, -2.780906680908541873, 1.499999999999999112 ) ) ;
#25995 = DIRECTION ( 'NONE',  ( -0.000000000000000000, -0.000000000000000000, -1.000000000000000000 ) ) ;
#25996 = EDGE_CURVE ( 'NONE', #12596, #7729, #18755, .T. ) ;
#25997 = CARTESIAN_POINT ( 'NONE',  ( -3.449949199999996274, 0.000000000000000000, 0.000000000000000000 ) ) ;
#25998 = CARTESIAN_POINT ( 'NONE',  ( 2.692942092879393456, -0.02443046219423304979, 1.307625729273631077 ) ) ;
#25999 = ORIENTED_EDGE ( 'NONE', *, *, #28017, .T. ) ;
#26000 = DIRECTION ( 'NONE',  ( 2.219124775575021862E-17, 0.2588190451025318417, -0.9659258262890653146 ) ) ;
#26001 = CARTESIAN_POINT ( 'NONE',  ( 7.064423600674403225, -8.711672189282625212, -0.8180878109954319299 ) ) ;
#26002 = CARTESIAN_POINT ( 'NONE',  ( -2.330754651808319766E-16, -2.718385644597204553, 4.208382051008182856 ) ) ;
#26003 = EDGE_LOOP ( 'NONE', ( #13951, #9652, #6257, #18140, #397, #3133, #27805, #19927, #30329, #25089, #26286, #9345, #16704, #30728, #28043, #361, #9895, #14490, #18165, #14255, #2572, #24048, #9260, #31356, #24883, #19627, #296, #23186, #7377, #23894, #13607, #149, #29763, #24934, #13355, #29821, #26743, #19781, #15172, #31331, #31846, #10038, #3679, #13923, #20700, #30879, #9075, #28775, #4194, #10476, #28072, #7196, #28394, #32463, #20365, #18096, #29596, #6135, #27282, #26570, #30464, #24716, #22599, #15224, #28146, #26350, #5811, #14687, #24922, #30715, #959, #8443, #11980, #32359, #14635, #31168, #4482, #13217, #14194, #11599, #17295, #29324, #11379, #23777, #18172, #22108, #18938, #732, #19503, #23381, #8525, #5161, #18362, #22497, #27910, #22722, #18963, #10605, #8071, #17068, #10080, #9351, #6552, #11251, #16707, #16563, #11051, #29456 ) ) ;
#26004 = CARTESIAN_POINT ( 'NONE',  ( 23.67250000136559507, 3.024605502323846729, -0.3178988483021056854 ) ) ;
#26005 = ADVANCED_FACE ( 'NONE', ( #32295 ), #16718, .T. ) ;
#26006 = APPROVAL ( #23557, 'UNSPECIFIED' ) ;
#26007 = CARTESIAN_POINT ( 'NONE',  ( -2.400050802731187094, -3.113457007523259268, 0.9222479816126455399 ) ) ;
#26008 = CARTESIAN_POINT ( 'NONE',  ( 18.70218739254009677, -21.34730519116027025, -1.543632415226145804 ) ) ;
#26009 = ORIENTED_EDGE ( 'NONE', *, *, #22639, .T. ) ;
#26010 = CARTESIAN_POINT ( 'NONE',  ( 18.85511084201081289, -4.796792731029945855, -4.091315477141356460 ) ) ;
#26011 = VERTEX_POINT ( 'NONE', #8860 ) ;
#26012 = CARTESIAN_POINT ( 'NONE',  ( 85.10544820223228157, -1.573551533641234901, -1.915219082070890755 ) ) ;
#26013 = PERSON_AND_ORGANIZATION ( #13161, #1318 ) ;
#26015 = EDGE_LOOP ( 'NONE', ( #1882, #25531, #26642, #12781 ) ) ;
#26014 = CARTESIAN_POINT ( 'NONE',  ( 10.00000000000000178, -8.574039729943018837E-16, 0.000000000000000000 ) ) ;
#26016 = ORIENTED_EDGE ( 'NONE', *, *, #27973, .T. ) ;
#26017 = CARTESIAN_POINT ( 'NONE',  ( 0.4008809018342579522, 9.770170320898831307, 2.274078661686000924 ) ) ;
#26018 = EDGE_CURVE ( 'NONE', #14768, #14212, #21889, .T. ) ;
#26019 = VERTEX_POINT ( 'NONE', #17219 ) ;
#26020 = DIRECTION ( 'NONE',  ( -0.000000000000000000, -0.000000000000000000, -1.000000000000000000 ) ) ;
#26022 = ORIENTED_EDGE ( 'NONE', *, *, #14539, .T. ) ;
#26021 = CARTESIAN_POINT ( 'NONE',  ( 35.34133959476921660, -3.844168172129591277, -0.8105616794546218751 ) ) ;
#26023 = CARTESIAN_POINT ( 'NONE',  ( 9.910042481050302499, 1.133699783719172016, 1.049999999999999600 ) ) ;
#26024 = DIRECTION ( 'NONE',  ( -8.541412920197222280E-17, -0.9961946980917457672, 0.08715574274765533480 ) ) ;
#26025 = EDGE_CURVE ( 'NONE', #27447, #13727, #11538, .T. ) ;
#26026 = FACE_OUTER_BOUND ( 'NONE', #17728, .T. ) ;
#26027 = LINE ( 'NONE', #12980, #26337 ) ;
#26028 = ORIENTED_EDGE ( 'NONE', *, *, #22495, .T. ) ;
#26029 =( BOUNDED_CURVE ( )  B_SPLINE_CURVE ( 2, ( #5878, #3408, #3082, #6063, #8880, #3228, #16066, #16253, #28782, #23438, #23926 ),
 .UNSPECIFIED., .F., .F. ) 
 B_SPLINE_CURVE_WITH_KNOTS ( ( 3, 2, 2, 2, 2, 3 ),
 ( 0.5603822619934377691, 0.5625000000000000000, 0.5781250000000000000, 0.5937500000000000000, 0.6093750000000000000, 0.6228822619934377691 ),
 .UNSPECIFIED. ) 
 CURVE ( )  GEOMETRIC_REPRESENTATION_ITEM ( )  RATIONAL_B_SPLINE_CURVE ( ( 0.9821626249036861100, 0.9896829947469995004, 1.000000000000000000, 0.9238795325112867385, 1.000000000000000000, 0.9238795325112867385, 1.000000000000000000, 0.9238795325112867385, 1.000000000000000000, 0.9341965377642872381, 0.9821626249036861100 ) ) 
 REPRESENTATION_ITEM ( '' )  );
#26030 = DIRECTION ( 'NONE',  ( -0.8251117619019970872, 0.5649695393302031077, 0.000000000000000000 ) ) ;
#26031 = DIRECTION ( 'NONE',  ( 8.678904333908113252E-16, 0.000000000000000000, -1.000000000000000000 ) ) ;
#26032 = CARTESIAN_POINT ( 'NONE',  ( 29.19739603781543025, -7.896110766395437963, -1.873788768280044925 ) ) ;
#26033 = CARTESIAN_POINT ( 'NONE',  ( 3.822634483660907761E-16, 4.458382051008192626, 2.285372942704970267 ) ) ;
#26034 = CARTESIAN_POINT ( 'NONE',  ( -15.51216819290874227, -25.44850941282521006, 1.500000000000000000 ) ) ;
#26035 = CARTESIAN_POINT ( 'NONE',  ( 23.22234548918896380, -21.93639154399404489, 1.104776513122921022 ) ) ;
#26036 = CARTESIAN_POINT ( 'NONE',  ( 22.99290772595112387, -0.1310194482076047495, -2.499999999999998668 ) ) ;
#26037 = LINE ( 'NONE', #2998, #141 ) ;
#26038 = B_SPLINE_CURVE_WITH_KNOTS ( 'NONE', 3,
 ( #28392, #2344, #7989, #15695 ),
 .UNSPECIFIED., .F., .F.,
 ( 4, 4 ),
 ( 0.005732069968871193570, 0.4737525964755946450 ),
 .UNSPECIFIED. ) ;
#26039 = CARTESIAN_POINT ( 'NONE',  ( -2.762550801365593500, -2.752080473201636845, 2.228590825266444586 ) ) ;
#26040 = ORIENTED_EDGE ( 'NONE', *, *, #8345, .T. ) ;
#26041 = B_SPLINE_CURVE_WITH_KNOTS ( 'NONE', 3,
 ( #1471, #32055, #6458, #3991, #24355, #24503, #11329, #11647, #31747, #14305 ),
 .UNSPECIFIED., .F., .F.,
 ( 4, 2, 2, 2, 4 ),
 ( 2.740849916258459394E-07, 0.0005478761651001745094, 0.001095478245208723325, 0.001643080325317272140, 0.002190682405425820739 ),
 .UNSPECIFIED. ) ;
#26042 = CARTESIAN_POINT ( 'NONE',  ( -3.604531657079157903, 2.325406398514293205, -1.883076972206379374 ) ) ;
#26043 = CARTESIAN_POINT ( 'NONE',  ( 15.28872660057388799, 20.76088595412472060, -4.612695725900422872 ) ) ;
#26044 = FACE_OUTER_BOUND ( 'NONE', #12247, .T. ) ;
#26045 = CARTESIAN_POINT ( 'NONE',  ( 23.15368348421776901, -16.86203458153667256, 1.000000000000138778 ) ) ;
#26046 = ORIENTED_EDGE ( 'NONE', *, *, #25551, .T. ) ;
#26047 = CARTESIAN_POINT ( 'NONE',  ( 84.94207106226485848, -3.684213880882921899, -3.390607676403233128 ) ) ;
#26048 = ORIENTED_EDGE ( 'NONE', *, *, #19705, .F. ) ;
#26049 = DIRECTION ( 'NONE',  ( -1.000000000000000000, 0.000000000000000000, 0.000000000000000000 ) ) ;
#26050 = PERSON_AND_ORGANIZATION_ROLE ( 'creator' ) ;
#26051 = CARTESIAN_POINT ( 'NONE',  ( 85.03413872134471774, -5.177407751507606903, 4.033869228796232775 ) ) ;
#26052 = EDGE_CURVE ( 'NONE', #10585, #9751, #24199, .T. ) ;
#26053 = EDGE_CURVE ( 'NONE', #10466, #112, #24553, .T. ) ;
#26054 = PLANE ( 'NONE',  #10706 ) ;
#26056 = CARTESIAN_POINT ( 'NONE',  ( 6.883866557622099869, 8.415306967752711031, -2.328663417917355982 ) ) ;
#26055 = DIRECTION ( 'NONE',  ( -0.000000000000000000, 0.9961946980917454342, 0.08715574274765873486 ) ) ;
#26057 = ORIENTED_EDGE ( 'NONE', *, *, #24714, .T. ) ;
#26058 = CARTESIAN_POINT ( 'NONE',  ( -3.690938403952409329E-13, 7.533794289458907834, 7.944914065997345176 ) ) ;
#26059 = CARTESIAN_POINT ( 'NONE',  ( 3.499999999999999556, 5.471841788314750765, -3.018103451449674068 ) ) ;
#26060 = CARTESIAN_POINT ( 'NONE',  ( 2.274274201625316572, -7.958834565716716547, -7.593217523260693547 ) ) ;
#26062 = ORIENTED_EDGE ( 'NONE', *, *, #11202, .F. ) ;
#26061 = CARTESIAN_POINT ( 'NONE',  ( 108.3190036904951796, 19.95449834640353259, -1.980516148027076984 ) ) ;
#26063 = CARTESIAN_POINT ( 'NONE',  ( -4.512550801365592612, 1.088641768524161613, 3.675193018007247403 ) ) ;
#26064 = CARTESIAN_POINT ( 'NONE',  ( 108.1382411484322290, 18.94794118670416694, 4.145841387855481841 ) ) ;
#26065 = CARTESIAN_POINT ( 'NONE',  ( 7.249760686538667009, 2.741043480755029016, -7.530955069117485579 ) ) ;
#26066 = ORIENTED_EDGE ( 'NONE', *, *, #11231, .F. ) ;
#26067 = ORIENTED_EDGE ( 'NONE', *, *, #12990, .T. ) ;
#26068 = CARTESIAN_POINT ( 'NONE',  ( 7.249760686538667009, -7.530955069117533540, 2.741043480754901118 ) ) ;
#26069 = DIRECTION ( 'NONE',  ( 1.000000000000000000, -0.000000000000000000, -0.000000000000000000 ) ) ;
#26070 = ORIENTED_EDGE ( 'NONE', *, *, #19818, .F. ) ;
#26071 = CARTESIAN_POINT ( 'NONE',  ( 2.274274201627287884, 5.222868219167418502, -9.680994141364108074 ) ) ;
#26072 = CARTESIAN_POINT ( 'NONE',  ( 3.249999999999999556, -7.360373001730883047, -4.729683950898953881 ) ) ;
#26073 = CARTESIAN_POINT ( 'NONE',  ( 47.68482864957484679, -3.825617316378891797, -0.07017451552781625579 ) ) ;
#26074 = CARTESIAN_POINT ( 'NONE',  ( 3.381541507458994289, -0.06919447570412250170, -1.261810069052565986 ) ) ;
#26075 = DIRECTION ( 'NONE',  ( 1.000000000000000000, 0.000000000000000000, 0.000000000000000000 ) ) ;
#26076 = ORIENTED_EDGE ( 'NONE', *, *, #5808, .F. ) ;
#26077 = DIRECTION ( 'NONE',  ( 1.000000000000000000, 0.000000000000000000, 0.000000000000000000 ) ) ;
#26078 = EDGE_CURVE ( 'NONE', #13143, #9106, #11691, .T. ) ;
#26079 = ORIENTED_EDGE ( 'NONE', *, *, #12240, .T. ) ;
#26080 = DATE_AND_TIME ( #11178, #21029 ) ;
#26081 = CARTESIAN_POINT ( 'NONE',  ( 101.9216173105994585, -5.769792427975423799, -0.4426577264581311733 ) ) ;
#26082 = VERTEX_POINT ( 'NONE', #9181 ) ;
#26083 = CARTESIAN_POINT ( 'NONE',  ( 107.5147077154356623, 18.30459826903478771, -4.398253369385427547 ) ) ;
#26084 = ORIENTED_EDGE ( 'NONE', *, *, #6947, .T. ) ;
#26085 = CYLINDRICAL_SURFACE ( 'NONE', #11902, 5.100000000000000533 ) ;
#26087 = ORIENTED_EDGE ( 'NONE', *, *, #8186, .F. ) ;
#26086 = CARTESIAN_POINT ( 'NONE',  ( 54.95033023691122764, -5.534837039125057423, -4.185347662766374377 ) ) ;
#26088 = ADVANCED_FACE ( 'NONE', ( #4030 ), #1305, .T. ) ;
#26089 = EDGE_LOOP ( 'NONE', ( #31813, #1986, #16903, #14645, #673 ) ) ;
#26090 = DIRECTION ( 'NONE',  ( 0.000000000000000000, 0.000000000000000000, -1.000000000000000000 ) ) ;
#26091 = CARTESIAN_POINT ( 'NONE',  ( -3.462550801365593678, -3.521866450007987037, -0.3701630799359323931 ) ) ;
#26092 = CARTESIAN_POINT ( 'NONE',  ( 7.189332377417184006, -9.531173777829009097, 1.500000000000000000 ) ) ;
#26093 = DIRECTION ( 'NONE',  ( 1.000000000000000000, -0.000000000000000000, -0.000000000000000000 ) ) ;
#26095 = ORIENTED_EDGE ( 'NONE', *, *, #14674, .T. ) ;
#26094 = CARTESIAN_POINT ( 'NONE',  ( -15.12340757463330476, -27.93932300454937590, -0.9999999999999997780 ) ) ;
#26096 = CARTESIAN_POINT ( 'NONE',  ( 11.04311965146451158, 15.00000000000000178, 1.508259000770581615 ) ) ;
#26097 = CARTESIAN_POINT ( 'NONE',  ( 13.86820177083861871, 7.731989999893393417, 1.050000000000000044 ) ) ;
#26098 = EDGE_CURVE ( 'NONE', #12815, #28083, #28492, .T. ) ;
#26099 = CARTESIAN_POINT ( 'NONE',  ( -0.1325319112326446558, -14.88632472074928081, 1.499999999999681366 ) ) ;
#26100 = CARTESIAN_POINT ( 'NONE',  ( -29.24402871571405882, 0.000000000000000000, 11.50000000000000000 ) ) ;
#26101 = CARTESIAN_POINT ( 'NONE',  ( 3.569153896158649530, -0.01695480042954938815, 1.144240241240434663 ) ) ;
#26103 = ORIENTED_EDGE ( 'NONE', *, *, #9855, .T. ) ;
#26102 = CARTESIAN_POINT ( 'NONE',  ( 23.85324836636559453, -17.43424264171722982, 1.580747861890658745 ) ) ;
#26104 = CARTESIAN_POINT ( 'NONE',  ( 5.377543748152548986, -1.391664247347174754, -7.892520144992448472 ) ) ;
#26105 = CARTESIAN_POINT ( 'NONE',  ( -31.15578486440642436, -25.44239456788696785, 1.499999999999999778 ) ) ;
#26106 = CARTESIAN_POINT ( 'NONE',  ( 22.61000000136559507, 3.156283516753366047, 0.9349337715887203748 ) ) ;
#26107 = EDGE_CURVE ( 'NONE', #32817, #25210, #28413, .T. ) ;
#26108 = CARTESIAN_POINT ( 'NONE',  ( -20.31068713123109859, 5.033963319883215881, 1.500000000000000000 ) ) ;
#26109 = CARTESIAN_POINT ( 'NONE',  ( 101.8408884992664980, -4.607317627582337316, -3.084862410648784969 ) ) ;
#26110 = DIRECTION ( 'NONE',  ( 0.9816271834476637537, 0.000000000000000000, 0.1908089953765453872 ) ) ;
#26111 = CARTESIAN_POINT ( 'NONE',  ( 108.0291781248179177, -18.48951985539285658, 4.325670280512381005 ) ) ;
#26112 = AXIS2_PLACEMENT_3D ( 'NONE', #23828, #940, #10627 ) ;
#26113 = EDGE_CURVE ( 'NONE', #15269, #1202, #9482, .T. ) ;
#26114 = CARTESIAN_POINT ( 'NONE',  ( -23.35000000000000142, -10.96966150227469505, -11.09540449768827308 ) ) ;
#26115 = ORIENTED_EDGE ( 'NONE', *, *, #15116, .F. ) ;
#26116 = CARTESIAN_POINT ( 'NONE',  ( 25.55210404927549916, 2.101042102276441170, 1.904186784126992604 ) ) ;
#26117 = DIRECTION ( 'NONE',  ( -1.000000000000000000, 0.000000000000000000, 0.000000000000000000 ) ) ;
#26118 = EDGE_CURVE ( 'NONE', #13402, #4337, #983, .T. ) ;
#26119 = CARTESIAN_POINT ( 'NONE',  ( 107.9618353151786181, 20.81780380167319677, 0.000000000000000000 ) ) ;
#26121 = CARTESIAN_POINT ( 'NONE',  ( 108.0076953296759683, -18.18017294959541630, 4.637765880993337753 ) ) ;
#26120 = CARTESIAN_POINT ( 'NONE',  ( 7.249760686538667009, 6.940565734314597002, 4.007137495034836405 ) ) ;
#26122 = EDGE_CURVE ( 'NONE', #19255, #1082, #16193, .T. ) ;
#26123 = ORIENTED_EDGE ( 'NONE', *, *, #32089, .F. ) ;
#26124 = B_SPLINE_CURVE_WITH_KNOTS ( 'NONE', 3,
 ( #9781, #30350, #7421, #27825, #2767, #32872, #12762, #15287, #17808, #22968 ),
 .UNSPECIFIED., .F., .F.,
 ( 4, 2, 2, 2, 4 ),
 ( 3.032460776715785715E-07, 0.0005479053915603962011, 0.001095507537043120816, 0.001643109682525845322, 0.002190711828008569829 ),
 .UNSPECIFIED. ) ;
#26125 = DIRECTION ( 'NONE',  ( 0.000000000000000000, 0.000000000000000000, -1.000000000000000000 ) ) ;
#26126 = ORIENTED_EDGE ( 'NONE', *, *, #28624, .T. ) ;
#26127 = DIRECTION ( 'NONE',  ( -1.000000000000000000, -0.000000000000000000, -0.000000000000000000 ) ) ;
#26129 = VERTEX_POINT ( 'NONE', #5526 ) ;
#26128 = CARTESIAN_POINT ( 'NONE',  ( 0.000000000000000000, 6.807171995660584507, 6.478011392632914145 ) ) ;
#26130 = VERTEX_POINT ( 'NONE', #3028 ) ;
#26131 = CARTESIAN_POINT ( 'NONE',  ( 102.9361373302715918, -5.944196040818415128, -2.713652344655543391 ) ) ;
#26132 = DIRECTION ( 'NONE',  ( 1.000000000000000000, 0.000000000000000000, 0.000000000000000000 ) ) ;
#26134 = VERTEX_POINT ( 'NONE', #31574 ) ;
#26133 = DIRECTION ( 'NONE',  ( -0.000000000000000000, -0.000000000000000000, -1.000000000000000000 ) ) ;
#26135 = ORIENTED_EDGE ( 'NONE', *, *, #21114, .T. ) ;
#26136 = DIRECTION ( 'NONE',  ( -1.000000000000000000, 0.000000000000000000, 0.000000000000000000 ) ) ;
#26137 = CARTESIAN_POINT ( 'NONE',  ( 25.23499999999999943, -2.208672634433321348E-15, 0.000000000000000000 ) ) ;
#26138 = FACE_OUTER_BOUND ( 'NONE', #33043, .T. ) ;
#26139 = CARTESIAN_POINT ( 'NONE',  ( 107.4495515710665359, -17.35288078708288140, -4.502149265236362830 ) ) ;
#26140 = CARTESIAN_POINT ( 'NONE',  ( 101.6022419886208468, -1.170867242066747638, 0.4426577264886745189 ) ) ;
#26141 = EDGE_CURVE ( 'NONE', #24949, #21127, #22621, .T. ) ;
#26142 = AXIS2_PLACEMENT_3D ( 'NONE', #17598, #15415, #22949 ) ;
#26143 = CARTESIAN_POINT ( 'NONE',  ( 107.5617723795401872, -18.98359893170738744, -4.522129901861166701 ) ) ;
#26144 = CARTESIAN_POINT ( 'NONE',  ( 4.959216681210401489, -12.47312135805140088, 1.500000000000000666 ) ) ;
#26145 = CARTESIAN_POINT ( 'NONE',  ( 29.21679767122600069, -7.327048195461536295, 2.787782193693228994 ) ) ;
#26146 = CARTESIAN_POINT ( 'NONE',  ( 2.274274201625327230, 9.680994141368847394, -5.222868219166750592 ) ) ;
#26147 = CARTESIAN_POINT ( 'NONE',  ( 10.56870887191539587, 4.467071865485493731, -1.625881193364653088 ) ) ;
#26148 = AXIS2_PLACEMENT_3D ( 'NONE', #6915, #17303, #1765 ) ;
#26149 = ORIENTED_EDGE ( 'NONE', *, *, #21253, .T. ) ;
#26150 = DIRECTION ( 'NONE',  ( 1.000000000000000000, -0.000000000000000000, -0.000000000000000000 ) ) ;
#26151 =( REPRESENTATION_RELATIONSHIP ('NONE','NONE', #1085, #27351 ) REPRESENTATION_RELATIONSHIP_WITH_TRANSFORMATION ( #17330 )SHAPE_REPRESENTATION_RELATIONSHIP( ) );
#26152 = CARTESIAN_POINT ( 'NONE',  ( 29.38825086720287771, -3.456623792456554156, 2.713652344655542503 ) ) ;
#26153 = EDGE_CURVE ( 'NONE', #1139, #12534, #11532, .T. ) ;
#26154 = CARTESIAN_POINT ( 'NONE',  ( 10.00000000000000178, 4.787500056513387392, -1.476463073999587872 ) ) ;
#26155 = ORIENTED_EDGE ( 'NONE', *, *, #4921, .T. ) ;
#26156 = CARTESIAN_POINT ( 'NONE',  ( 24.86000000136559862, 1.570731468192929858, 2.892927487894329186 ) ) ;
#26157 = LINE ( 'NONE', #28520, #12488 ) ;
#26158 = EDGE_CURVE ( 'NONE', #27483, #18153, #21023, .T. ) ;
#26159 = CARTESIAN_POINT ( 'NONE',  ( 18.74274612900900294, -21.25842652921760489, -1.734019191250015357 ) ) ;
#26160 = EDGE_LOOP ( 'NONE', ( #31239, #17674, #2937, #15339 ) ) ;
#26161 = CARTESIAN_POINT ( 'NONE',  ( 4.290242492657217039E-16, 5.003758587302148619, -0.2499999999999991951 ) ) ;
#26162 = ADVANCED_FACE ( 'NONE', ( #5823 ), #11163, .F. ) ;
#26163 = CIRCLE ( 'NONE', #23477, 2.999999999999999556 ) ;
#26164 = AXIS2_PLACEMENT_3D ( 'NONE', #15465, #30733, #28036 ) ;
#26165 = ORIENTED_EDGE ( 'NONE', *, *, #30556, .F. ) ;
#26166 = DIRECTION ( 'NONE',  ( 0.000000000000000000, 0.000000000000000000, 1.000000000000000000 ) ) ;
#26167 = APPROVAL_DATE_TIME ( #26501, #16528 ) ;
#26169 = ORIENTED_EDGE ( 'NONE', *, *, #14859, .F. ) ;
#26168 = CARTESIAN_POINT ( 'NONE',  ( -4.176822952888146645, -3.225712836239801096, -0.9788672205760856615 ) ) ;
#26170 = ORIENTED_EDGE ( 'NONE', *, *, #7251, .F. ) ;
#26171 = CARTESIAN_POINT ( 'NONE',  ( 24.48500000136559507, 2.892927487894327410, -1.570731468192931635 ) ) ;
#26172 = ORIENTED_EDGE ( 'NONE', *, *, #9943, .T. ) ;
#26173 = AXIS2_PLACEMENT_3D ( 'NONE', #18288, #31186, #13109 ) ;
#26174 = CARTESIAN_POINT ( 'NONE',  ( 5.377543748152548098, 8.385837730238846314E-14, -8.014274990069656823 ) ) ;
#26176 = ORIENTED_EDGE ( 'NONE', *, *, #3209, .T. ) ;
#26175 = CARTESIAN_POINT ( 'NONE',  ( 84.86147853072903047, -2.382337935102287307, -0.8105612886928852401 ) ) ;
#26177 = CARTESIAN_POINT ( 'NONE',  ( 16.42946203030704311, 11.64644840300599959, 1.049999999999999822 ) ) ;
#26178 = DIRECTION ( 'NONE',  ( 4.917867153433085311E-17, 0.5735764363510552633, -0.8191520442889853593 ) ) ;
#26179 = CARTESIAN_POINT ( 'NONE',  ( 3.499999999999999556, -5.233522515400055752, -4.720195129223329289 ) ) ;
#26180 = DIRECTION ( 'NONE',  ( -1.000000000000000000, 0.000000000000000000, -0.000000000000000000 ) ) ;
#26181 = ADVANCED_FACE ( 'NONE', ( #3516 ), #24021, .F. ) ;
#26182 = ORIENTED_EDGE ( 'NONE', *, *, #10140, .T. ) ;
#26183 = CC_DESIGN_PERSON_AND_ORGANIZATION_ASSIGNMENT ( #6495, #4330, ( #2027 ) ) ;
#26184 = CARTESIAN_POINT ( 'NONE',  ( 0.000000000000000000, 0.000000000000000000, 0.000000000000000000 ) ) ;
#26185 = CARTESIAN_POINT ( 'NONE',  ( 109.5084093630373729, -17.21855534384546971, -4.522129901861164925 ) ) ;
#26186 = CARTESIAN_POINT ( 'NONE',  ( 102.5330529704722125, -5.572982809271280757, -1.169950773232049102 ) ) ;
#26187 = DIRECTION ( 'NONE',  ( 0.000000000000000000, 0.000000000000000000, 1.000000000000000000 ) ) ;
#26188 = VECTOR ( 'NONE', #27029, 1000.000000000000000 ) ;
#26189 = FACE_OUTER_BOUND ( 'NONE', #30147, .T. ) ;
#26190 = CARTESIAN_POINT ( 'NONE',  ( 22.00639167669143603, -21.80013755708273848, 1.500000000000000000 ) ) ;
#26191 = CARTESIAN_POINT ( 'NONE',  ( 23.86000000000000298, 1.573300977624590313, -1.942864903642426144 ) ) ;
#26192 = CARTESIAN_POINT ( 'NONE',  ( -3.690938403952409329E-13, 7.533794289458907834, 7.944914065997345176 ) ) ;
#26193 = CIRCLE ( 'NONE', #11754, 2.999999999999999556 ) ;
#26194 = CARTESIAN_POINT ( 'NONE',  ( -25.21220230200964352, 4.362210445733495590, 1.500000000000934142 ) ) ;
#26195 = CARTESIAN_POINT ( 'NONE',  ( -3.612550801365593589, -1.828967928396026510, 3.368539882008728004 ) ) ;
#26196 = ORIENTED_EDGE ( 'NONE', *, *, #27368, .T. ) ;
#26197 = EDGE_CURVE ( 'NONE', #18045, #21273, #19422, .T. ) ;
#26198 = CARTESIAN_POINT ( 'NONE',  ( -4.354531657079157903, 3.105402419394639235, -0.9198621039125850496 ) ) ;
#26199 = AXIS2_PLACEMENT_3D ( 'NONE', #18076, #703, #10707 ) ;
#26200 = CARTESIAN_POINT ( 'NONE',  ( 16.36487458112951643, 19.37645981759113312, -4.612695725900422872 ) ) ;
#26201 = CYLINDRICAL_SURFACE ( 'NONE', #25279, 2.999999999999999112 ) ;
#26202 = CARTESIAN_POINT ( 'NONE',  ( 8.690654615650863946, -10.89241706942921084, 1.000000000000000000 ) ) ;
#26203 = ORIENTED_EDGE ( 'NONE', *, *, #32400, .T. ) ;
#26204 = DIRECTION ( 'NONE',  ( 1.000000000000000000, 0.000000000000000000, 0.000000000000000000 ) ) ;
#26205 = ORIENTED_EDGE ( 'NONE', *, *, #26240, .T. ) ;
#26206 = CARTESIAN_POINT ( 'NONE',  ( 7.249760686538667009, -6.139290821770219786, -5.151476664237539360 ) ) ;
#26207 = SHAPE_DEFINITION_REPRESENTATION ( #7355, #6656 ) ;
#26208 = CIRCLE ( 'NONE', #32632, 4.999999999999999112 ) ;
#26209 = CIRCLE ( 'NONE', #11254, 297.9387600756452912 ) ;
#26210 = CARTESIAN_POINT ( 'NONE',  ( 84.97327636560633835, -4.184508908553603135, 4.155404232685564914 ) ) ;
#26211 = CIRCLE ( 'NONE', #9625, 6.248999999999999666 ) ;
#26212 = CARTESIAN_POINT ( 'NONE',  ( 9.220089837531610044, 0.1261361023189421227, 1.391323255828233130 ) ) ;
#26213 = AXIS2_PLACEMENT_3D ( 'NONE', #9667, #6996, #22069 ) ;
#26214 = CARTESIAN_POINT ( 'NONE',  ( 6.037141879243262288, 6.770886333893425757, 5.096219216992873058 ) ) ;
#26215 = VERTEX_POINT ( 'NONE', #3658 ) ;
#26216 = LINE ( 'NONE', #28876, #21040 ) ;
#26217 = ADVANCED_FACE ( 'NONE', ( #11343 ), #28889, .T. ) ;
#26218 = CARTESIAN_POINT ( 'NONE',  ( 1.750000000000000222, 8.357095590591338663, 1.552080310331533486 ) ) ;
#26219 = CARTESIAN_POINT ( 'NONE',  ( 8.528645601772334217, -0.5000000000000011102, 1.500000000000000000 ) ) ;
#26220 = CIRCLE ( 'NONE', #32623, 3.250000000000002665 ) ;
#26222 = VERTEX_POINT ( 'NONE', #21068 ) ;
#26221 = CARTESIAN_POINT ( 'NONE',  ( 9.292339479667081292, 0.2315767011690351151, -1.048511744989948813 ) ) ;
#26223 = CARTESIAN_POINT ( 'NONE',  ( -4.312550801365593323, -3.675193018007246071, 1.088641768524163167 ) ) ;
#26224 = DIRECTION ( 'NONE',  ( -0.9896144216807899463, 0.000000000000000000, -0.1437473352845038410 ) ) ;
#26225 = CARTESIAN_POINT ( 'NONE',  ( 85.10546509785196179, -6.328795743799873641, -2.184955973843232258 ) ) ;
#26226 = ORIENTED_EDGE ( 'NONE', *, *, #21285, .T. ) ;
#26227 = EDGE_LOOP ( 'NONE', ( #1619, #21892, #26103, #22056 ) ) ;
#26228 = CARTESIAN_POINT ( 'NONE',  ( 3.499999999999999556, -5.233522515400120589, 4.720195129223259123 ) ) ;
#26229 = CARTESIAN_POINT ( 'NONE',  ( 56.97280603064898941, -277.2763395528616002, 4.629213727441584325 ) ) ;
#26230 = DIRECTION ( 'NONE',  ( 0.000000000000000000, 0.000000000000000000, 1.000000000000000000 ) ) ;
#26231 = CONICAL_SURFACE ( 'NONE', #12868, 2.099999999999997868, 1.029744258676653423 ) ;
#26232 = EDGE_CURVE ( 'NONE', #14650, #6245, #31414, .T. ) ;
#26233 = EDGE_CURVE ( 'NONE', #27498, #16275, #3345, .T. ) ;
#26234 = AXIS2_PLACEMENT_3D ( 'NONE', #27817, #28801, #13112 ) ;
#26235 = CIRCLE ( 'NONE', #28353, 3.750000000000000444 ) ;
#26236 = CARTESIAN_POINT ( 'NONE',  ( 7.249760686538667009, -4.007137495034764463, -6.940565734314639634 ) ) ;
#26237 = B_SPLINE_CURVE_WITH_KNOTS ( 'NONE', 3,
 ( #29486, #1737, #27295, #6581, #29660, #6741, #11935, #27127 ),
 .UNSPECIFIED., .F., .F.,
 ( 4, 2, 2, 4 ),
 ( 2.197717205396726239E-07, 0.001262070444981969576, 0.001892995781612684262, 0.002523921118243398730 ),
 .UNSPECIFIED. ) ;
#26238 = CARTESIAN_POINT ( 'NONE',  ( -1.841338014675546475, 0.2391638310232261089, 3.112837935894453345 ) ) ;
#26239 = AXIS2_PLACEMENT_3D ( 'NONE', #16661, #4136, #11995 ) ;
#26240 = EDGE_CURVE ( 'NONE', #12555, #32142, #10854, .T. ) ;
#26241 = CARTESIAN_POINT ( 'NONE',  ( -3.887550801365593500, 2.228590825266444142, 2.752080473201636845 ) ) ;
#26242 = CARTESIAN_POINT ( 'NONE',  ( -30.98484230743790135, -10.96966150227469328, -11.09540449768827308 ) ) ;
#26243 = CARTESIAN_POINT ( 'NONE',  ( 102.5437075123492008, -5.726773290143887252, 0.4367666012699079059 ) ) ;
#26244 = ORIENTED_EDGE ( 'NONE', *, *, #15136, .F. ) ;
#26245 = CIRCLE ( 'NONE', #30529, 6.248999999999999666 ) ;
#26246 = VERTEX_POINT ( 'NONE', #13673 ) ;
#26247 = PERSON_AND_ORGANIZATION ( #6766, #25292 ) ;
#26248 = DIRECTION ( 'NONE',  ( 0.000000000000000000, 1.000000000000000000, 0.000000000000000000 ) ) ;
#26249 = CARTESIAN_POINT ( 'NONE',  ( 19.54632490742270434, -15.82374593131492801, -1.000000000000000000 ) ) ;
#26250 = ORIENTED_EDGE ( 'NONE', *, *, #13637, .F. ) ;
#26251 = DIRECTION ( 'NONE',  ( -6.062761635205578219E-17, -0.7071067811865465735, 0.7071067811865484609 ) ) ;
#26252 = ORIENTED_EDGE ( 'NONE', *, *, #28789, .T. ) ;
#26253 = AXIS2_PLACEMENT_3D ( 'NONE', #3916, #1059, #5755 ) ;
#26254 = VERTEX_POINT ( 'NONE', #4000 ) ;
#26255 = CARTESIAN_POINT ( 'NONE',  ( 9.331062908042635939, 15.00000000000000178, -4.612695725900422872 ) ) ;
#26256 = CARTESIAN_POINT ( 'NONE',  ( -5.562550801365593323, 2.752080473201636845, -2.228590825266444142 ) ) ;
#26257 = CIRCLE ( 'NONE', #11833, 4.000000000000001776 ) ;
#26258 = CARTESIAN_POINT ( 'NONE',  ( 2.037945749704312686E-16, 2.376879293651064540, 4.116875700062091248 ) ) ;
#26259 = VECTOR ( 'NONE', #18958, 1000.000000000000000 ) ;
#26260 = CARTESIAN_POINT ( 'NONE',  ( 1.750000000000000222, 7.003298780661427969, 4.817032923780590892 ) ) ;
#26262 = VERTEX_POINT ( 'NONE', #8976 ) ;
#26261 = CARTESIAN_POINT ( 'NONE',  ( 5.489343958331427409, 7.593062460271035263, -2.874233210898287538 ) ) ;
#26263 = CARTESIAN_POINT ( 'NONE',  ( -6.887550801365593500, -2.752080473201636845, 2.228590825266444586 ) ) ;
#26264 = AXIS2_PLACEMENT_3D ( 'NONE', #19758, #4719, #22615 ) ;
#26265 = CARTESIAN_POINT ( 'NONE',  ( 11.66870695089360588, 3.948484734291052067, 1.050000000000000044 ) ) ;
#26266 = DIRECTION ( 'NONE',  ( 0.000000000000000000, 0.000000000000000000, 1.000000000000000000 ) ) ;
#26267 = CARTESIAN_POINT ( 'NONE',  ( 20.92250000136559507, -1.913930629741527500, 2.363507492473149618 ) ) ;
#26268 = AXIS2_PLACEMENT_3D ( 'NONE', #28111, #2702, #2899 ) ;
#26269 = CARTESIAN_POINT ( 'NONE',  ( 12.44989959798868817, 0.5000000000000000000, 13.00000000000004441 ) ) ;
#26271 = ORIENTED_EDGE ( 'NONE', *, *, #32581, .F. ) ;
#26270 = DIRECTION ( 'NONE',  ( 1.000000000000000000, 0.000000000000000000, 0.000000000000000000 ) ) ;
#26272 = CIRCLE ( 'NONE', #11844, 6.000000000000001776 ) ;
#26273 = VECTOR ( 'NONE', #4823, 1000.000000000000000 ) ;
#26274 = EDGE_CURVE ( 'NONE', #31424, #20071, #26704, .T. ) ;
#26275 = CARTESIAN_POINT ( 'NONE',  ( 7.249760686538667009, 2.210816291636212405, 8.466096581343489191 ) ) ;
#26276 = CARTESIAN_POINT ( 'NONE',  ( 21.79750000273118715, -2.594547506269383685, -0.7685399846772043020 ) ) ;
#26277 = CARTESIAN_POINT ( 'NONE',  ( -17.76073374637450542, 7.575402792874719182, 2.048453119712636550 ) ) ;
#26278 = CARTESIAN_POINT ( 'NONE',  ( 107.3818320530746320, -16.38511360653449600, 0.000000000000000000 ) ) ;
#26279 = CARTESIAN_POINT ( 'NONE',  ( -2.655659815843975036, 0.1700350810728117334, -1.254089647469598612 ) ) ;
#26280 = CIRCLE ( 'NONE', #16113, 301.6269746700523342 ) ;
#26281 = CARTESIAN_POINT ( 'NONE',  ( 7.249760686538667009, 0.000000000000000000, 0.000000000000000000 ) ) ;
#26282 = B_SPLINE_SURFACE_WITH_KNOTS ( 'NONE', 1, 3, ( 
 ( #14599, #24804, #12094, #22292, #32503, #19780, #29988, #7080, #28477, #3078, #18263, #540, #2571, #7756, #55, #20466 ),
 ( #2418, #2929, #15259, #12588, #15765, #15090, #15408, #5398, #30837, #12737, #20629, #10729, #13091, #8249, #5234, #18442 ),
 ( #22943, #249, #30681, #25307, #10242, #17948, #28135, #13234, #25462, #23290, #15590, #7903, #393, #25619, #25805, #18093 ) ),
 .UNSPECIFIED., .F., .F., .F.,
 ( 2, 1, 2 ),
 ( 4, 2, 2, 2, 2, 2, 2, 4 ),
 ( -0.1724389077684020943, 0.000000000000000000, 1.000000000000000000 ),
 ( 0.000000000000000000, 0.5000000000000000000, 0.6250000000000000000, 0.7500000000000000000, 0.8125000000000000000, 0.8750000000000000000, 0.9375000000000000000, 1.000000000000000000 ),
 .UNSPECIFIED. ) ;
#26283 = CIRCLE ( 'NONE', #11855, 0.4499999999999999001 ) ;
#26284 = VECTOR ( 'NONE', #32420, 1000.000000000000000 ) ;
#26285 = DIRECTION ( 'NONE',  ( -0.9947025833170222153, -0.1027947991993880122, 0.000000000000000000 ) ) ;
#26286 = ORIENTED_EDGE ( 'NONE', *, *, #4184, .F. ) ;
#26287 = AXIS2_PLACEMENT_3D ( 'NONE', #11780, #21985, #32210 ) ;
#26288 =( BOUNDED_CURVE ( )  B_SPLINE_CURVE ( 2, ( #31469, #31323, #29130, #19091, #8548, #6216, #21606 ),
 .UNSPECIFIED., .F., .F. ) 
 B_SPLINE_CURVE_WITH_KNOTS ( ( 3, 2, 2, 3 ),
 ( 0.07856246879372839886, 0.09375000000000000000, 0.1093750000000000000, 0.1228822619934377414 ),
 .UNSPECIFIED. ) 
 CURVE ( )  GEOMETRIC_REPRESENTATION_ITEM ( )  RATIONAL_B_SPLINE_CURVE ( ( 0.9958568977429422819, 0.9260107535730678352, 1.000000000000000000, 0.9238795325112867385, 1.000000000000000000, 0.9341965377642873491, 0.9821626249036861100 ) ) 
 REPRESENTATION_ITEM ( '' )  );
#26289 = CIRCLE ( 'NONE', #16130, 6.250000000000000000 ) ;
#26290 = CARTESIAN_POINT ( 'NONE',  ( 17.37538333147191949, -21.16291065652713144, 1.499999999999996891 ) ) ;
#26291 = CARTESIAN_POINT ( 'NONE',  ( -2.988195613244121418, -0.2505024616802880577, -1.434921225358063879 ) ) ;
#26292 = CARTESIAN_POINT ( 'NONE',  ( 7.249760686538667009, -0.8180878109961253752, -8.711672189281435053 ) ) ;
#26295 = CARTESIAN_POINT ( 'NONE',  ( 107.9822664857447450, -17.81400392288609780, 4.398951253679784124 ) ) ;
#26294 = CARTESIAN_POINT ( 'NONE',  ( 108.0732140668137617, 18.58584473779162138, -4.631593095966008100 ) ) ;
#26293 = AXIS2_PLACEMENT_3D ( 'NONE', #8157, #18363, #15837 ) ;
#26296 = ORIENTED_EDGE ( 'NONE', *, *, #19625, .F. ) ;
#26297 = AXIS2_PLACEMENT_3D ( 'NONE', #11225, #8732, #16402 ) ;
#26298 = B_SPLINE_CURVE_WITH_KNOTS ( 'NONE', 3,
 ( #21049, #15990, #26056, #15845, #18032, #23528, #31254, #12824, #30594, #28071 ),
 .UNSPECIFIED., .F., .F.,
 ( 4, 2, 2, 2, 4 ),
 ( 1.968338519001761812E-07, 0.0005467927057105466870, 0.001093388577569193252, 0.001639984449427839925, 0.002186580321286487900 ),
 .UNSPECIFIED. ) ;
#26299 = DIRECTION ( 'NONE',  ( -0.9896144216807899463, 8.678901113238559347E-19, -0.1437473352845035635 ) ) ;
#26300 = ORIENTED_EDGE ( 'NONE', *, *, #23981, .T. ) ;
#26301 = CARTESIAN_POINT ( 'NONE',  ( 1.624999999999999778, 9.680994141368771011, 5.222868219166891812 ) ) ;
#26303 = ORIENTED_EDGE ( 'NONE', *, *, #14649, .T. ) ;
#26302 = DIRECTION ( 'NONE',  ( 7.770718973608941679E-17, 0.9063077870366467170, 0.4226182617407064912 ) ) ;
#26304 = ORIENTED_EDGE ( 'NONE', *, *, #11508, .F. ) ;
#26305 = CARTESIAN_POINT ( 'NONE',  ( 48.08400536259535585, -8.675012021204926427, -2.713652344655543391 ) ) ;
#26306 = CARTESIAN_POINT ( 'NONE',  ( 17.39502519979081185, -21.04076415203811479, -1.751145182513948573 ) ) ;
#26308 = EDGE_LOOP ( 'NONE', ( #7463, #30487, #8538, #26436 ) ) ;
#26307 = CARTESIAN_POINT ( 'NONE',  ( 5.377543748152549874, -4.007137495034861274, 6.940565734314584567 ) ) ;
#26309 = AXIS2_PLACEMENT_3D ( 'NONE', #23826, #11283, #26652 ) ;
#26310 = FACE_OUTER_BOUND ( 'NONE', #27210, .T. ) ;
#26311 = CARTESIAN_POINT ( 'NONE',  ( -4.155175026768859858, -6.548389795709734784, -1.745040213387592187 ) ) ;
#26312 = ADVANCED_FACE ( 'NONE', ( #22205 ), #14316, .F. ) ;
#26313 = CIRCLE ( 'NONE', #15069, 8.500000000000000000 ) ;
#26314 = CARTESIAN_POINT ( 'NONE',  ( 108.1166869805057900, -19.74962560783402310, -1.742921814161544569 ) ) ;
#26315 = AXIS2_PLACEMENT_3D ( 'NONE', #18250, #28465, #17934 ) ;
#26316 = CARTESIAN_POINT ( 'NONE',  ( 107.7918428252582714, -20.44935860102534519, -1.500028854543400181 ) ) ;
#26317 = CARTESIAN_POINT ( 'NONE',  ( 107.9477480374278571, -17.31694685422549540, -4.497032296529938300 ) ) ;
#26318 = CARTESIAN_POINT ( 'NONE',  ( 6.037141848526922594, 3.315649934461718740, 7.798898458906289299 ) ) ;
#26319 = CONICAL_SURFACE ( 'NONE', #2314, 10.00000000000000355, 0.03490658503988666728 ) ;
#26320 = AXIS2_PLACEMENT_3D ( 'NONE', #29692, #19655, #11621 ) ;
#26321 = VECTOR ( 'NONE', #23099, 1000.000000000000114 ) ;
#26322 = LINE ( 'NONE', #23796, #3288 ) ;
#26323 = CARTESIAN_POINT ( 'NONE',  ( 24.55656763645044904, -0.8852964313267484009, 2.499999999999997780 ) ) ;
#26324 = CARTESIAN_POINT ( 'NONE',  ( 85.08237158772919884, -5.954015309888582408, 2.787781826238851401 ) ) ;
#26325 = ADVANCED_FACE ( 'NONE', ( #31910 ), #29381, .F. ) ;
#26326 = AXIS2_PLACEMENT_3D ( 'NONE', #5121, #17138, #1960 ) ;
#26327 = DIRECTION ( 'NONE',  ( 1.000000000000000000, -0.000000000000000000, -0.000000000000000000 ) ) ;
#26328 = CARTESIAN_POINT ( 'NONE',  ( 5.489344087273876127, 5.138668362895363551, -6.285690376021046077 ) ) ;
#26329 = EDGE_LOOP ( 'NONE', ( #31838, #11801, #32633, #18553 ) ) ;
#26330 = CARTESIAN_POINT ( 'NONE',  ( 5.612718622971681448, -2.996580135471476503, -7.650113768151205029 ) ) ;
#26331 = PERSON ( 'NAUO-PER6', 'UNSPECIFIED', 'UNSPECIFIED', ('UNSPECIFIED'), ('UNSPECIFIED'), ('UNSPECIFIED') ) ;
#26332 = LINE ( 'NONE', #32346, #654 ) ;
#26333 = ADVANCED_FACE ( 'NONE', ( #9475 ), #24210, .T. ) ;
#26334 = CARTESIAN_POINT ( 'NONE',  ( 17.75999999999999801, -2.208672634433321348E-15, 0.000000000000000000 ) ) ;
#26335 = ORIENTED_EDGE ( 'NONE', *, *, #10979, .T. ) ;
#26336 = CARTESIAN_POINT ( 'NONE',  ( 22.36000000136559152, -1.570731468192933633, -2.892927487894330074 ) ) ;
#26337 = VECTOR ( 'NONE', #7810, 1000.000000000000000 ) ;
#26338 = AXIS2_PLACEMENT_3D ( 'NONE', #24525, #14324, #32078 ) ;
#26339 = CARTESIAN_POINT ( 'NONE',  ( -15.26206363037222857, -25.49623161314220710, 1.500000000000013989 ) ) ;
#26340 = DIRECTION ( 'NONE',  ( 0.000000000000000000, 1.000000000000000000, 3.469446951953612611E-15 ) ) ;
#26341 = ORIENTED_EDGE ( 'NONE', *, *, #17343, .T. ) ;
#26342 = CARTESIAN_POINT ( 'NONE',  ( 0.5492144360001000036, -7.007719521915549699, -1.500000000000000666 ) ) ;
#26343 = ORIENTED_EDGE ( 'NONE', *, *, #1570, .F. ) ;
#26344 = CIRCLE ( 'NONE', #26874, 3.024999999999999911 ) ;
#26346 = ADVANCED_FACE ( 'NONE', ( #29573 ), #27045, .T. ) ;
#26345 = AXIS2_PLACEMENT_3D ( 'NONE', #14049, #13560, #26756 ) ;
#26347 = ORIENTED_EDGE ( 'NONE', *, *, #6078, .F. ) ;
#26348 = CARTESIAN_POINT ( 'NONE',  ( 6.530491627857222703, 3.540416224243776888, -7.903708701126651803 ) ) ;
#26349 = APPROVAL_DATE_TIME ( #28528, #32320 ) ;
#26350 = ORIENTED_EDGE ( 'NONE', *, *, #8107, .F. ) ;
#26351 = VERTEX_POINT ( 'NONE', #3818 ) ;
#26352 = CYLINDRICAL_SURFACE ( 'NONE', #32648, 8.500000000000000000 ) ;
#26353 = SECURITY_CLASSIFICATION ( '', '', #22218 ) ;
#26354 = ORIENTED_EDGE ( 'NONE', *, *, #20308, .T. ) ;
#26355 = CARTESIAN_POINT ( 'NONE',  ( 21.25111450864416085, -3.256483526998273983E-15, 2.499999999999998668 ) ) ;
#26357 = ORIENTED_EDGE ( 'NONE', *, *, #9454, .T. ) ;
#26356 = DIRECTION ( 'NONE',  ( 1.000000000000000000, -0.000000000000000000, -0.000000000000000000 ) ) ;
#26358 = CARTESIAN_POINT ( 'NONE',  ( 2.274274201621893976, 1.464956435144894931, 10.90201369671109610 ) ) ;
#26359 = CARTESIAN_POINT ( 'NONE',  ( 0.7632845268398871230, 8.461683424509313767, 2.223716399045601921 ) ) ;
#26360 = CARTESIAN_POINT ( 'NONE',  ( 19.10390797508231131, -2.015740111943978619, -0.07017451552781628354 ) ) ;
#26361 = CARTESIAN_POINT ( 'NONE',  ( 5.887530252753763627, 5.105578361685915390, 6.663910820542600533 ) ) ;
#26362 = CARTESIAN_POINT ( 'NONE',  ( 107.5579690617258848, -18.92842216329967542, 4.649137216790264482 ) ) ;
#26363 = CIRCLE ( 'NONE', #30123, 8.500000000000000000 ) ;
#26364 = AXIS2_PLACEMENT_3D ( 'NONE', #16467, #27790, #29699 ) ;
#26365 = CARTESIAN_POINT ( 'NONE',  ( -3.950050800000000528, -3.113457007523259268, 0.9222479816126455399 ) ) ;
#26366 = DIRECTION ( 'NONE',  ( 0.000000000000000000, 1.000000000000000000, 0.000000000000000000 ) ) ;
#26367 = CARTESIAN_POINT ( 'NONE',  ( 35.27971914370662887, -7.797547734959323407, -2.184956776477516183 ) ) ;
#26368 = CARTESIAN_POINT ( 'NONE',  ( 12.44989959798878587, 20.00000000000000000, 1.818740222761551451 ) ) ;
#26370 = ADVANCED_FACE ( 'NONE', ( #1827 ), #6969, .F. ) ;
#26369 =( REPRESENTATION_RELATIONSHIP ('NONE','NONE', #1085, #30799 ) REPRESENTATION_RELATIONSHIP_WITH_TRANSFORMATION ( #15456 )SHAPE_REPRESENTATION_RELATIONSHIP( ) );
#26371 = AXIS2_PLACEMENT_3D ( 'NONE', #29304, #26802, #1412 ) ;
#26372 = EDGE_CURVE ( 'NONE', #24462, #9763, #11827, .T. ) ;
#26373 = AXIS2_PLACEMENT_3D ( 'NONE', #21785, #31993, #16785 ) ;
#26374 = AXIS2_PLACEMENT_3D ( 'NONE', #26229, #31268, #18690 ) ;
#26375 = DIRECTION ( 'NONE',  ( -1.000000000000000000, 1.387778780781444256E-14, 0.000000000000000000 ) ) ;
#26376 = DIRECTION ( 'NONE',  ( 0.000000000000000000, 0.9659258262890679791, 0.2588190451025216277 ) ) ;
#26377 = CARTESIAN_POINT ( 'NONE',  ( 22.79750000273118715, -2.594547506269383685, -0.7685399846772043020 ) ) ;
#26378 = CARTESIAN_POINT ( 'NONE',  ( 21.99035326629933706, -21.86692099231501984, 1.263015267642078054 ) ) ;
#26379 = SECURITY_CLASSIFICATION ( '', '', #8953 ) ;
#26380 = CARTESIAN_POINT ( 'NONE',  ( 108.1104766427000925, 18.79333746343691658, 4.476124295753212579 ) ) ;
#26381 = EDGE_CURVE ( 'NONE', #26504, #572, #3827, .T. ) ;
#26382 = CARTESIAN_POINT ( 'NONE',  ( -3.012550801365593500, 3.368539882008727115, 1.828967928396026954 ) ) ;
#26383 = VERTEX_POINT ( 'NONE', #11658 ) ;
#26384 = CARTESIAN_POINT ( 'NONE',  ( -4.850050800000001772, -1.549418761218565477, 2.853674364686380471 ) ) ;
#26385 = CYLINDRICAL_SURFACE ( 'NONE', #32769, 0.5000000000000004441 ) ;
#26386 = CARTESIAN_POINT ( 'NONE',  ( -23.35000000000000142, -10.96966150227469505, 4.000000000000000000 ) ) ;
#26387 = CARTESIAN_POINT ( 'NONE',  ( 8.845957756764844859, -0.9823800963980794387, 1.500000000000000000 ) ) ;
#26388 = VERTEX_POINT ( 'NONE', #14486 ) ;
#26389 = CARTESIAN_POINT ( 'NONE',  ( 4.749760686538667009, -2.741043480754977946, 7.530955069117504230 ) ) ;
#26390 = EDGE_CURVE ( 'NONE', #29074, #9056, #13470, .T. ) ;
#26391 = CC_DESIGN_PERSON_AND_ORGANIZATION_ASSIGNMENT ( #20021, #32720, ( #26402 ) ) ;
#26392 = CIRCLE ( 'NONE', #14622, 8.999999999999998224 ) ;
#26393 = CIRCLE ( 'NONE', #9807, 11.00000000000000000 ) ;
#26394 = ORIENTED_EDGE ( 'NONE', *, *, #15714, .T. ) ;
#26395 = CARTESIAN_POINT ( 'NONE',  ( 1.306406124627619736, -9.317880825549442747, 1.499999999999999556 ) ) ;
#26396 = PERSON_AND_ORGANIZATION ( #6766, #25292 ) ;
#26397 = CARTESIAN_POINT ( 'NONE',  ( 102.3749895180304605, -3.302517831815073190, 4.312042181588143563 ) ) ;
#26398 = DIRECTION ( 'NONE',  ( -1.000000000000000000, 0.000000000000000000, -0.000000000000000000 ) ) ;
#26399 = CARTESIAN_POINT ( 'NONE',  ( 10.56870887191539587, -4.616489984850547401, 1.946309384392575392 ) ) ;
#26400 = DIRECTION ( 'NONE',  ( 0.000000000000000000, 0.000000000000000000, -1.000000000000000000 ) ) ;
#26401 = ORIENTED_EDGE ( 'NONE', *, *, #2603, .T. ) ;
#26402 = SECURITY_CLASSIFICATION ( '', '', #17827 ) ;
#26403 = CARTESIAN_POINT ( 'NONE',  ( 7.249760686538667009, -8.466096581343496297, 2.210816291636187536 ) ) ;
#26404 = CARTESIAN_POINT ( 'NONE',  ( 25.93644697397389720, 19.04148194274331729, -1.255264836812425067 ) ) ;
#26405 = CARTESIAN_POINT ( 'NONE',  ( 21.79750000136559507, 2.363507492473148286, 1.913930629741525058 ) ) ;
#26407 = EDGE_LOOP ( 'NONE', ( #15375, #5739, #21633 ) ) ;
#26406 = CARTESIAN_POINT ( 'NONE',  ( -7.000050800000000351, 7.347880794884120722E-16, 6.000000000000000888 ) ) ;
#26408 = CARTESIAN_POINT ( 'NONE',  ( -2.412550801365592967, 1.828967928396027176, -3.368539882008727115 ) ) ;
#26409 = CARTESIAN_POINT ( 'NONE',  ( 108.2737963169669655, 19.70276585262076452, 2.534196689747376663 ) ) ;
#26410 = DIRECTION ( 'NONE',  ( -0.000000000000000000, -1.000000000000000000, 0.000000000000000000 ) ) ;
#26411 = ADVANCED_FACE ( 'NONE', ( #6659 ), #16848, .T. ) ;
#26412 = EDGE_LOOP ( 'NONE', ( #1162, #29833, #11841, #18142 ) ) ;
#26413 = ORIENTED_EDGE ( 'NONE', *, *, #4463, .F. ) ;
#26414 = CARTESIAN_POINT ( 'NONE',  ( 0.000000000000000000, 2.429606751577119805, -5.757344182232886354 ) ) ;
#26415 = VECTOR ( 'NONE', #417, 1000.000000000000000 ) ;
#26416 = DIRECTION ( 'NONE',  ( -1.000000000000000000, 0.000000000000000000, 0.000000000000000000 ) ) ;
#26417 = CARTESIAN_POINT ( 'NONE',  ( 1.750000000000000222, -7.673322273190749776, 3.656518192455051608 ) ) ;
#26418 = CARTESIAN_POINT ( 'NONE',  ( -0.4046470899336805926, -12.07320251013792323, 5.485967528433935314 ) ) ;
#26419 = DIRECTION ( 'NONE',  ( 0.000000000000000000, 0.8660254037844362651, 0.5000000000000039968 ) ) ;
#26420 = CARTESIAN_POINT ( 'NONE',  ( -58.12302020695992866, -3.824990096116924310, 5.760101628985031752 ) ) ;
#26421 = CARTESIAN_POINT ( 'NONE',  ( -3.337550801365593678, 1.828967928396027398, -3.368539882008727115 ) ) ;
#26422 = ORGANIZATION ( 'NAUO-ORG5', 'UNSPECIFIED', 'UNSPECIFIED' ) ;
#26423 = CARTESIAN_POINT ( 'NONE',  ( 10.00000000000000000, 4.893557421779793832E-14, -4.753758587302147731 ) ) ;
#26424 = FACE_OUTER_BOUND ( 'NONE', #1572, .T. ) ;
#26425 = ORIENTED_EDGE ( 'NONE', *, *, #17739, .F. ) ;
#26426 = CARTESIAN_POINT ( 'NONE',  ( 2.795120501772739630, -8.308193303464506130, -5.116149273377909701 ) ) ;
#26427 = EDGE_CURVE ( 'NONE', #12534, #32817, #8143, .T. ) ;
#26428 = ORIENTED_EDGE ( 'NONE', *, *, #20793, .F. ) ;
#26429 = CALENDAR_DATE ( 2026, 6, 10 ) ;
#26430 = DIRECTION ( 'NONE',  ( 0.000000000000000000, 1.000000000000000000, 0.000000000000000000 ) ) ;
#26431 = CIRCLE ( 'NONE', #7212, 8.500000000000000000 ) ;
#26432 = CARTESIAN_POINT ( 'NONE',  ( 0.000000000000000000, 4.762163868918412923, -9.915734732513168836 ) ) ;
#26433 = VERTEX_POINT ( 'NONE', #32260 ) ;
#26434 = CYLINDRICAL_SURFACE ( 'NONE', #5498, 2.499999999999997780 ) ;
#26435 = ORIENTED_EDGE ( 'NONE', *, *, #8507, .F. ) ;
#26436 = ORIENTED_EDGE ( 'NONE', *, *, #21878, .F. ) ;
#26437 = DIRECTION ( 'NONE',  ( -8.326672684688674053E-17, -0.3746065934159164001, 0.9271838545667857590 ) ) ;
#26438 = CARTESIAN_POINT ( 'NONE',  ( -3.312550801365593767, -1.088641768524163611, -3.675193018007245627 ) ) ;
#26439 = ADVANCED_FACE ( 'NONE', ( #21702 ), #1332, .F. ) ;
#26440 = CARTESIAN_POINT ( 'NONE',  ( 6.682200477904377323, -7.715721153621220019, 1.500000000000000000 ) ) ;
#26441 = CARTESIAN_POINT ( 'NONE',  ( 0.6153366188829528793, -5.549022540254107128, -1.499999999999999556 ) ) ;
#26443 = EDGE_LOOP ( 'NONE', ( #17011, #15687, #12805, #31136 ) ) ;
#26442 = CARTESIAN_POINT ( 'NONE',  ( 12.71851269413118857, 6.640480776649662076, -1.500000000000000222 ) ) ;
#26444 = CARTESIAN_POINT ( 'NONE',  ( -6.687550801365594211, -2.228590825266444586, -2.752080473201636401 ) ) ;
#26445 = CARTESIAN_POINT ( 'NONE',  ( 15.58693300141982441, 10.49296960241998100, 1.050000000000000044 ) ) ;
#26446 = EDGE_CURVE ( 'NONE', #25541, #7070, #30977, .T. ) ;
#26447 = CARTESIAN_POINT ( 'NONE',  ( 8.235945875020298956, -19.08855532455987358, 1.500000000000315525 ) ) ;
#26448 = CARTESIAN_POINT ( 'NONE',  ( 20.79750000136559507, 0.3178988483021036315, 3.024605502323848949 ) ) ;
#26450 = ORIENTED_EDGE ( 'NONE', *, *, #6346, .T. ) ;
#26449 = DIRECTION ( 'NONE',  ( 0.000000000000000000, 0.000000000000000000, 1.000000000000000000 ) ) ;
#26451 = CARTESIAN_POINT ( 'NONE',  ( 0.000000000000000000, 0.000000000000000000, 0.000000000000000000 ) ) ;
#26452 = DIRECTION ( 'NONE',  ( 0.2951703194034056010, -0.3797261271633441404, 0.8767454310646958238 ) ) ;
#26453 = CARTESIAN_POINT ( 'NONE',  ( -21.68109753780424143, 3.720325412122139408, 1.500000000000000000 ) ) ;
#26454 = CARTESIAN_POINT ( 'NONE',  ( 110.0816933595962439, 17.77332459904788209, 5.412820279296879811 ) ) ;
#26455 = LINE ( 'NONE', #13376, #6572 ) ;
#26456 = DIRECTION ( 'NONE',  ( 0.000000000000000000, 0.4067366430758009299, -0.9135454576426005335 ) ) ;
#26457 = CARTESIAN_POINT ( 'NONE',  ( 9.302055952193859056, 0.2457637073201327793, 1.049999999999999822 ) ) ;
#26458 = CARTESIAN_POINT ( 'NONE',  ( -6.837550801365593678, -3.675193018007246071, 1.088641768524163167 ) ) ;
#26459 = ORIENTED_EDGE ( 'NONE', *, *, #24064, .T. ) ;
#26460 = CARTESIAN_POINT ( 'NONE',  ( 108.3696618535068126, 20.23658298680886958, 1.395260099363828665 ) ) ;
#26461 = LINE ( 'NONE', #23922, #18659 ) ;
#26463 = CARTESIAN_POINT ( 'NONE',  ( 24.08745121461140570, -17.31475877198404589, 1.374955925956904412 ) ) ;
#26462 = DIRECTION ( 'NONE',  ( -0.000000000000000000, -1.000000000000000000, -0.000000000000000000 ) ) ;
#26464 = ORIENTED_EDGE ( 'NONE', *, *, #13332, .F. ) ;
#26465 = DIRECTION ( 'NONE',  ( -0.000000000000000000, 0.000000000000000000, 1.000000000000000000 ) ) ;
#26466 = ORIENTED_EDGE ( 'NONE', *, *, #12571, .T. ) ;
#26467 = FACE_OUTER_BOUND ( 'NONE', #4116, .T. ) ;
#26469 = ORIENTED_EDGE ( 'NONE', *, *, #1821, .T. ) ;
#26468 = CARTESIAN_POINT ( 'NONE',  ( 0.7632845268398871230, 8.461683424509313767, 2.223716399045601921 ) ) ;
#26470 = ORIENTED_EDGE ( 'NONE', *, *, #20856, .T. ) ;
#26471 = FACE_OUTER_BOUND ( 'NONE', #19093, .T. ) ;
#26472 = ADVANCED_FACE ( 'NONE', ( #15324 ), #15151, .T. ) ;
#26473 = ADVANCED_FACE ( 'NONE', ( #12652 ), #5147, .T. ) ;
#26474 = CARTESIAN_POINT ( 'NONE',  ( 0.7632845268398871230, 0.000000000000000000, 0.000000000000000000 ) ) ;
#26476 = ORIENTED_EDGE ( 'NONE', *, *, #23865, .F. ) ;
#26475 = LINE ( 'NONE', #31655, #21902 ) ;
#26477 = CARTESIAN_POINT ( 'NONE',  ( 19.01933586186248348, 14.56926017555086972, -1.500000000000000000 ) ) ;
#26478 = CARTESIAN_POINT ( 'NONE',  ( -2.160443185886078865, -12.59954908393165240, -1.743857611967832622 ) ) ;
#26479 = CARTESIAN_POINT ( 'NONE',  ( 34.98193025661424826, 0.5174497483512506824, 2.482234843104951239 ) ) ;
#26480 = CARTESIAN_POINT ( 'NONE',  ( 7.154313483739800361, -6.723190066291400591, -1.000000000000000000 ) ) ;
#26481 = CARTESIAN_POINT ( 'NONE',  ( 107.4501371742636735, -17.36131785966625785, -4.525205764350905824 ) ) ;
#26482 = CARTESIAN_POINT ( 'NONE',  ( 25.75999999999999801, -2.208672634433321348E-15, 0.000000000000000000 ) ) ;
#26483 = CARTESIAN_POINT ( 'NONE',  ( 24.61000000273118715, -1.573300977624594976, 1.942864903642425700 ) ) ;
#26484 = CARTESIAN_POINT ( 'NONE',  ( -2.223027892448374399, -2.927336879245633572, 4.522129901861158707 ) ) ;
#26485 = CARTESIAN_POINT ( 'NONE',  ( 2.995361005316234060, -0.2432974174152501834, 1.434016190628301546 ) ) ;
#26486 =( BOUNDED_SURFACE ( )  B_SPLINE_SURFACE ( 3, 2, ( 
 ( #32752, #4989, #25376 ),
 ( #15481, #14979, #22356 ),
 ( #32569, #12503, #9829 ),
 ( #12314, #20045, #20355 ),
 ( #30240, #20192, #30389 ),
 ( #7310, #27697, #4802 ),
 ( #7655, #17854, #25194 ),
 ( #2319, #7462, #17662 ),
 ( #2485, #28052, #25883 ),
 ( #26378, #31383, #31534 ),
 ( #13298, #13468, #23505 ),
 ( #15829, #21329, #10809 ) ),
 .UNSPECIFIED., .F., .F., .F. ) 
 B_SPLINE_SURFACE_WITH_KNOTS ( ( 4, 2, 2, 2, 2, 4 ),
 ( 3, 3 ),
 ( 0.01237460209466365035, 0.01250742172631305257, 0.01264024135796245653, 0.01290588062126126270, 0.01343715914785887505, 0.01449971620105409802 ),
 ( 0.000000000000000000, 1.000000000000000000 ),
 .UNSPECIFIED. ) 
 GEOMETRIC_REPRESENTATION_ITEM ( )  RATIONAL_B_SPLINE_SURFACE ( (
 ( 1.000000000000000000, 0.9985794324048127280, 1.000000000000000000),
 ( 1.000000000000000000, 0.9985649967291867490, 1.000000000000000000),
 ( 1.000000000000000000, 0.9977546568863879806, 1.000000000000000000),
 ( 1.000000000000000000, 0.9959318651690971524, 1.000000000000000000),
 ( 1.000000000000000000, 0.9948682866524912738, 1.000000000000000000),
 ( 1.000000000000000000, 0.9916149370760292125, 1.000000000000000000),
 ( 1.000000000000000000, 0.9892930324833523192, 1.000000000000000000),
 ( 1.000000000000000000, 0.9821212088646815719, 1.000000000000000000),
 ( 1.000000000000000000, 0.9771237707447232301, 1.000000000000000000),
 ( 1.000000000000000000, 0.9616790524998285461, 1.000000000000000000),
 ( 1.000000000000000000, 0.9507373671939208792, 1.000000000000000000),
 ( 1.000000000000000000, 0.9391581256476260187, 1.000000000000000000) ) ) 
 REPRESENTATION_ITEM ( '' )  SURFACE ( )  );
#26487 = ORIENTED_EDGE ( 'NONE', *, *, #15212, .T. ) ;
#26488 = CARTESIAN_POINT ( 'NONE',  ( 7.249760686538667009, 0.000000000000000000, 0.000000000000000000 ) ) ;
#26489 = CARTESIAN_POINT ( 'NONE',  ( -55.91000000000000369, -10.96999999999998643, 1.499999999999999556 ) ) ;
#26490 = EDGE_CURVE ( 'NONE', #4375, #28862, #18287, .T. ) ;
#26491 = CARTESIAN_POINT ( 'NONE',  ( 2.274274201625327230, 10.90201369670498543, 1.464956435139579183 ) ) ;
#26492 = ORIENTED_EDGE ( 'NONE', *, *, #9549, .F. ) ;
#26493 = CARTESIAN_POINT ( 'NONE',  ( 25.30158241411874798, -1.345927778950697595, 2.192379955416479120 ) ) ;
#26494 = CARTESIAN_POINT ( 'NONE',  ( 15.55254023221931448, 20.42149909151575926, -5.396302277755718357 ) ) ;
#26495 = ORIENTED_EDGE ( 'NONE', *, *, #25876, .T. ) ;
#26496 = PLANE ( 'NONE',  #20375 ) ;
#26497 = VERTEX_POINT ( 'NONE', #26523 ) ;
#26498 = EDGE_CURVE ( 'NONE', #5204, #21729, #22185, .T. ) ;
#26499 = ORIENTED_EDGE ( 'NONE', *, *, #19243, .T. ) ;
#26500 = CARTESIAN_POINT ( 'NONE',  ( 25.14437127914504444, -17.52581659214493115, -1.374992938514766116 ) ) ;
#26501 = DATE_AND_TIME ( #3454, #25338 ) ;
#26503 = ORIENTED_EDGE ( 'NONE', *, *, #26835, .T. ) ;
#26502 = CARTESIAN_POINT ( 'NONE',  ( 8.901201215455881055, 15.00000000000000000, 5.412820279296879811 ) ) ;
#26504 = VERTEX_POINT ( 'NONE', #3300 ) ;
#26505 = FACE_OUTER_BOUND ( 'NONE', #11367, .T. ) ;
#26506 = EDGE_CURVE ( 'NONE', #2670, #7224, #31069, .T. ) ;
#26507 = ORIENTED_EDGE ( 'NONE', *, *, #27217, .T. ) ;
#26508 = CARTESIAN_POINT ( 'NONE',  ( 0.7632845268398871230, 2.223716399045691183, -8.461683424509292450 ) ) ;
#26510 = VERTEX_POINT ( 'NONE', #21184 ) ;
#26509 = CARTESIAN_POINT ( 'NONE',  ( 19.01022352368569557, -3.062944256724156489, -0.8105616806061153312 ) ) ;
#26511 = CARTESIAN_POINT ( 'NONE',  ( 22.00111451137534502, -1.241879311143409511E-16, -2.499999999999998668 ) ) ;
#26512 = CARTESIAN_POINT ( 'NONE',  ( 0.7632845268398871230, -8.461683424509331530, 2.223716399045538861 ) ) ;
#26513 = EDGE_CURVE ( 'NONE', #11008, #13391, #13150, .T. ) ;
#26514 = CARTESIAN_POINT ( 'NONE',  ( 3.249999999999999556, 0.000000000000000000, 0.000000000000000000 ) ) ;
#26515 = LINE ( 'NONE', #1586, #27428 ) ;
#26516 = CARTESIAN_POINT ( 'NONE',  ( -50.81000000000000227, -10.96999999999998643, 5.949999999999999289 ) ) ;
#26517 = FACE_OUTER_BOUND ( 'NONE', #24842, .T. ) ;
#26518 = EDGE_CURVE ( 'NONE', #533, #33011, #3874, .T. ) ;
#26519 = CARTESIAN_POINT ( 'NONE',  ( 29.18336473368350070, -8.306880066003914820, -0.07017451552783354751 ) ) ;
#26520 = DIRECTION ( 'NONE',  ( 0.000000000000000000, 0.9659258262890698665, -0.2588190451025149663 ) ) ;
#26521 = DIRECTION ( 'NONE',  ( 1.000000000000000000, -0.000000000000000000, -0.000000000000000000 ) ) ;
#26522 = LINE ( 'NONE', #803, #8632 ) ;
#26523 = CARTESIAN_POINT ( 'NONE',  ( 0.7632845268398871230, 4.729683950898978750, -7.360373001730866171 ) ) ;
#26524 = CARTESIAN_POINT ( 'NONE',  ( 5.489344087273876127, -6.285690376021061176, -5.138668362895343122 ) ) ;
#26525 = EDGE_CURVE ( 'NONE', #28440, #2672, #5648, .T. ) ;
#26526 = CARTESIAN_POINT ( 'NONE',  ( -50.81000000000000227, -10.96999999999998643, 2.028141679950118625 ) ) ;
#26527 = CARTESIAN_POINT ( 'NONE',  ( -3.312550801365593767, -1.088641768524163389, -3.675193018007246071 ) ) ;
#26528 = VERTEX_POINT ( 'NONE', #8311 ) ;
#26529 = CARTESIAN_POINT ( 'NONE',  ( -7.550050800000000173, 3.113457007523260156, -0.9222479816126439855 ) ) ;
#26530 = EDGE_CURVE ( 'NONE', #20748, #26134, #456, .T. ) ;
#26531 = CARTESIAN_POINT ( 'NONE',  ( 108.1960732670209211, 19.26997324246898557, 4.630839363390588659 ) ) ;
#26532 = CARTESIAN_POINT ( 'NONE',  ( 6.784984840995086586, -5.399320162307873261, 1.500000000000000000 ) ) ;
#26533 = ORIENTED_EDGE ( 'NONE', *, *, #774, .T. ) ;
#26534 = DIRECTION ( 'NONE',  ( -1.000000000000000000, -0.000000000000000000, -0.000000000000000000 ) ) ;
#26535 = EDGE_LOOP ( 'NONE', ( #29924, #2694, #18987, #21144, #32882 ) ) ;
#26536 = CARTESIAN_POINT ( 'NONE',  ( 0.5636301045504281682, -7.175383382611437710, 1.500000000000000444 ) ) ;
#26537 = COORDINATED_UNIVERSAL_TIME_OFFSET ( 0, 0, .AHEAD. ) ;
#26538 = EDGE_CURVE ( 'NONE', #3978, #8056, #17053, .T. ) ;
#26539 = CARTESIAN_POINT ( 'NONE',  ( 54.96134875812031595, -5.932951279990229310, 4.312042181584448741 ) ) ;
#26540 = EDGE_CURVE ( 'NONE', #25174, #32970, #31117, .T. ) ;
#26541 = DIRECTION ( 'NONE',  ( 1.000000000000000000, 0.000000000000000000, 0.000000000000000000 ) ) ;
#26542 = CARTESIAN_POINT ( 'NONE',  ( 2.437082316315975383, -1.217322776604802037, 10.59788678609686308 ) ) ;
#26543 = CARTESIAN_POINT ( 'NONE',  ( 2.274274201625327230, -4.762163868918204201, -9.915734732513268312 ) ) ;
#26544 = ORIENTED_EDGE ( 'NONE', *, *, #12013, .T. ) ;
#26545 = EDGE_CURVE ( 'NONE', #15334, #21706, #23266, .T. ) ;
#26546 = CARTESIAN_POINT ( 'NONE',  ( 0.3045633657612867307, 6.808202580038980045, 7.698316278340386454 ) ) ;
#26547 = CARTESIAN_POINT ( 'NONE',  ( -3.691385125341854500E-13, 10.85582367538961179, -1.425064293572943619 ) ) ;
#26548 = CARTESIAN_POINT ( 'NONE',  ( 18.95251007638874441, -3.708064768245253884, -2.336400966235247623 ) ) ;
#26550 = ORIENTED_EDGE ( 'NONE', *, *, #23429, .T. ) ;
#26549 = PLANE ( 'NONE',  #11752 ) ;
#26551 = CARTESIAN_POINT ( 'NONE',  ( -3.512550801365593944, -3.675193018007246071, 1.088641768524163167 ) ) ;
#26552 = CARTESIAN_POINT ( 'NONE',  ( 25.75999999999999801, 5.000000000000000000, 0.000000000000000000 ) ) ;
#26553 = CARTESIAN_POINT ( 'NONE',  ( 0.7632845268398888994, -6.772677083992417302, 5.538577986808867593 ) ) ;
#26554 = ORIENTED_EDGE ( 'NONE', *, *, #29176, .F. ) ;
#26555 = EDGE_CURVE ( 'NONE', #17821, #13648, #16150, .T. ) ;
#26556 = DIRECTION ( 'NONE',  ( -1.000000000000000000, -0.000000000000000000, 0.000000000000000000 ) ) ;
#26557 = LINE ( 'NONE', #8661, #25144 ) ;
#26558 = DIRECTION ( 'NONE',  ( -0.000000000000000000, -1.000000000000000000, 0.000000000000000000 ) ) ;
#26559 = CARTESIAN_POINT ( 'NONE',  ( 3.554613218822865850, -15.76807188677689986, 4.522129901861159595 ) ) ;
#26560 = ORIENTED_EDGE ( 'NONE', *, *, #22094, .T. ) ;
#26561 = LINE ( 'NONE', #16500, #28981 ) ;
#26562 = ORIENTED_EDGE ( 'NONE', *, *, #32087, .F. ) ;
#26563 = CARTESIAN_POINT ( 'NONE',  ( 5.885541736258997680, 2.519172009312041105, -8.006759975090627535 ) ) ;
#26564 = CARTESIAN_POINT ( 'NONE',  ( -2.124956573341760357, 1.323625320507108460, 3.284597389080124774 ) ) ;
#26565 = CARTESIAN_POINT ( 'NONE',  ( -2.837550801365593678, -3.675193018007245627, 1.088641768524163389 ) ) ;
#26566 = CARTESIAN_POINT ( 'NONE',  ( 0.1606232843927789256, -10.56438947505147929, -1.177222770084765502 ) ) ;
#26567 = DIRECTION ( 'NONE',  ( 0.03487826274237457863, -0.9987827659587181772, 0.03487826274237498803 ) ) ;
#26568 = ORIENTED_EDGE ( 'NONE', *, *, #17352, .T. ) ;
#26569 = DIRECTION ( 'NONE',  ( -3.469446951953614189E-15, 0.000000000000000000, -1.000000000000000000 ) ) ;
#26570 = ORIENTED_EDGE ( 'NONE', *, *, #26966, .F. ) ;
#26571 = PERSON_AND_ORGANIZATION_ROLE ( 'classification_officer' ) ;
#26572 = ADVANCED_FACE ( 'NONE', ( #28551, #13467 ), #23686, .F. ) ;
#26573 = CARTESIAN_POINT ( 'NONE',  ( 54.97722363747754315, -6.506539134378061640, 3.993434333287562144 ) ) ;
#26574 = EDGE_CURVE ( 'NONE', #32326, #20387, #7387, .T. ) ;
#26575 = DIRECTION ( 'NONE',  ( 0.07581065956227768521, 0.4221436659004723091, -0.9033534575330096628 ) ) ;
#26576 = VERTEX_POINT ( 'NONE', #6884 ) ;
#26577 = CARTESIAN_POINT ( 'NONE',  ( -8.000050800000000351, 0.000000000000000000, 0.000000000000000000 ) ) ;
#26578 = ORIENTED_EDGE ( 'NONE', *, *, #3720, .F. ) ;
#26579 = EDGE_LOOP ( 'NONE', ( #9067, #15155, #29505, #11901 ) ) ;
#26580 = CARTESIAN_POINT ( 'NONE',  ( 3.249999999999999556, 8.461683424509345741, -2.223716399045483350 ) ) ;
#26581 = CARTESIAN_POINT ( 'NONE',  ( -5.912550801365594744, -3.675193018007245627, 1.088641768524163389 ) ) ;
#26582 = CARTESIAN_POINT ( 'NONE',  ( 22.67249999999999943, -1.291182301015472378, -2.378061970571982098 ) ) ;
#26583 = CARTESIAN_POINT ( 'NONE',  ( -3.712942406915326288, 4.884725290497410777E-15, -2.999999999999999556 ) ) ;
#26585 = ORIENTED_EDGE ( 'NONE', *, *, #4036, .F. ) ;
#26584 = CARTESIAN_POINT ( 'NONE',  ( 32.37020706055090358, 18.00000000000000355, -3.000000000000004885 ) ) ;
#26586 = CARTESIAN_POINT ( 'NONE',  ( -6.587550801365593678, 0.3701630799359330593, -3.521866450007987037 ) ) ;
#26587 = CARTESIAN_POINT ( 'NONE',  ( 84.62099044691464655, -6.357652361207289715, 2.184954680079133293 ) ) ;
#26588 = CARTESIAN_POINT ( 'NONE',  ( 14.48597245533614064, -20.94846345271118437, 1.500000000000000444 ) ) ;
#26589 = DIRECTION ( 'NONE',  ( 0.000000000000000000, 0.7431448254773954654, -0.6691306063588569053 ) ) ;
#26591 = ORIENTED_EDGE ( 'NONE', *, *, #1172, .T. ) ;
#26590 = DIRECTION ( 'NONE',  ( 0.000000000000000000, -0.8191520442889869136, -0.5735764363510531538 ) ) ;
#26592 = EDGE_CURVE ( 'NONE', #32541, #5615, #1291, .T. ) ;
#26593 = CC_DESIGN_DATE_AND_TIME_ASSIGNMENT ( #3976, #16976, ( #2068 ) ) ;
#26594 = LINE ( 'NONE', #3696, #11477 ) ;
#26595 = DIRECTION ( 'NONE',  ( -1.000000000000000000, 8.574039729943022041E-17, -3.081487911019577365E-33 ) ) ;
#26596 = B_SPLINE_CURVE_WITH_KNOTS ( 'NONE', 3,
 ( #16139, #23498, #10976, #944, #8133, #8611, #29181, #3293 ),
 .UNSPECIFIED., .F., .F.,
 ( 4, 2, 2, 4 ),
 ( 0.000000000000000000, 0.0003782825618925954618, 0.0005674238428388933553, 0.0007565651237851912488 ),
 .UNSPECIFIED. ) ;
#26597 = DIRECTION ( 'NONE',  ( -1.000000000000000000, 0.000000000000000000, 0.000000000000000000 ) ) ;
#26598 = CARTESIAN_POINT ( 'NONE',  ( -2.767073886773233848, -0.6621507858625382825, -1.748408842879326075 ) ) ;
#26599 = CARTESIAN_POINT ( 'NONE',  ( 12.44989959798877699, 0.5174497483512504603, 2.981930256614307329 ) ) ;
#26600 = CARTESIAN_POINT ( 'NONE',  ( 9.288430967222316426, 0.2258737065014515821, 1.045938632499123999 ) ) ;
#26601 = CARTESIAN_POINT ( 'NONE',  ( 107.8717334959377609, -16.22235636681381621, 1.414040860148557677 ) ) ;
#26602 = EDGE_LOOP ( 'NONE', ( #24123, #24343, #2947, #12864 ) ) ;
#26603 = EDGE_CURVE ( 'NONE', #6904, #32600, #7899, .T. ) ;
#26604 = CARTESIAN_POINT ( 'NONE',  ( 20.75046113880689092, -21.62010873700215541, 1.554218361998283227 ) ) ;
#26605 = EDGE_CURVE ( 'NONE', #9995, #5270, #22559, .T. ) ;
#26606 = FACE_OUTER_BOUND ( 'NONE', #22700, .T. ) ;
#26608 = CARTESIAN_POINT ( 'NONE',  ( 107.9476209416900474, -17.31511670722516882, 4.492030933741832044 ) ) ;
#26607 = DIRECTION ( 'NONE',  ( -0.4999999999999977240, -0.8660254037844398178, 0.000000000000000000 ) ) ;
#26609 = VERTEX_POINT ( 'NONE', #27627 ) ;
#26610 = EDGE_LOOP ( 'NONE', ( #10624, #8943, #16482, #30251 ) ) ;
#26611 = DIRECTION ( 'NONE',  ( 0.000000000000000000, 0.5735764363510391650, 0.8191520442889965725 ) ) ;
#26613 = VERTEX_POINT ( 'NONE', #11469 ) ;
#26612 = CARTESIAN_POINT ( 'NONE',  ( 84.96567518654291007, -4.060553804896915864, -3.995969900420532461 ) ) ;
#26614 = ORIENTED_EDGE ( 'NONE', *, *, #15967, .F. ) ;
#26615 = DIRECTION ( 'NONE',  ( 1.000000000000000000, -8.574039729943018344E-17, -0.000000000000000000 ) ) ;
#26616 = DIRECTION ( 'NONE',  ( -1.000000000000000000, -0.000000000000000000, -0.000000000000000000 ) ) ;
#26618 = ORIENTED_EDGE ( 'NONE', *, *, #25703, .T. ) ;
#26617 = DIRECTION ( 'NONE',  ( -1.000000000000000000, 8.574039729943018344E-17, -0.000000000000000000 ) ) ;
#26619 = CARTESIAN_POINT ( 'NONE',  ( 13.87075382900347975, 7.736340727340449419, -1.050000000000000044 ) ) ;
#26620 = CARTESIAN_POINT ( 'NONE',  ( 17.39502519979081185, -21.04076415203811479, -1.751145182513948573 ) ) ;
#26621 = CARTESIAN_POINT ( 'NONE',  ( 108.0549841752498565, -18.86112056187526775, -3.563976902055589147 ) ) ;
#26622 = CARTESIAN_POINT ( 'NONE',  ( 10.63777812034630976, -12.44241537516159113, -1.000000000000000000 ) ) ;
#26623 = DIRECTION ( 'NONE',  ( 1.000000000000000000, -8.574039729943018344E-17, -0.000000000000000000 ) ) ;
#26624 = DIRECTION ( 'NONE',  ( 0.1436597682917715446, 0.03489949670250103858, -0.9890115753135888532 ) ) ;
#26625 = CARTESIAN_POINT ( 'NONE',  ( 24.86000000273118715, -1.942864903642428587, -1.573300977624592756 ) ) ;
#26626 = CARTESIAN_POINT ( 'NONE',  ( 41.35220755422911054, -6.766095577562686536, 3.993434768846746419 ) ) ;
#26627 = CARTESIAN_POINT ( 'NONE',  ( -3.050050800000000617, -2.853674364686378695, -1.549418761218566809 ) ) ;
#26628 = DIRECTION ( 'NONE',  ( 0.000000000000000000, -1.000000000000000000, -1.040834085586083626E-14 ) ) ;
#26629 = ORIENTED_EDGE ( 'NONE', *, *, #12012, .F. ) ;
#26630 = LINE ( 'NONE', #19113, #11895 ) ;
#26631 = CARTESIAN_POINT ( 'NONE',  ( -29.73484230743789070, -25.93932300454937945, 11.09540449768827308 ) ) ;
#26632 = EDGE_CURVE ( 'NONE', #31261, #3782, #21664, .T. ) ;
#26633 = DIRECTION ( 'NONE',  ( -0.04852105321274841065, 0.4695180821586825148, 0.8815886103626556780 ) ) ;
#26634 = VERTEX_POINT ( 'NONE', #19962 ) ;
#26635 = ADVANCED_FACE ( 'NONE', ( #17576 ), #1912, .T. ) ;
#26636 = EDGE_CURVE ( 'NONE', #13368, #4840, #13947, .T. ) ;
#26637 = CARTESIAN_POINT ( 'NONE',  ( -8.000050800000000351, 0.6450660259192652068, -3.401635239564149593 ) ) ;
#26638 = CARTESIAN_POINT ( 'NONE',  ( 18.73041676179872184, -21.25644754115793233, 1.734286084696329722 ) ) ;
#26639 = ORIENTED_EDGE ( 'NONE', *, *, #13719, .T. ) ;
#26640 = FACE_OUTER_BOUND ( 'NONE', #32192, .T. ) ;
#26641 = ORIENTED_EDGE ( 'NONE', *, *, #26122, .T. ) ;
#26642 = ORIENTED_EDGE ( 'NONE', *, *, #21668, .T. ) ;
#26643 = CARTESIAN_POINT ( 'NONE',  ( 19.08086296608603405, -2.273337061837030326, -1.915219082070890755 ) ) ;
#26645 = EDGE_LOOP ( 'NONE', ( #3054, #26942, #18485, #13189, #6438 ) ) ;
#26644 = CARTESIAN_POINT ( 'NONE',  ( -1.082681991931091270, 0.000000000000000000, 4.629213727441584325 ) ) ;
#26646 = ORIENTED_EDGE ( 'NONE', *, *, #28160, .F. ) ;
#26647 = ORIENTED_EDGE ( 'NONE', *, *, #11876, .F. ) ;
#26648 = CARTESIAN_POINT ( 'NONE',  ( -1.921189184902823754, -10.44034746380417467, 4.522129901861158707 ) ) ;
#26649 = CARTESIAN_POINT ( 'NONE',  ( -56.71071518287084245, 0.7496615022747109558, 1.500000000000000000 ) ) ;
#26651 = ORIENTED_EDGE ( 'NONE', *, *, #32746, .F. ) ;
#26650 = LINE ( 'NONE', #21491, #22434 ) ;
#26652 = DIRECTION ( 'NONE',  ( 0.000000000000000000, 0.000000000000000000, -1.000000000000000000 ) ) ;
#26653 = DIRECTION ( 'NONE',  ( 0.000000000000000000, -3.854941057726238689E-15, 1.000000000000000000 ) ) ;
#26654 = CARTESIAN_POINT ( 'NONE',  ( 25.75999999999999801, -2.208672634433321348E-15, 0.000000000000000000 ) ) ;
#26655 = DIRECTION ( 'NONE',  ( -0.000000000000000000, -0.000000000000000000, -1.000000000000000000 ) ) ;
#26656 = CARTESIAN_POINT ( 'NONE',  ( 10.00000000000000178, 3.024842911000690915, 3.993798362933321133 ) ) ;
#26657 = AXIS2_PLACEMENT_3D ( 'NONE', #9543, #11727, #17420 ) ;
#26658 =( BOUNDED_SURFACE ( )  B_SPLINE_SURFACE ( 3, 2, ( 
 ( #13595, #3584, #3105 ),
 ( #3434, #8421, #913 ),
 ( #5614, #11091, #23637 ),
 ( #21290, #25998, #26485 ),
 ( #31491, #7932, #5756 ),
 ( #3254, #16274, #758 ),
 ( #28661, #18614, #2959 ),
 ( #13744, #31193, #25838 ),
 ( #28806, #23461, #13116 ),
 ( #10942, #23948, #28507 ) ),
 .UNSPECIFIED., .F., .F., .F. ) 
 B_SPLINE_SURFACE_WITH_KNOTS ( ( 4, 2, 2, 2, 4 ),
 ( 3, 3 ),
 ( 0.003636727685402258142, 0.004103800047000625076, 0.004570872408598991576, 0.005037944770197358077, 0.005505017131795725445 ),
 ( 0.000000000000000000, 1.000000000000000000 ),
 .UNSPECIFIED. ) 
 GEOMETRIC_REPRESENTATION_ITEM ( )  RATIONAL_B_SPLINE_SURFACE ( (
 ( 1.000000000000000000, 0.8449619147701442623, 1.000000000000000000),
 ( 1.000000000000000000, 0.8255905392900690920, 1.000000000000000000),
 ( 1.000000000000000000, 0.8027571906106222288, 1.000000000000000000),
 ( 1.000000000000000000, 0.7529839109803591057, 1.000000000000000000),
 ( 1.000000000000000000, 0.7260803501547112848, 1.000000000000000000),
 ( 1.000000000000000000, 0.6677408092242498316, 1.000000000000000000),
 ( 1.000000000000000000, 0.6373774895460140311, 1.000000000000000000),
 ( 1.000000000000000000, 0.5732936775527678330, 1.000000000000000000),
 ( 1.000000000000000000, 0.5402556527144246612, 1.000000000000000000),
 ( 1.000000000000000000, 0.5090209295198749873, 1.000000000000000000) ) ) 
 REPRESENTATION_ITEM ( '' )  SURFACE ( )  );
#26659 = CARTESIAN_POINT ( 'NONE',  ( 0.8407900506754626413, -11.56055812333295130, -4.522129901861164925 ) ) ;
#26660 = CARTESIAN_POINT ( 'NONE',  ( 18.60402535544292490, -7.603424548862588672, -0.4367666033500683942 ) ) ;
#26661 = CARTESIAN_POINT ( 'NONE',  ( 9.149098621172164769, 18.06225657836807841, -4.612695725900421984 ) ) ;
#26662 = EDGE_CURVE ( 'NONE', #27553, #20422, #17861, .T. ) ;
#26663 = CARTESIAN_POINT ( 'NONE',  ( 5.377543748152548098, 7.530955069117513112, 2.741043480754951744 ) ) ;
#26664 = LINE ( 'NONE', #23503, #25736 ) ;
#26665 = FACE_OUTER_BOUND ( 'NONE', #21688, .T. ) ;
#26666 = CARTESIAN_POINT ( 'NONE',  ( -10.00000000000000000, 0.000000000000000000, 0.000000000000000000 ) ) ;
#26667 = CARTESIAN_POINT ( 'NONE',  ( 21.54750000000000298, -2.594547506269383685, -0.7685399846772043020 ) ) ;
#26668 = CARTESIAN_POINT ( 'NONE',  ( -5.750050802731187183, -0.3135853898029607456, 2.983565686104819648 ) ) ;
#26669 = ORIENTED_EDGE ( 'NONE', *, *, #5130, .F. ) ;
#26670 = CARTESIAN_POINT ( 'NONE',  ( -5.200050800000000528, 2.331437884370912705, -1.887961173149511618 ) ) ;
#26671 = AXIS2_PLACEMENT_3D ( 'NONE', #391, #26117, #23772 ) ;
#26672 = VECTOR ( 'NONE', #22257, 1000.000000000000000 ) ;
#26673 = CARTESIAN_POINT ( 'NONE',  ( 3.249999999999999556, -8.461683424509331530, 2.223716399045538861 ) ) ;
#26674 = CARTESIAN_POINT ( 'NONE',  ( -48.07500000000000284, -10.96966150227468972, 7.500000000000000000 ) ) ;
#26675 = DIRECTION ( 'NONE',  ( 0.000000000000000000, -0.5735764363510469366, -0.8191520442889912434 ) ) ;
#26676 = ORIENTED_EDGE ( 'NONE', *, *, #18751, .T. ) ;
#26677 = CARTESIAN_POINT ( 'NONE',  ( -7.100050799999999995, -2.983565686104819648, -0.3135853898029605791 ) ) ;
#26678 = CIRCLE ( 'NONE', #16527, 8.500000000000000000 ) ;
#26679 = EDGE_LOOP ( 'NONE', ( #29395, #23810, #19295, #9744, #29543 ) ) ;
#26680 = CARTESIAN_POINT ( 'NONE',  ( 0.4783367452032581402, -8.598034230381170318, 1.771412240841123920 ) ) ;
#26681 = DATE_TIME_ROLE ( 'creation_date' ) ;
#26682 = VERTEX_POINT ( 'NONE', #24166 ) ;
#26683 = CARTESIAN_POINT ( 'NONE',  ( 102.3836362560106465, -3.427337902231936351, 4.312042181584448741 ) ) ;
#26684 = FACE_OUTER_BOUND ( 'NONE', #4946, .T. ) ;
#26685 = CARTESIAN_POINT ( 'NONE',  ( 28.69250200978156329, -5.658193782479810530, -4.053847714210987441 ) ) ;
#26686 = CARTESIAN_POINT ( 'NONE',  ( 21.04767255914888580, -17.06392231637762436, -1.500000000000848210 ) ) ;
#26687 = FACE_OUTER_BOUND ( 'NONE', #21195, .T. ) ;
#26688 = ORIENTED_EDGE ( 'NONE', *, *, #244, .T. ) ;
#26689 = DIRECTION ( 'NONE',  ( -1.000000000000000000, -0.000000000000000000, -0.000000000000000000 ) ) ;
#26690 = CARTESIAN_POINT ( 'NONE',  ( 107.4454642110974447, 16.41225513980339912, 1.495340255777613869 ) ) ;
#26691 = CARTESIAN_POINT ( 'NONE',  ( 0.000000000000000000, 4.137773741518454784, -5.705158055754753654 ) ) ;
#26692 = VECTOR ( 'NONE', #10510, 1000.000000000000000 ) ;
#26694 = ORIENTED_EDGE ( 'NONE', *, *, #32465, .T. ) ;
#26693 = CARTESIAN_POINT ( 'NONE',  ( 25.57927635680546175, 0.4793050474504166325, -2.813602956598889815 ) ) ;
#26695 = FACE_OUTER_BOUND ( 'NONE', #23614, .T. ) ;
#26696 = AXIS2_PLACEMENT_3D ( 'NONE', #10739, #31172, #15915 ) ;
#26697 = ADVANCED_FACE ( 'NONE', ( #14590 ), #4728, .T. ) ;
#26698 = DIRECTION ( 'NONE',  ( -0.000000000000000000, 0.000000000000000000, 1.000000000000000000 ) ) ;
#26699 = CARTESIAN_POINT ( 'NONE',  ( 2.437082469501516080, -2.117184480729032092, -10.45536235038316519 ) ) ;
#26700 = PLANE ( 'NONE',  #11432 ) ;
#26701 = AXIS2_PLACEMENT_3D ( 'NONE', #8043, #30816, #18242 ) ;
#26702 = DIRECTION ( 'NONE',  ( -1.000000000000000000, 0.000000000000000000, 0.000000000000000000 ) ) ;
#26703 = CARTESIAN_POINT ( 'NONE',  ( 25.75999999999999801, -2.208672634433321348E-15, 0.000000000000000000 ) ) ;
#26704 = LINE ( 'NONE', #9137, #30597 ) ;
#26705 = CARTESIAN_POINT ( 'NONE',  ( 3.544356706772826993, -14.29624599654059303, 5.485967528433933538 ) ) ;
#26706 = ORIENTED_EDGE ( 'NONE', *, *, #6947, .F. ) ;
#26707 = EDGE_CURVE ( 'NONE', #26351, #32786, #3364, .T. ) ;
#26708 = ADVANCED_FACE ( 'NONE', ( #9401 ), #17307, .T. ) ;
#26709 = CARTESIAN_POINT ( 'NONE',  ( 23.84310522038115465, -4.329614468541457484, 4.522129901861162260 ) ) ;
#26710 = ORIENTED_EDGE ( 'NONE', *, *, #18575, .F. ) ;
#26711 = CARTESIAN_POINT ( 'NONE',  ( 3.249999999999999556, -8.461683424509297780, -2.223716399045661873 ) ) ;
#26712 = CARTESIAN_POINT ( 'NONE',  ( -58.11719619654970614, -3.766776810957159771, 5.550376981476754068 ) ) ;
#26713 = AXIS2_PLACEMENT_3D ( 'NONE', #17531, #9862, #33091 ) ;
#26714 = CARTESIAN_POINT ( 'NONE',  ( -3.937550801365593323, 3.368539882008727115, 1.828967928396027176 ) ) ;
#26715 = VECTOR ( 'NONE', #10303, 1000.000000000000000 ) ;
#26716 = CARTESIAN_POINT ( 'NONE',  ( 3.249999999999999556, 1.699438267350499521, -9.241976615262139205 ) ) ;
#26717 = DIRECTION ( 'NONE',  ( -1.000000000000000000, 0.000000000000000000, 0.000000000000000000 ) ) ;
#26718 = ORIENTED_EDGE ( 'NONE', *, *, #27807, .F. ) ;
#26719 = FACE_OUTER_BOUND ( 'NONE', #3164, .T. ) ;
#26720 = ADVANCED_FACE ( 'NONE', ( #26665 ), #3777, .T. ) ;
#26721 = AXIS2_PLACEMENT_3D ( 'NONE', #1964, #17331, #6633 ) ;
#26722 = VECTOR ( 'NONE', #71, 999.9999999999998863 ) ;
#26723 = ORIENTED_EDGE ( 'NONE', *, *, #1409, .F. ) ;
#26724 = DATE_TIME_ROLE ( 'classification_date' ) ;
#26725 = CARTESIAN_POINT ( 'NONE',  ( 69.07037654389817760, -6.114898606693179417, 3.995971199216228786 ) ) ;
#26726 = ADVANCED_FACE ( 'NONE', ( #20450 ), #25452, .F. ) ;
#26727 = CIRCLE ( 'NONE', #30503, 8.750000000000000000 ) ;
#26728 = CARTESIAN_POINT ( 'NONE',  ( 7.151900074888314585, -6.858124901741749824, -0.9999999999999997780 ) ) ;
#26729 = VERTEX_POINT ( 'NONE', #25606 ) ;
#26730 = CARTESIAN_POINT ( 'NONE',  ( 0.3045634671936391369, -10.22982953726848265, 0.9829946734954320142 ) ) ;
#26731 = EDGE_LOOP ( 'NONE', ( #3123, #7622, #22836, #29491, #19594, #13535, #50, #10110 ) ) ;
#26732 = ORIENTED_EDGE ( 'NONE', *, *, #21351, .F. ) ;
#26733 = CARTESIAN_POINT ( 'NONE',  ( 6.883866621640343908, 6.224335161395018190, 6.123537914202261234 ) ) ;
#26734 = CARTESIAN_POINT ( 'NONE',  ( -5.262550801365593500, -0.3701630799359326152, 3.521866450007987037 ) ) ;
#26735 = CARTESIAN_POINT ( 'NONE',  ( 24.67249999999999943, -1.291182301015472378, -2.378061970571982098 ) ) ;
#26736 = DIRECTION ( 'NONE',  ( 0.000000000000000000, 0.000000000000000000, -1.000000000000000000 ) ) ;
#26738 = EDGE_LOOP ( 'NONE', ( #1894, #6009, #11104, #24376 ) ) ;
#26737 = LINE ( 'NONE', #26584, #5891 ) ;
#26739 = CARTESIAN_POINT ( 'NONE',  ( -5.487550801365593145, 2.228590825266444142, 2.752080473201636845 ) ) ;
#26740 = VECTOR ( 'NONE', #16143, 1000.000000000000000 ) ;
#26741 = CARTESIAN_POINT ( 'NONE',  ( 6.038144853276842916, 1.911563584435307162, -8.256557579931646629 ) ) ;
#26742 = DIRECTION ( 'NONE',  ( 2.219124775574956535E-17, 0.2588190451025241812, -0.9659258262890673130 ) ) ;
#26743 = ORIENTED_EDGE ( 'NONE', *, *, #27238, .F. ) ;
#26745 = ORIENTED_EDGE ( 'NONE', *, *, #30625, .T. ) ;
#26744 = CARTESIAN_POINT ( 'NONE',  ( 5.489321676144492734, -6.978593840069416743, -4.149060317827578892 ) ) ;
#26746 = AXIS2_PLACEMENT_3D ( 'NONE', #20304, #30857, #2089 ) ;
#26747 = AXIS2_PLACEMENT_3D ( 'NONE', #29073, #28726, #15999 ) ;
#26748 = AXIS2_PLACEMENT_3D ( 'NONE', #27532, #27854, #4630 ) ;
#26749 = CARTESIAN_POINT ( 'NONE',  ( 20.92250000273118360, -1.291182301015472378, -2.378061970571982098 ) ) ;
#26750 = ADVANCED_FACE ( 'NONE', ( #20270 ), #20966, .T. ) ;
#26751 = EDGE_CURVE ( 'NONE', #5304, #24201, #11336, .T. ) ;
#26752 = CARTESIAN_POINT ( 'NONE',  ( 25.36291108019387863, -17.54678858634073890, 1.252583955065272425 ) ) ;
#26753 = CARTESIAN_POINT ( 'NONE',  ( 17.32050807568873552, 10.00000000000002309, 0.000000000000000000 ) ) ;
#26754 = CARTESIAN_POINT ( 'NONE',  ( -4.555723515433391491, -6.511021237588678012, -1.499999999999999556 ) ) ;
#26755 = VECTOR ( 'NONE', #20639, 1000.000000000000000 ) ;
#26756 = DIRECTION ( 'NONE',  ( 0.000000000000000000, 0.000000000000000000, 1.000000000000000000 ) ) ;
#26757 = CARTESIAN_POINT ( 'NONE',  ( 5.377543748152548098, 8.385837730238846314E-14, -8.014274990069656823 ) ) ;
#26758 = CARTESIAN_POINT ( 'NONE',  ( -3.237550801365593589, 3.675193018007247403, -1.088641768524161391 ) ) ;
#26759 = DIRECTION ( 'NONE',  ( 0.000000000000000000, 0.000000000000000000, -1.000000000000000000 ) ) ;
#26760 = ORIENTED_EDGE ( 'NONE', *, *, #32831, .T. ) ;
#26761 = CARTESIAN_POINT ( 'NONE',  ( 0.7632845268398871230, 0.000000000000000000, 0.000000000000000000 ) ) ;
#26762 = VECTOR ( 'NONE', #26521, 1000.000000000000000 ) ;
#26763 = LINE ( 'NONE', #28957, #3417 ) ;
#26765 = CARTESIAN_POINT ( 'NONE',  ( 107.6996442589673819, 19.35565155597529596, -4.612695725900422872 ) ) ;
#26764 = DIRECTION ( 'NONE',  ( 0.000000000000000000, 0.000000000000000000, -1.000000000000000000 ) ) ;
#26766 = EDGE_LOOP ( 'NONE', ( #5089, #14892, #5802, #13684, #13315 ) ) ;
#26767 = AXIS2_PLACEMENT_3D ( 'NONE', #28411, #8007, #10672 ) ;
#26769 = EDGE_CURVE ( 'NONE', #19049, #6820, #25226, .T. ) ;
#26768 = AXIS2_PLACEMENT_3D ( 'NONE', #22478, #14779, #6921 ) ;
#26770 = CARTESIAN_POINT ( 'NONE',  ( 18.66634262892177532, -21.55284492811545860, 1.491166157331047293 ) ) ;
#26771 = AXIS2_PLACEMENT_3D ( 'NONE', #32245, #9308, #3806 ) ;
#26772 = ORIENTED_EDGE ( 'NONE', *, *, #12326, .T. ) ;
#26773 = CARTESIAN_POINT ( 'NONE',  ( -50.60000000000000142, -0.5000000000000000000, 1.000000000000000000 ) ) ;
#26775 = ORIENTED_EDGE ( 'NONE', *, *, #32172, .T. ) ;
#26774 = CARTESIAN_POINT ( 'NONE',  ( 40.87774520873607287, -5.751096254936027385, -3.997238040213327626 ) ) ;
#26776 = ORIENTED_EDGE ( 'NONE', *, *, #29892, .T. ) ;
#26777 = CYLINDRICAL_SURFACE ( 'NONE', #25184, 2.499999999999997780 ) ;
#26778 = AXIS2_PLACEMENT_3D ( 'NONE', #27998, #405, #5415 ) ;
#26779 = VECTOR ( 'NONE', #5005, 1000.000000000000000 ) ;
#26780 = CARTESIAN_POINT ( 'NONE',  ( -17.45597128428592981, -25.43932300454937234, 11.50000000000000000 ) ) ;
#26782 = VERTEX_POINT ( 'NONE', #18434 ) ;
#26781 = DIRECTION ( 'NONE',  ( 1.000000000000000000, -0.000000000000000000, -0.000000000000000000 ) ) ;
#26783 = CARTESIAN_POINT ( 'NONE',  ( 15.90893862193319386, 10.93205754319533263, -1.050000000000000044 ) ) ;
#26784 = CARTESIAN_POINT ( 'NONE',  ( -3.790542665135919531, -3.338451600437029931, -1.747101525495873053 ) ) ;
#26785 = B_SPLINE_CURVE_WITH_KNOTS ( 'NONE', 3,
 ( #2082, #22466, #30502, #32683, #9764, #7586, #30187, #9929 ),
 .UNSPECIFIED., .F., .F.,
 ( 4, 2, 2, 4 ),
 ( 2.213836054414765521E-07, 0.001227982086136578848, 0.001841862437402150407, 0.002455742788667721749 ),
 .UNSPECIFIED. ) ;
#26786 = FACE_OUTER_BOUND ( 'NONE', #24223, .T. ) ;
#26787 = CARTESIAN_POINT ( 'NONE',  ( 9.360049167874114673, -11.53021799246534584, -1.000000000000000000 ) ) ;
#26789 = ORIENTED_EDGE ( 'NONE', *, *, #11160, .T. ) ;
#26788 = CARTESIAN_POINT ( 'NONE',  ( -2.962942409646513564, 4.884725290497410777E-15, -2.999999999999999556 ) ) ;
#26790 = CARTESIAN_POINT ( 'NONE',  ( 7.249760686538667009, 3.647351267791570262, 7.953573330858228374 ) ) ;
#26791 = EDGE_CURVE ( 'NONE', #12161, #6820, #20617, .T. ) ;
#26792 = AXIS2_PLACEMENT_3D ( 'NONE', #16093, #26327, #16273 ) ;
#26793 = CARTESIAN_POINT ( 'NONE',  ( -4.058229847495222268E-16, -1.825746869171931852, 4.518882073553349699 ) ) ;
#26794 = AXIS2_PLACEMENT_3D ( 'NONE', #17355, #4644, #25018 ) ;
#26795 = CARTESIAN_POINT ( 'NONE',  ( -2.962992063741595405, -11.77309494928644185, 1.500000000000000000 ) ) ;
#26796 = CARTESIAN_POINT ( 'NONE',  ( 0.6728002192015016814, -5.823680980849866629, 7.058361986489762430 ) ) ;
#26797 = ORIENTED_EDGE ( 'NONE', *, *, #25340, .T. ) ;
#26798 = DIRECTION ( 'NONE',  ( -0.000000000000000000, -0.000000000000000000, 1.000000000000000000 ) ) ;
#26799 = AXIS2_PLACEMENT_3D ( 'NONE', #27618, #27278, #9722 ) ;
#26800 = VECTOR ( 'NONE', #11531, 1000.000000000000000 ) ;
#26801 = CARTESIAN_POINT ( 'NONE',  ( 107.3578191293706396, -16.03232060375378154, -1.799467592163734642 ) ) ;
#26802 = DIRECTION ( 'NONE',  ( 0.000000000000000000, -0.8191520442889927978, -0.5735764363510448272 ) ) ;
#26803 = EDGE_LOOP ( 'NONE', ( #688, #305, #27635, #12100 ) ) ;
#26804 = AXIS2_PLACEMENT_3D ( 'NONE', #2784, #2973, #104 ) ;
#26805 = B_SPLINE_CURVE_WITH_KNOTS ( 'NONE', 3,
 ( #1811, #3805, #8820, #6955, #14470, #1469 ),
 .UNSPECIFIED., .F., .F.,
 ( 4, 2, 4 ),
 ( -5.641427396388729422E-06, 0.0003847768015433646440, 0.0007751950304831179903 ),
 .UNSPECIFIED. ) ;
#26806 = CARTESIAN_POINT ( 'NONE',  ( -8.000050800000000351, 0.3588475416126519768, -3.414206294404568798 ) ) ;
#26807 = CARTESIAN_POINT ( 'NONE',  ( 110.0816933595962439, 17.77332459904788209, -5.396302277755718357 ) ) ;
#26808 = ORIENTED_EDGE ( 'NONE', *, *, #13686, .F. ) ;
#26809 = CARTESIAN_POINT ( 'NONE',  ( 6.357668022120091855, 6.947679035623525401, -5.080751859797282499 ) ) ;
#26810 = ORIENTED_EDGE ( 'NONE', *, *, #5540, .T. ) ;
#26811 = CIRCLE ( 'NONE', #5475, 5.009999999999999787 ) ;
#26812 = ORIENTED_EDGE ( 'NONE', *, *, #16861, .F. ) ;
#26813 = CARTESIAN_POINT ( 'NONE',  ( 25.38273381070351320, -17.54867692718865868, -1.149837904939237321 ) ) ;
#26814 = CIRCLE ( 'NONE', #18285, 2.999999999999999556 ) ;
#26816 = ORIENTED_EDGE ( 'NONE', *, *, #21617, .T. ) ;
#26815 = CARTESIAN_POINT ( 'NONE',  ( 3.499999999999999556, -4.724769925181146135, -4.089810527897805414 ) ) ;
#26817 = ORIENTED_EDGE ( 'NONE', *, *, #9776, .F. ) ;
#26818 = DIRECTION ( 'NONE',  ( 1.000000000000000000, -8.574039729943018344E-17, -0.000000000000000000 ) ) ;
#26819 = AXIS2_PLACEMENT_3D ( 'NONE', #26281, #22933, #21111 ) ;
#26820 = VERTEX_POINT ( 'NONE', #25959 ) ;
#26821 = CARTESIAN_POINT ( 'NONE',  ( 9.331062908042598636, 15.00000000000002132, 4.629213727441584325 ) ) ;
#26822 = CARTESIAN_POINT ( 'NONE',  ( 0.6791197550704605179, 2.303133748654099033, -8.860977624947469877 ) ) ;
#26824 = VERTEX_POINT ( 'NONE', #3067 ) ;
#26823 = LINE ( 'NONE', #11606, #19238 ) ;
#26825 = DIRECTION ( 'NONE',  ( 0.000000000000000000, 0.000000000000000000, 1.000000000000000000 ) ) ;
#26826 = DIRECTION ( 'NONE',  ( 1.000000000000000000, 0.000000000000000000, 0.000000000000000000 ) ) ;
#26827 = AXIS2_PLACEMENT_3D ( 'NONE', #14886, #27765, #4879 ) ;
#26828 = VECTOR ( 'NONE', #30250, 1000.000000000000000 ) ;
#26829 = ADVANCED_FACE ( 'NONE', ( #5224 ), #25293, .T. ) ;
#26830 = CARTESIAN_POINT ( 'NONE',  ( 6.883866482134012976, 0.8319830743950653584, 8.691827696555161964 ) ) ;
#26831 = DIRECTION ( 'NONE',  ( 1.000000000000000000, -0.000000000000000000, -0.000000000000000000 ) ) ;
#26832 = EDGE_CURVE ( 'NONE', #22618, #21128, #18084, .T. ) ;
#26834 = CARTESIAN_POINT ( 'NONE',  ( 107.5605484478042655, -18.96584416766395620, 4.567556099746715503 ) ) ;
#26833 = CIRCLE ( 'NONE', #15086, 2.999999999999998668 ) ;
#26835 = EDGE_CURVE ( 'NONE', #7472, #12927, #21485, .T. ) ;
#26836 = LINE ( 'NONE', #24327, #10269 ) ;
#26837 = CARTESIAN_POINT ( 'NONE',  ( 47.62814091865205768, 23.65599663307499156, 4.629213727441585213 ) ) ;
#26838 = CARTESIAN_POINT ( 'NONE',  ( 3.500000000000000000, 0.000000000000000000, 6.000000000000000000 ) ) ;
#26839 = CARTESIAN_POINT ( 'NONE',  ( 10.56870887191539587, 4.616489984850530526, 1.946309384392607811 ) ) ;
#26840 = VECTOR ( 'NONE', #30951, 999.9999999999998863 ) ;
#26841 = DIRECTION ( 'NONE',  ( 0.03662738895564522645, -0.5274252892134372317, -0.8488115212910425367 ) ) ;
#26842 = CARTESIAN_POINT ( 'NONE',  ( 102.7595417042496706, -3.401262957566509204, 3.636029349014984202 ) ) ;
#26843 = CIRCLE ( 'NONE', #12432, 5.009999999999999787 ) ;
#26844 = CIRCLE ( 'NONE', #23650, 0.5000000000000004441 ) ;
#26845 = LINE ( 'NONE', #19325, #3873 ) ;
#26846 = CARTESIAN_POINT ( 'NONE',  ( -5.800050802731187005, 0.9222479816126443186, 3.113457007523260156 ) ) ;
#26847 = ORIENTED_EDGE ( 'NONE', *, *, #568, .T. ) ;
#26848 = CIRCLE ( 'NONE', #4435, 5.000000000000001776 ) ;
#26849 = CIRCLE ( 'NONE', #20993, 11.00000000000000000 ) ;
#26850 = CARTESIAN_POINT ( 'NONE',  ( -7.700050800000000528, 0.3135853898029611342, -2.983565686104819648 ) ) ;
#26851 = CARTESIAN_POINT ( 'NONE',  ( 3.063284526839887167, -4.729683950898817102, -7.360373001730970977 ) ) ;
#26852 = CARTESIAN_POINT ( 'NONE',  ( 40.73236281613230148, -5.747100024567912691, -3.993433057586367241 ) ) ;
#26853 = CARTESIAN_POINT ( 'NONE',  ( 7.362531901230354947, -8.542914936813595261, 1.500000000000000000 ) ) ;
#26854 = AXIS2_PLACEMENT_3D ( 'NONE', #19585, #21473, #6859 ) ;
#26855 = VERTEX_POINT ( 'NONE', #30823 ) ;
#26856 = LINE ( 'NONE', #29703, #719 ) ;
#26857 = ORIENTED_EDGE ( 'NONE', *, *, #24656, .T. ) ;
#26858 = CARTESIAN_POINT ( 'NONE',  ( 3.163725240263005389, -11.65225984964322947, 1.500000000000000888 ) ) ;
#26859 = MECHANICAL_CONTEXT ( 'NONE', #25059, 'mechanical' ) ;
#26860 = CARTESIAN_POINT ( 'NONE',  ( 5.885541838704151374, 5.674471607902439985, 6.185046950422337986 ) ) ;
#26861 = ORIENTED_EDGE ( 'NONE', *, *, #6785, .T. ) ;
#26862 = CARTESIAN_POINT ( 'NONE',  ( 84.96557803822085475, -4.058969597120936079, 3.993433529938030357 ) ) ;
#26863 = CARTESIAN_POINT ( 'NONE',  ( -5.800050800000000173, 1.887961173149511618, 2.331437884370912705 ) ) ;
#26864 = AXIS2_PLACEMENT_3D ( 'NONE', #26482, #16269, #19268 ) ;
#26865 = CARTESIAN_POINT ( 'NONE',  ( 28.69116527693491392, -5.709888947837792550, -4.112224495657437195 ) ) ;
#26866 = DIRECTION ( 'NONE',  ( -1.000000000000000000, 0.000000000000000000, 0.000000000000000000 ) ) ;
#26867 = CARTESIAN_POINT ( 'NONE',  ( 0.000000000000000000, 5.241389472434663688, 4.711457988287072851 ) ) ;
#26868 = AXIS2_PLACEMENT_3D ( 'NONE', #29195, #6283, #14139 ) ;
#26869 = EDGE_LOOP ( 'NONE', ( #10198, #8409, #6867, #11518 ) ) ;
#26870 = TOROIDAL_SURFACE ( 'NONE', #21021, 7.144028715714068056, 0.5000000000000000000 ) ;
#26871 = ADVANCED_FACE ( 'NONE', ( #23422 ), #9731, .T. ) ;
#26872 = CARTESIAN_POINT ( 'NONE',  ( 8.914564461877747092, -1.485421493711411364E-07, 1.044418714689500538 ) ) ;
#26873 = LINE ( 'NONE', #1470, #17707 ) ;
#26874 = AXIS2_PLACEMENT_3D ( 'NONE', #5042, #15219, #27595 ) ;
#26875 = LINE ( 'NONE', #21691, #31146 ) ;
#26877 = EDGE_CURVE ( 'NONE', #29734, #30501, #28274, .T. ) ;
#26876 = AXIS2_PLACEMENT_3D ( 'NONE', #6035, #16231, #26589 ) ;
#26878 = B_SPLINE_CURVE_WITH_KNOTS ( 'NONE', 3,
 ( #24155, #21655, #31862, #14122, #3949, #27001 ),
 .UNSPECIFIED., .F., .F.,
 ( 4, 2, 4 ),
 ( 0.000000000000000000, 0.001111101121321064278, 0.002222202242642128556 ),
 .UNSPECIFIED. ) ;
#26880 = ORIENTED_EDGE ( 'NONE', *, *, #22237, .F. ) ;
#26879 = DIRECTION ( 'NONE',  ( 0.03487826274237464802, -0.9987827659587182882, 0.03487826274237493945 ) ) ;
#26881 = DIRECTION ( 'NONE',  ( -1.000000000000000000, 0.000000000000000000, -0.000000000000000000 ) ) ;
#26882 = CARTESIAN_POINT ( 'NONE',  ( 20.79750000136559507, 0.3178988483021036315, 3.024605502323848949 ) ) ;
#26883 = CARTESIAN_POINT ( 'NONE',  ( 71.84273455771214856, -21.42499078636276622, -4.522129901861166701 ) ) ;
#26884 = CARTESIAN_POINT ( 'NONE',  ( 26.04364899819628576, 19.05268753777025026, 1.166395880049359457 ) ) ;
#26885 = CARTESIAN_POINT ( 'NONE',  ( -56.27770248097862549, -0.0003384977252891612984, 0.000000000000000000 ) ) ;
#26886 = CC_DESIGN_APPROVAL ( #29060, ( #1899 ) ) ;
#26887 = LINE ( 'NONE', #21700, #28975 ) ;
#26888 = CARTESIAN_POINT ( 'NONE',  ( 25.43628654896339114, -17.54453578616444887, -1.025162786324184117 ) ) ;
#26889 = CARTESIAN_POINT ( 'NONE',  ( 24.42250000273118715, 1.291182301015469047, 2.378061970571981654 ) ) ;
#26890 = DIRECTION ( 'NONE',  ( 0.000000000000000000, 0.4226182617407097108, -0.9063077870366451627 ) ) ;
#26891 = EDGE_LOOP ( 'NONE', ( #13569, #27987, #23444, #8461 ) ) ;
#26892 = LINE ( 'NONE', #1831, #18313 ) ;
#26893 = EDGE_LOOP ( 'NONE', ( #1422, #5239, #10992, #5325 ) ) ;
#26894 = LINE ( 'NONE', #22046, #27905 ) ;
#26895 = AXIS2_PLACEMENT_3D ( 'NONE', #2557, #12724, #25954 ) ;
#26896 = CARTESIAN_POINT ( 'NONE',  ( -1.394036994807583480E-16, -1.625881193364668409, -4.467071865485488402 ) ) ;
#26897 = AXIS2_PLACEMENT_3D ( 'NONE', #27033, #26689, #19678 ) ;
#26898 =( BOUNDED_CURVE ( )  B_SPLINE_CURVE ( 2, ( #21139, #15788, #14202, #16089, #11695, #8271, #21893, #8086, #5608, #3251, #564 ),
 .UNSPECIFIED., .F., .F. ) 
 B_SPLINE_CURVE_WITH_KNOTS ( ( 3, 2, 2, 2, 2, 3 ),
 ( 0.2478822619934377414, 0.2500000000000000000, 0.2656250000000000000, 0.2812500000000000000, 0.2968750000000000000, 0.3103822619934377136 ),
 .UNSPECIFIED. ) 
 CURVE ( )  GEOMETRIC_REPRESENTATION_ITEM ( )  RATIONAL_B_SPLINE_CURVE ( ( 0.9821626249036861100, 0.9896829947469993893, 1.000000000000000000, 0.9238795325112867385, 1.000000000000000000, 0.9238795325112867385, 1.000000000000000000, 0.9238795325112867385, 1.000000000000000000, 0.9341965377642874602, 0.9821626249036857770 ) ) 
 REPRESENTATION_ITEM ( '' )  );
#26899 = CARTESIAN_POINT ( 'NONE',  ( 41.44567272411835290, -7.615257740949710197, -4.522129901861164036 ) ) ;
#26900 = AXIS2_PLACEMENT_3D ( 'NONE', #30359, #5117, #25659 ) ;
#26901 = CARTESIAN_POINT ( 'NONE',  ( 0.7632845268398871230, -8.734705317681623171, -0.4999240074895356933 ) ) ;
#26902 = CARTESIAN_POINT ( 'NONE',  ( 0.7212197917546229187, -4.829101774923286072, -7.537903528366462602 ) ) ;
#26903 = EDGE_LOOP ( 'NONE', ( #21998, #30140, #8551 ) ) ;
#26904 = CARTESIAN_POINT ( 'NONE',  ( -58.35662399578649939, -4.056783446705964025, 5.700525030782698011 ) ) ;
#26906 = ADVANCED_FACE ( 'NONE', ( #10227 ), #4890, .T. ) ;
#26905 = ORIENTED_EDGE ( 'NONE', *, *, #27156, .F. ) ;
#26907 = APPROVAL_STATUS ( 'not_yet_approved' ) ;
#26909 = CARTESIAN_POINT ( 'NONE',  ( 28.66413209314083588, -6.764116340039933561, 3.995336671804473383 ) ) ;
#26908 = CC_DESIGN_APPROVAL ( #19229, ( #2373 ) ) ;
#26910 = EDGE_CURVE ( 'NONE', #660, #6261, #10406, .T. ) ;
#26911 = CARTESIAN_POINT ( 'NONE',  ( 9.052197806735183150, -0.5587348279125937678, -0.9999999999999997780 ) ) ;
#26912 = EDGE_LOOP ( 'NONE', ( #24818, #8079, #25160, #20723 ) ) ;
#26913 = CARTESIAN_POINT ( 'NONE',  ( 5.377543748152548986, 4.007137495034812424, 6.940565734314612101 ) ) ;
#26914 = VERTEX_POINT ( 'NONE', #13080 ) ;
#26915 = ORIENTED_EDGE ( 'NONE', *, *, #28979, .T. ) ;
#26916 = DIRECTION ( 'NONE',  ( 0.000000000000000000, 0.4226182617406930020, 0.9063077870366529343 ) ) ;
#26917 = LINE ( 'NONE', #27067, #608 ) ;
#26918 = CARTESIAN_POINT ( 'NONE',  ( 23.23500000000000298, 0.2613211581691317065, 2.486304738420681559 ) ) ;
#26919 = CARTESIAN_POINT ( 'NONE',  ( 2.281627749324421472, -0.2935656086769634077, -1.757435426329174044 ) ) ;
#26921 = ORIENTED_EDGE ( 'NONE', *, *, #14666, .F. ) ;
#26920 = CARTESIAN_POINT ( 'NONE',  ( 10.52034268205830614, 3.641590349731970822, -3.055657119358763829 ) ) ;
#26922 = AXIS2_PLACEMENT_3D ( 'NONE', #18156, #18343, #28361 ) ;
#26923 = CARTESIAN_POINT ( 'NONE',  ( -7.937550801365594211, 3.368539882008727115, 1.828967928396026954 ) ) ;
#26924 = DIRECTION ( 'NONE',  ( 0.000000000000000000, 0.000000000000000000, -1.000000000000000000 ) ) ;
#26925 = EDGE_CURVE ( 'NONE', #9445, #16287, #13453, .T. ) ;
#26926 = DIRECTION ( 'NONE',  ( 0.000000000000000000, -0.4226182617406906705, -0.9063077870366540445 ) ) ;
#26927 = DIRECTION ( 'NONE',  ( 1.000000000000000000, -0.000000000000000000, -0.000000000000000000 ) ) ;
#26928 = ORIENTED_EDGE ( 'NONE', *, *, #13019, .F. ) ;
#26930 = ORIENTED_EDGE ( 'NONE', *, *, #1166, .F. ) ;
#26929 = CARTESIAN_POINT ( 'NONE',  ( 12.84684103081497142, 21.67296960808364403, 1.472725903438507844 ) ) ;
#26931 = DIRECTION ( 'NONE',  ( 0.000000000000000000, 0.2588190451025139671, 0.9659258262890701996 ) ) ;
#26932 = CARTESIAN_POINT ( 'NONE',  ( 22.04750000273119070, 0.7685399846772009713, -2.594547506269381909 ) ) ;
#26933 = EDGE_CURVE ( 'NONE', #13010, #23377, #31153, .T. ) ;
#26934 = ORGANIZATION ( 'NAUO-ORG1', 'UNSPECIFIED', 'UNSPECIFIED' ) ;
#26935 = CARTESIAN_POINT ( 'NONE',  ( -16.60354855507976524, 13.22775097665246946, 1.500000000000000000 ) ) ;
#26936 = DIRECTION ( 'NONE',  ( -0.000000000000000000, 0.000000000000000000, 1.000000000000000000 ) ) ;
#26937 = CARTESIAN_POINT ( 'NONE',  ( -2.880987360464339009, -0.6119841066606575009, -1.500000000000000222 ) ) ;
#26938 = CARTESIAN_POINT ( 'NONE',  ( -32.06740601709051930, -27.93932300454937590, -0.9045955023117255855 ) ) ;
#26939 = CARTESIAN_POINT ( 'NONE',  ( 29.32642088966447602, -4.109531239332479657, 1.873788766282109552 ) ) ;
#26940 = FACE_OUTER_BOUND ( 'NONE', #20141, .T. ) ;
#26941 = DIRECTION ( 'NONE',  ( -0.1027947991993877902, 0.9947025833170222153, 0.000000000000000000 ) ) ;
#26942 = ORIENTED_EDGE ( 'NONE', *, *, #28056, .T. ) ;
#26943 = ADVANCED_FACE ( 'NONE', ( #31796 ), #16385, .T. ) ;
#26944 = CARTESIAN_POINT ( 'NONE',  ( 107.4500373638804120, -17.36019379023677089, -4.522129901861164036 ) ) ;
#26945 = EDGE_CURVE ( 'NONE', #19623, #12441, #19073, .T. ) ;
#26946 = DIRECTION ( 'NONE',  ( 0.7222222222222246524, 0.000000000000000000, -0.6916610887771492688 ) ) ;
#26948 = CARTESIAN_POINT ( 'NONE',  ( 5.489321676144491846, -7.082488557107319949, 3.969109389279940725 ) ) ;
#26947 = CARTESIAN_POINT ( 'NONE',  ( -3.500050800000000351, 2.983565686104819648, 0.3135853898029609677 ) ) ;
#26949 = ORIENTED_EDGE ( 'NONE', *, *, #4698, .T. ) ;
#26950 = DIRECTION ( 'NONE',  ( 1.000000000000000000, 0.000000000000000000, 0.000000000000000000 ) ) ;
#26951 = ORIENTED_EDGE ( 'NONE', *, *, #1091, .F. ) ;
#26952 = DIRECTION ( 'NONE',  ( 0.000000000000000000, 0.000000000000000000, -1.000000000000000000 ) ) ;
#26954 = ORIENTED_EDGE ( 'NONE', *, *, #29522, .F. ) ;
#26953 = CARTESIAN_POINT ( 'NONE',  ( 69.01326405434069500, -4.970996605387691503, -3.995007138417703718 ) ) ;
#26955 = VERTEX_POINT ( 'NONE', #14045 ) ;
#26956 = EDGE_CURVE ( 'NONE', #502, #6248, #29263, .T. ) ;
#26957 = EDGE_CURVE ( 'NONE', #19352, #32781, #6349, .T. ) ;
#26958 = CARTESIAN_POINT ( 'NONE',  ( 23.30656763371926488, -0.8852964313267484009, 2.499999999999997780 ) ) ;
#26959 = CARTESIAN_POINT ( 'NONE',  ( 4.749760686538667009, -2.741043480754877582, -7.530955069117540646 ) ) ;
#26961 = ORIENTED_EDGE ( 'NONE', *, *, #33077, .T. ) ;
#26960 = FACE_OUTER_BOUND ( 'NONE', #7563, .T. ) ;
#26962 = CARTESIAN_POINT ( 'NONE',  ( 15.60185111400613600, 10.48692277187139155, -1.050000000000000044 ) ) ;
#26963 = CARTESIAN_POINT ( 'NONE',  ( 22.61000000000000298, -1.942864903642428587, -1.573300977624592756 ) ) ;
#26964 = CARTESIAN_POINT ( 'NONE',  ( -15.09999999999999609, -21.93932300455815820, 1.000000000000000000 ) ) ;
#26965 = CARTESIAN_POINT ( 'NONE',  ( 12.29359089006071137, -13.32350401976880327, -1.500000000000554889 ) ) ;
#26966 = EDGE_CURVE ( 'NONE', #15085, #21907, #5720, .T. ) ;
#26968 = VERTEX_POINT ( 'NONE', #18925 ) ;
#26967 = CARTESIAN_POINT ( 'NONE',  ( 107.5410504431967240, -18.68278515834781928, -4.957602148651905516 ) ) ;
#26969 = DIRECTION ( 'NONE',  ( 0.000000000000000000, 0.000000000000000000, -1.000000000000000000 ) ) ;
#26970 = CARTESIAN_POINT ( 'NONE',  ( 24.92250000273118360, -1.291182301015472600, -2.378061970571982098 ) ) ;
#26971 = CARTESIAN_POINT ( 'NONE',  ( -8.049676575031998738, 0.000000000000000000, 0.000000000000000000 ) ) ;
#26972 = EDGE_CURVE ( 'NONE', #12444, #12204, #7072, .T. ) ;
#26973 = DIRECTION ( 'NONE',  ( 0.000000000000000000, 0.9993908270190956511, 0.03489949670250104552 ) ) ;
#26974 = FACE_OUTER_BOUND ( 'NONE', #10460, .T. ) ;
#26975 = EDGE_LOOP ( 'NONE', ( #8108, #14378, #18905 ) ) ;
#26976 = CARTESIAN_POINT ( 'NONE',  ( -6.512942406915326110, 3.284080845023683730E-15, 3.000000000000000000 ) ) ;
#26977 = DIRECTION ( 'NONE',  ( -1.000000000000000000, -0.000000000000000000, 0.000000000000000000 ) ) ;
#26978 = CARTESIAN_POINT ( 'NONE',  ( 3.499999999999999556, 3.771202944355708020, 4.982773259188384429 ) ) ;
#26979 = ORIENTED_EDGE ( 'NONE', *, *, #28693, .T. ) ;
#26980 = CYLINDRICAL_SURFACE ( 'NONE', #17840, 11.00000000000000000 ) ;
#26981 = DIRECTION ( 'NONE',  ( -1.000000000000000000, 0.000000000000000000, 0.000000000000000000 ) ) ;
#26982 = ORIENTED_EDGE ( 'NONE', *, *, #25415, .T. ) ;
#26983 = CARTESIAN_POINT ( 'NONE',  ( 108.2036592059121887, 19.31221474348532396, 3.367636781498203558 ) ) ;
#26984 = EDGE_CURVE ( 'NONE', #15916, #425, #2313, .T. ) ;
#26985 = EDGE_LOOP ( 'NONE', ( #22112, #6369, #21947, #19029 ) ) ;
#26986 = VERTEX_POINT ( 'NONE', #18580 ) ;
#26987 = CARTESIAN_POINT ( 'NONE',  ( 102.5829460782277209, -0.8583298743145987286, -2.713652344655540727 ) ) ;
#26988 = PERSON_AND_ORGANIZATION_ROLE ( 'classification_officer' ) ;
#26990 = ORIENTED_EDGE ( 'NONE', *, *, #14539, .F. ) ;
#26989 = CARTESIAN_POINT ( 'NONE',  ( 0.000000000000000000, -5.233522515400120589, 4.720195129223259123 ) ) ;
#26991 = ORIENTED_EDGE ( 'NONE', *, *, #24185, .F. ) ;
#26992 = CARTESIAN_POINT ( 'NONE',  ( 21.48500000136559507, 2.892927487894327410, -1.570731468192931635 ) ) ;
#26993 = ADVANCED_FACE ( 'NONE', ( #28939 ), #20729, .F. ) ;
#26994 = ORIENTED_EDGE ( 'NONE', *, *, #7935, .T. ) ;
#26995 = DIRECTION ( 'NONE',  ( 1.000000000000000000, -8.574039729943018344E-17, -0.000000000000000000 ) ) ;
#26996 = DIRECTION ( 'NONE',  ( 0.000000000000000000, 1.000000000000000000, 0.000000000000000000 ) ) ;
#26998 = ORIENTED_EDGE ( 'NONE', *, *, #229, .T. ) ;
#26997 = DIRECTION ( 'NONE',  ( -0.000000000000000000, -0.000000000000000000, 1.000000000000000000 ) ) ;
#26999 = CARTESIAN_POINT ( 'NONE',  ( 3.249999999999999556, 8.475820894092974456, 4.057423117305423155 ) ) ;
#27000 = CARTESIAN_POINT ( 'NONE',  ( 2.795120465735310589, 2.298374178341501040, -9.482538569693103270 ) ) ;
#27001 = CARTESIAN_POINT ( 'NONE',  ( 101.8797206818347973, -5.166491396334524033, 2.184956718991889257 ) ) ;
#27002 = CARTESIAN_POINT ( 'NONE',  ( 1.661358730909628482E-15, -10.85582367538893322, -1.425064293572451790 ) ) ;
#27003 = EDGE_CURVE ( 'NONE', #8635, #32283, #17787, .T. ) ;
#27004 = FACE_OUTER_BOUND ( 'NONE', #19882, .T. ) ;
#27005 = CARTESIAN_POINT ( 'NONE',  ( 35.27024661284173845, -8.402227462205928532, -0.4367666027840573229 ) ) ;
#27006 = DIRECTION ( 'NONE',  ( -0.000000000000000000, -0.9659258262890700886, 0.2588190451025139116 ) ) ;
#27007 = EDGE_CURVE ( 'NONE', #17346, #17028, #19233, .T. ) ;
#27008 = CARTESIAN_POINT ( 'NONE',  ( 18.65837979360809840, -6.995851018290569989, -0.07017451552783644797 ) ) ;
#27009 = CC_DESIGN_PERSON_AND_ORGANIZATION_ASSIGNMENT ( #10685, #26571, ( #7128 ) ) ;
#27010 = PLANE ( 'NONE',  #26287 ) ;
#27011 = CARTESIAN_POINT ( 'NONE',  ( 23.92250000273118715, -1.291182301015472600, -2.378061970571982098 ) ) ;
#27012 = CARTESIAN_POINT ( 'NONE',  ( 21.74290772321993970, -0.1310194482076047495, -2.499999999999998668 ) ) ;
#27013 = CARTESIAN_POINT ( 'NONE',  ( -5.600050802731187716, -3.113457007523259268, 0.9222479816126455399 ) ) ;
#27014 = VERTEX_POINT ( 'NONE', #29769 ) ;
#27015 = CARTESIAN_POINT ( 'NONE',  ( -5.800050800000000173, 1.887961173149511618, 2.331437884370912705 ) ) ;
#27016 = DIRECTION ( 'NONE',  ( -1.000000000000000000, 2.473959037481237219E-13, -0.000000000000000000 ) ) ;
#27017 = CARTESIAN_POINT ( 'NONE',  ( -5.750050802731187183, -0.3135853898029607456, 2.983565686104819648 ) ) ;
#27018 = CARTESIAN_POINT ( 'NONE',  ( 7.637044425071358944, -3.948987408480924888, 1.500000000000286215 ) ) ;
#27019 = VERTEX_POINT ( 'NONE', #29432 ) ;
#27020 = CARTESIAN_POINT ( 'NONE',  ( 20.07596637266122386, -16.49406355791761314, -1.500000000000000444 ) ) ;
#27021 = EDGE_CURVE ( 'NONE', #15187, #10158, #27555, .T. ) ;
#27022 = ORIENTED_EDGE ( 'NONE', *, *, #1514, .T. ) ;
#27023 = CARTESIAN_POINT ( 'NONE',  ( 2.040131092124688017, -10.88355153714070944, 1.762033267153191529 ) ) ;
#27024 = EDGE_CURVE ( 'NONE', #27475, #13277, #4845, .T. ) ;
#27025 = APPROVAL_ROLE ( '' ) ;
#27026 = CARTESIAN_POINT ( 'NONE',  ( 22.25111450864416085, -3.256483526998273983E-15, 2.499999999999998668 ) ) ;
#27027 = ORIENTED_EDGE ( 'NONE', *, *, #18920, .F. ) ;
#27028 = CARTESIAN_POINT ( 'NONE',  ( 9.172108879787137070, -0.1070445578126106301, -1.318121098349317233 ) ) ;
#27029 = DIRECTION ( 'NONE',  ( -1.000000000000000000, 8.574039729943022041E-17, -1.232595164407830946E-32 ) ) ;
#27030 = CARTESIAN_POINT ( 'NONE',  ( -2.609496843286264411, -0.08904926966055601301, 1.559466048951597905 ) ) ;
#27031 = CARTESIAN_POINT ( 'NONE',  ( 24.27681693764188964, -17.38739216501981844, -1.394420419282224710 ) ) ;
#27032 = ORIENTED_EDGE ( 'NONE', *, *, #15867, .T. ) ;
#27033 = CARTESIAN_POINT ( 'NONE',  ( 0.000000000000000000, 0.000000000000000000, 0.000000000000000000 ) ) ;
#27034 = CARTESIAN_POINT ( 'NONE',  ( 107.1772993348646281, 16.40207914262226296, 1.508259000770581615 ) ) ;
#27035 = LINE ( 'NONE', #6155, #2304 ) ;
#27037 = EDGE_LOOP ( 'NONE', ( #13583, #13270, #15545 ) ) ;
#27036 = CARTESIAN_POINT ( 'NONE',  ( 25.70386696102259805, 2.933694492117787433, -0.5143199855282081234 ) ) ;
#27038 = DIRECTION ( 'NONE',  ( 0.000000000000000000, -0.4067366430757887730, -0.9135454576426058626 ) ) ;
#27039 = FACE_OUTER_BOUND ( 'NONE', #11703, .T. ) ;
#27040 = CARTESIAN_POINT ( 'NONE',  ( -2.819379691724354764, -6.927609664243463250, -4.522129901861166701 ) ) ;
#27041 = FACE_OUTER_BOUND ( 'NONE', #2376, .T. ) ;
#27042 = LINE ( 'NONE', #16995, #19995 ) ;
#27043 = CARTESIAN_POINT ( 'NONE',  ( -31.69096085994287648, -21.93932300455405482, 1.032046942684759827 ) ) ;
#27044 = PLANE ( 'NONE',  #12377 ) ;
#27045 = CYLINDRICAL_SURFACE ( 'NONE', #15072, 8.749000000000002331 ) ;
#27046 = DIRECTION ( 'NONE',  ( 0.000000000000000000, 0.000000000000000000, 1.000000000000000000 ) ) ;
#27047 = ORIENTED_EDGE ( 'NONE', *, *, #9962, .F. ) ;
#27048 = CARTESIAN_POINT ( 'NONE',  ( -2.850050802731187716, 2.331437884370912705, -1.887961173149511618 ) ) ;
#27049 = ORIENTED_EDGE ( 'NONE', *, *, #6291, .T. ) ;
#27050 = CARTESIAN_POINT ( 'NONE',  ( 5.377543748152549874, 2.741043480755029016, -7.530955069117485579 ) ) ;
#27051 = CARTESIAN_POINT ( 'NONE',  ( 7.249760686538667009, -8.437262856154180923, 2.318425219014200511 ) ) ;
#27052 = DIRECTION ( 'NONE',  ( -1.000000000000000000, -0.000000000000000000, 0.000000000000000000 ) ) ;
#27053 = DIRECTION ( 'NONE',  ( -0.9896144216807899463, 0.000000000000000000, -0.1437473352845035635 ) ) ;
#27054 = LINE ( 'NONE', #32272, #30631 ) ;
#27055 = VERTEX_POINT ( 'NONE', #20084 ) ;
#27056 = EDGE_CURVE ( 'NONE', #6248, #12746, #25742, .T. ) ;
#27057 = CARTESIAN_POINT ( 'NONE',  ( -58.79722610518447823, -4.531914678867814850, 5.561913525286415805 ) ) ;
#27058 = EDGE_CURVE ( 'NONE', #9130, #7398, #12437, .T. ) ;
#27059 = VERTEX_POINT ( 'NONE', #8191 ) ;
#27060 = CALENDAR_DATE ( 2026, 6, 10 ) ;
#27061 = CARTESIAN_POINT ( 'NONE',  ( 10.00000000000000178, -8.574039729943018837E-16, 0.000000000000000000 ) ) ;
#27062 = CARTESIAN_POINT ( 'NONE',  ( -3.450050802731187805, 1.887961173149511618, 2.331437884370912705 ) ) ;
#27063 = CARTESIAN_POINT ( 'NONE',  ( 6.037141879243264064, 6.194548269014965136, -5.783072176360581018 ) ) ;
#27064 = VERTEX_POINT ( 'NONE', #5680 ) ;
#27065 = ORIENTED_EDGE ( 'NONE', *, *, #14959, .T. ) ;
#27066 = CARTESIAN_POINT ( 'NONE',  ( 24.54749999999999943, -2.594547506269383685, -0.7685399846772043020 ) ) ;
#27067 = CARTESIAN_POINT ( 'NONE',  ( 4.749760686538667009, 1.391664247347228045, 7.892520144992438702 ) ) ;
#27068 = CARTESIAN_POINT ( 'NONE',  ( 23.36000000000000298, -1.573300977624594976, 1.942864903642425700 ) ) ;
#27069 = CARTESIAN_POINT ( 'NONE',  ( 3.986046653337826484, -12.21565841940772223, -1.500000000000423217 ) ) ;
#27071 = ORIENTED_EDGE ( 'NONE', *, *, #3809, .T. ) ;
#27070 = CARTESIAN_POINT ( 'NONE',  ( 0.000000000000000000, -2.417132211460119251, 8.149077976821791580 ) ) ;
#27072 = CARTESIAN_POINT ( 'NONE',  ( -4.487550801365593145, -2.752080473201636845, 2.228590825266444586 ) ) ;
#27073 = DIRECTION ( 'NONE',  ( 1.000000000000000000, -0.000000000000000000, -0.000000000000000000 ) ) ;
#27074 = CARTESIAN_POINT ( 'NONE',  ( 108.1288400433390393, -19.92462668933127290, 1.384270303710046335 ) ) ;
#27075 = CARTESIAN_POINT ( 'NONE',  ( 10.00000000000000000, 2.376879293651063652, 4.116875700062091248 ) ) ;
#27076 = ORIENTED_EDGE ( 'NONE', *, *, #11544, .T. ) ;
#27078 = EDGE_LOOP ( 'NONE', ( #27944, #22424, #5868, #26710, #14607, #27307 ) ) ;
#27077 = CARTESIAN_POINT ( 'NONE',  ( 6.883866601413089370, -7.193114723270776167, -4.949663153219604261 ) ) ;
#27079 = CARTESIAN_POINT ( 'NONE',  ( 2.795120667414443982, 6.320583870825355000, 7.433119754671740687 ) ) ;
#27080 =( BOUNDED_SURFACE ( )  B_SPLINE_SURFACE ( 3, 3, ( 
 ( #28771, #23765, #18435, #25960 ),
 ( #3214, #28627, #6049, #23423 ),
 ( #31454, #10904, #21109, #26454 ),
 ( #878, #5862, #8532, #13558 ) ),
 .UNSPECIFIED., .F., .F., .F. ) 
 B_SPLINE_SURFACE_WITH_KNOTS ( ( 4, 4 ),
 ( 4, 4 ),
 ( 0.000000000000000000, 1.000000000000000000 ),
 ( 0.000000000000000000, 1.000000000000000000 ),
 .UNSPECIFIED. ) 
 GEOMETRIC_REPRESENTATION_ITEM ( )  RATIONAL_B_SPLINE_SURFACE ( (
 ( 1.000000000000000000, 0.9917560313531952332, 0.9917560313531952332, 1.000000000000000000),
 ( 0.6539698177806696489, 0.6485785111069292119, 0.6485785111069292119, 0.6539698177806696489),
 ( 0.6539698177806696489, 0.6485785111069292119, 0.6485785111069292119, 0.6539698177806696489),
 ( 1.000000000000000000, 0.9917560313531952332, 0.9917560313531952332, 1.000000000000000000) ) ) 
 REPRESENTATION_ITEM ( '' )  SURFACE ( )  );
#27081 = B_SPLINE_CURVE_WITH_KNOTS ( 'NONE', 3,
 ( #23773, #1380, #21423, #16553, #15908, #13722, #13384, #8724 ),
 .UNSPECIFIED., .F., .F.,
 ( 4, 2, 2, 4 ),
 ( 2.494123547463239299E-07, 0.001262099805913989656, 0.001893025002693609444, 0.002523950199473229232 ),
 .UNSPECIFIED. ) ;
#27082 = CARTESIAN_POINT ( 'NONE',  ( 10.57125986779756843, 0.6226916219172707878, -4.971152295393295617 ) ) ;
#27083 = CARTESIAN_POINT ( 'NONE',  ( 25.29750000136559507, -2.363507492473152283, -1.913930629741525280 ) ) ;
#27084 = CARTESIAN_POINT ( 'NONE',  ( 10.55147673363119054, 4.458382051008191738, 2.285372942704970267 ) ) ;
#27085 = DIRECTION ( 'NONE',  ( 1.000000000000000000, 0.000000000000000000, 0.000000000000000000 ) ) ;
#27086 = ADVANCED_FACE ( 'NONE', ( #11019 ), #10319, .T. ) ;
#27087 = CARTESIAN_POINT ( 'NONE',  ( 2.592584712405585634, -2.232024585011552542, 10.08167743096629287 ) ) ;
#27088 = CARTESIAN_POINT ( 'NONE',  ( 84.88357813082512848, -2.741221277476444396, 1.873788409402975530 ) ) ;
#27089 = DIRECTION ( 'NONE',  ( -0.5075624751249148137, -0.8616149568369101397, 0.000000000000000000 ) ) ;
#27090 = EDGE_LOOP ( 'NONE', ( #22132, #24994, #3111, #27596, #6714, #9359, #32133, #15042, #18283, #22402 ) ) ;
#27091 = CARTESIAN_POINT ( 'NONE',  ( 101.6960370908956008, -2.521493381538000733, 3.387663558704466116 ) ) ;
#27092 = ORIENTED_EDGE ( 'NONE', *, *, #32404, .T. ) ;
#27093 = CARTESIAN_POINT ( 'NONE',  ( 21.34740231350976458, -21.82855858833835327, 1.313840182778293064 ) ) ;
#27094 = DIRECTION ( 'NONE',  ( 0.000000000000000000, 0.000000000000000000, 1.000000000000000000 ) ) ;
#27095 = CYLINDRICAL_SURFACE ( 'NONE', #6422, 2.499999999999997780 ) ;
#27096 = ORIENTED_EDGE ( 'NONE', *, *, #8074, .T. ) ;
#27097 = CARTESIAN_POINT ( 'NONE',  ( 1.394036994807608625E-16, 1.625881193364697719, 4.467071865485476856 ) ) ;
#27098 = ORIENTED_EDGE ( 'NONE', *, *, #7504, .F. ) ;
#27099 = CARTESIAN_POINT ( 'NONE',  ( 3.020080146456703751, -8.942241244950249524, 0.5244911560275880014 ) ) ;
#27101 = EDGE_LOOP ( 'NONE', ( #23332, #7628, #13432, #17993 ) ) ;
#27100 = CARTESIAN_POINT ( 'NONE',  ( 28.69354884964465668, -5.617738173989101469, -3.996604665426794156 ) ) ;
#27102 = ADVANCED_FACE ( 'NONE', ( #10855 ), #13999, .T. ) ;
#27103 = VERTEX_POINT ( 'NONE', #6000 ) ;
#27104 = DIRECTION ( 'NONE',  ( -1.000000000000000000, 0.000000000000000000, 0.000000000000000000 ) ) ;
#27105 = CARTESIAN_POINT ( 'NONE',  ( -50.60000000000000142, -10.96966150227468972, 7.500000000000000000 ) ) ;
#27107 = VERTEX_POINT ( 'NONE', #26071 ) ;
#27106 = CARTESIAN_POINT ( 'NONE',  ( -4.497588124534941834, -5.387736868085173825, -1.500000000000000000 ) ) ;
#27108 = CARTESIAN_POINT ( 'NONE',  ( -3.529825581556913254E-16, -4.116875700062066379, -2.376879293651108060 ) ) ;
#27109 = DIRECTION ( 'NONE',  ( -1.000000000000000000, 0.000000000000000000, 0.000000000000000000 ) ) ;
#27110 = EDGE_CURVE ( 'NONE', #16163, #1782, #8171, .T. ) ;
#27111 = CARTESIAN_POINT ( 'NONE',  ( -2.880987360464337677, -0.6119841066606549473, 1.499999999999999112 ) ) ;
#27112 = CARTESIAN_POINT ( 'NONE',  ( 7.192400642327426041, -7.644771086453554076, -1.500000000000285549 ) ) ;
#27114 = ORIENTED_EDGE ( 'NONE', *, *, #32404, .F. ) ;
#27113 = CARTESIAN_POINT ( 'NONE',  ( 108.0492966005174367, -18.77922090048372183, -4.828784975709461413 ) ) ;
#27115 = CARTESIAN_POINT ( 'NONE',  ( 2.661997781067676705, -9.315861390595078007, -3.981025027156597229 ) ) ;
#27116 = B_SPLINE_CURVE_WITH_KNOTS ( 'NONE', 3,
 ( #5546, #1000, #5836, #8211, #26249, #18710, #23399, #25933, #11181, #503, #3367, #10689, #31122, #21389, #23743, #856, #31430, #31596, #8685, #18410, #17014, #16516, #29244, #26728, #4016, #24381, #22222, #1498, #24231, #21873, #21719, #19551, #26911, #9494 ),
 .UNSPECIFIED., .F., .F.,
 ( 4, 2, 2, 2, 2, 2, 2, 2, 2, 2, 2, 2, 2, 2, 2, 2, 4 ),
 ( 4.567156475735417400E-05, 0.003725671012342181808, 0.007405670459927009286, 0.01108566990751183763, 0.01292566963130425441, 0.01476566935509666771, 0.01660566907888907928, 0.01844566880268149259, 0.01936566866457770444, 0.02028566852647391283, 0.02120566838837012469, 0.02212566825026633308, 0.02304566811216254493, 0.02396566797405875332, 0.02580566769785117356, 0.02764566742164359381, 0.02948566714543601752 ),
 .UNSPECIFIED. ) ;
#27117 = EDGE_CURVE ( 'NONE', #11534, #7768, #8705, .T. ) ;
#27118 = CARTESIAN_POINT ( 'NONE',  ( 23.29750000273119070, 2.594547506269380133, 0.7685399846772031918 ) ) ;
#27119 = FACE_OUTER_BOUND ( 'NONE', #9510, .T. ) ;
#27120 = FACE_OUTER_BOUND ( 'NONE', #12425, .T. ) ;
#27121 = LINE ( 'NONE', #1914, #18813 ) ;
#27122 = ORIENTED_EDGE ( 'NONE', *, *, #7638, .F. ) ;
#27123 = FACE_OUTER_BOUND ( 'NONE', #15567, .T. ) ;
#27124 = EDGE_CURVE ( 'NONE', #508, #12143, #31662, .T. ) ;
#27125 = DIRECTION ( 'NONE',  ( 7.472768010110040824E-18, 0.08715574274764535667, 0.9961946980917466554 ) ) ;
#27126 = EDGE_CURVE ( 'NONE', #6261, #31435, #1231, .T. ) ;
#27127 = CARTESIAN_POINT ( 'NONE',  ( 3.063284526842892319, -5.538577986798981279, -6.772677083981775148 ) ) ;
#27128 = ORIENTED_EDGE ( 'NONE', *, *, #30763, .T. ) ;
#27129 = CARTESIAN_POINT ( 'NONE',  ( 9.350000000000001421, 0.000000000000000000, 1.000000000000000000 ) ) ;
#27130 = CARTESIAN_POINT ( 'NONE',  ( 3.094741023239413469, -0.1906005183311293705, -1.397910568869148440 ) ) ;
#27131 = ORIENTED_EDGE ( 'NONE', *, *, #4851, .F. ) ;
#27132 = CARTESIAN_POINT ( 'NONE',  ( 108.3798353887428192, 20.29323324528803596, 1.274429984091367318 ) ) ;
#27133 = EDGE_CURVE ( 'NONE', #25870, #32468, #25790, .T. ) ;
#27134 = ORIENTED_EDGE ( 'NONE', *, *, #5321, .F. ) ;
#27135 = ORIENTED_EDGE ( 'NONE', *, *, #7722, .T. ) ;
#27136 = DIRECTION ( 'NONE',  ( 1.000000000000000000, 0.000000000000000000, 0.000000000000000000 ) ) ;
#27137 = APPROVAL_STATUS ( 'not_yet_approved' ) ;
#27139 = ORIENTED_EDGE ( 'NONE', *, *, #24917, .F. ) ;
#27138 = DIRECTION ( 'NONE',  ( 0.000000000000000000, 0.000000000000000000, -1.000000000000000000 ) ) ;
#27140 = ORIENTED_EDGE ( 'NONE', *, *, #20954, .F. ) ;
#27141 = CARTESIAN_POINT ( 'NONE',  ( 21.92250000136559507, -1.913930629741527500, 2.363507492473149618 ) ) ;
#27142 = EDGE_CURVE ( 'NONE', #32109, #31656, #14016, .T. ) ;
#27143 = ORIENTED_EDGE ( 'NONE', *, *, #28766, .T. ) ;
#27144 = CARTESIAN_POINT ( 'NONE',  ( 0.6791197550704917152, -2.303133748654007995, 8.860977624947331321 ) ) ;
#27145 = CARTESIAN_POINT ( 'NONE',  ( 0.7632845268398871230, 2.223716399045691183, -8.461683424509292450 ) ) ;
#27147 = ORIENTED_EDGE ( 'NONE', *, *, #31376, .F. ) ;
#27146 = CARTESIAN_POINT ( 'NONE',  ( 3.424298583717156572E-16, 3.993798362933309143, 3.024842911000705570 ) ) ;
#27148 = CARTESIAN_POINT ( 'NONE',  ( 5.489321606599603776, -7.664118171219017839, 2.678948506461303225 ) ) ;
#27149 = CARTESIAN_POINT ( 'NONE',  ( -34.55410851074696410, 0.5000000000000000000, 3.046816775802633881 ) ) ;
#27150 = CARTESIAN_POINT ( 'NONE',  ( 101.8275707284721250, -4.415545041187804109, 3.393491412270330354 ) ) ;
#27151 = CARTESIAN_POINT ( 'NONE',  ( 23.11000000136559507, -3.156283516753370044, -0.9349337715887220401 ) ) ;
#27152 = FACE_OUTER_BOUND ( 'NONE', #24518, .T. ) ;
#27153 = CARTESIAN_POINT ( 'NONE',  ( -1.425727661597341989, -5.130997865967109384, -5.485967528433937979 ) ) ;
#27154 = CARTESIAN_POINT ( 'NONE',  ( 110.2274383572228942, 17.36892446252421962, 4.629213727441584325 ) ) ;
#27155 = CYLINDRICAL_SURFACE ( 'NONE', #20545, 2.099999999999997868 ) ;
#27156 = EDGE_CURVE ( 'NONE', #697, #21586, #17899, .T. ) ;
#27157 = CARTESIAN_POINT ( 'NONE',  ( -2.124956573341760357, 1.323625320507108460, 3.284597389080124774 ) ) ;
#27158 = CARTESIAN_POINT ( 'NONE',  ( 102.5829460782277351, -0.8583298743146008380, -2.713652344655543391 ) ) ;
#27159 = DIRECTION ( 'NONE',  ( -1.000000000000000000, -0.000000000000000000, 0.000000000000000000 ) ) ;
#27160 = EDGE_CURVE ( 'NONE', #18803, #21638, #13333, .T. ) ;
#27161 = CARTESIAN_POINT ( 'NONE',  ( 5.865515302491369098, 15.00000000000000000, -1.500000000000000000 ) ) ;
#27162 = EDGE_CURVE ( 'NONE', #31497, #28488, #6313, .T. ) ;
#27163 = CARTESIAN_POINT ( 'NONE',  ( -5.950050802731187360, 2.983565686104819648, 0.3135853898029609677 ) ) ;
#27164 = ORIENTED_EDGE ( 'NONE', *, *, #18765, .T. ) ;
#27165 = CARTESIAN_POINT ( 'NONE',  ( -4.550050800000000173, -0.9222479816126459840, -3.113457007523259268 ) ) ;
#27166 = DIRECTION ( 'NONE',  ( -0.2951703194034056565, 0.3797261271633441959, -0.8767454310646958238 ) ) ;
#27167 = CARTESIAN_POINT ( 'NONE',  ( -5.550050802731187893, -2.983565686104819648, -0.3135853898029605791 ) ) ;
#27168 = CARTESIAN_POINT ( 'NONE',  ( -4.250050800000000351, 2.853674364686379583, 1.549418761218565921 ) ) ;
#27169 = ORIENTED_EDGE ( 'NONE', *, *, #28166, .T. ) ;
#27170 = CARTESIAN_POINT ( 'NONE',  ( -2.100050802731187272, 1.549418761218566143, -2.853674364686379583 ) ) ;
#27171 = CARTESIAN_POINT ( 'NONE',  ( 10.51239158225343751, -12.94889321834390472, -1.500000000000000444 ) ) ;
#27172 = VERTEX_POINT ( 'NONE', #3350 ) ;
#27173 = CARTESIAN_POINT ( 'NONE',  ( 15.92138669867059342, -16.39214949420826528, 1.753532102563923445 ) ) ;
#27174 = PERSON_AND_ORGANIZATION ( #6766, #25292 ) ;
#27175 = CARTESIAN_POINT ( 'NONE',  ( -56.77769102277633095, 0.5030464795276025081, -1.050000000000000044 ) ) ;
#27176 = ORIENTED_EDGE ( 'NONE', *, *, #14113, .T. ) ;
#27177 = DIRECTION ( 'NONE',  ( -1.387778780781445676E-14, 0.000000000000000000, 1.000000000000000000 ) ) ;
#27178 = EDGE_CURVE ( 'NONE', #28120, #28083, #26561, .T. ) ;
#27179 = CC_DESIGN_PERSON_AND_ORGANIZATION_ASSIGNMENT ( #9297, #19513, ( #32113 ) ) ;
#27180 = CARTESIAN_POINT ( 'NONE',  ( 25.75999999999999801, -2.208672634433321348E-15, 0.000000000000000000 ) ) ;
#27181 = CARTESIAN_POINT ( 'NONE',  ( 28.67239840559955866, -6.439901994755928172, -4.275175838857114385 ) ) ;
#27182 = CARTESIAN_POINT ( 'NONE',  ( 7.064632879756603145, -2.210816291636270137, 8.466096581343476757 ) ) ;
#27183 = CARTESIAN_POINT ( 'NONE',  ( 107.8806307222008627, -16.35047421165092985, -1.384330804613826293 ) ) ;
#27184 = ORIENTED_EDGE ( 'NONE', *, *, #3599, .F. ) ;
#27185 = CARTESIAN_POINT ( 'NONE',  ( 8.870145747188287189, 0.000000000000000000, 1.000000000000000000 ) ) ;
#27186 = CARTESIAN_POINT ( 'NONE',  ( 23.15652614122476649, -21.92931078907647802, -1.107159753869481733 ) ) ;
#27187 = CARTESIAN_POINT ( 'NONE',  ( 1.624999999999999778, 10.82112760146736363, 1.975651141462276827 ) ) ;
#27189 = ORIENTED_EDGE ( 'NONE', *, *, #26603, .F. ) ;
#27188 = LINE ( 'NONE', #29369, #12279 ) ;
#27190 = CARTESIAN_POINT ( 'NONE',  ( -10.00000000000000000, 0.000000000000000000, 0.000000000000000000 ) ) ;
#27191 = DIRECTION ( 'NONE',  ( 1.000000000000000000, 0.000000000000000000, 0.000000000000000000 ) ) ;
#27192 = CARTESIAN_POINT ( 'NONE',  ( -31.52072750637464083, 0.5000000000000022204, 1.500000000000000000 ) ) ;
#27193 = CARTESIAN_POINT ( 'NONE',  ( 17.41559371906258136, 18.02474698348859405, 1.508259000770581615 ) ) ;
#27194 = ADVANCED_FACE ( 'NONE', ( #21219 ), #31417, .T. ) ;
#27195 = VECTOR ( 'NONE', #27737, 1000.000000000000000 ) ;
#27196 = CARTESIAN_POINT ( 'NONE',  ( -4.104821569165014520E-16, -4.787500056513378510, 1.476463073999619846 ) ) ;
#27197 = LINE ( 'NONE', #29731, #20397 ) ;
#27198 = CARTESIAN_POINT ( 'NONE',  ( 4.749760686538667009, -6.139290821770289064, 5.151476664237455871 ) ) ;
#27199 = CARTESIAN_POINT ( 'NONE',  ( 3.499999999999999556, -3.573533178329615367, 5.126388750707211450 ) ) ;
#27200 = AXIS2_PLACEMENT_3D ( 'NONE', #22299, #24454, #19480 ) ;
#27201 = ORIENTED_EDGE ( 'NONE', *, *, #8383, .F. ) ;
#27202 = DIRECTION ( 'NONE',  ( -1.000000000000000000, 0.000000000000000000, -0.000000000000000000 ) ) ;
#27203 = VERTEX_POINT ( 'NONE', #32573 ) ;
#27204 = CARTESIAN_POINT ( 'NONE',  ( -6.604531657079157903, 1.883076972206379374, 2.325406398514293205 ) ) ;
#27205 = VECTOR ( 'NONE', #28307, 1000.000000000000114 ) ;
#27206 = CARTESIAN_POINT ( 'NONE',  ( 25.54750000136559507, 1.913930629741522838, -2.363507492473150062 ) ) ;
#27207 = DIRECTION ( 'NONE',  ( 0.000000000000000000, -0.1045284632676536235, 0.9945218953682734009 ) ) ;
#27208 = CARTESIAN_POINT ( 'NONE',  ( 25.75999999999999446, 1.400653562255665729, 2.728866609423114209 ) ) ;
#27209 = DIRECTION ( 'NONE',  ( -1.000000000000000000, 8.574039729943022041E-17, 6.162975822039154730E-33 ) ) ;
#27210 = EDGE_LOOP ( 'NONE', ( #8329, #6692, #16815 ) ) ;
#27211 = CARTESIAN_POINT ( 'NONE',  ( -31.67864539881508179, -25.93932300454937945, 1.095404497688271528 ) ) ;
#27212 = B_SPLINE_CURVE_WITH_KNOTS ( 'NONE', 3,
 ( #24007, #20869, #13659, #23862, #8173, #8331, #8477, #970, #18377, #3160 ),
 .UNSPECIFIED., .F., .F.,
 ( 4, 2, 2, 2, 4 ),
 ( 0.000000000000000000, 0.0003410363541725902007, 0.0006820727083451804014, 0.001023109062517770602, 0.001364145416690360803 ),
 .UNSPECIFIED. ) ;
#27213 = EDGE_LOOP ( 'NONE', ( #12243, #6879, #25539, #17289, #25069 ) ) ;
#27214 = SHAPE_DEFINITION_REPRESENTATION ( #2877, #13 ) ;
#27215 = B_SPLINE_CURVE_WITH_KNOTS ( 'NONE', 3,
 ( #4660, #30403, #2147, #32766, #9844, #20057, #30252, #27709, #7476, #17681 ),
 .UNSPECIFIED., .F., .F.,
 ( 4, 2, 2, 2, 4 ),
 ( 2.493548413898819905E-07, 0.0005478513795029408152, 0.001095453404164491726, 0.001643055428826042637, 0.002190657453487593331 ),
 .UNSPECIFIED. ) ;
#27216 = CARTESIAN_POINT ( 'NONE',  ( 18.75900454161397590, -5.871068286376763368, 4.006107076242098053 ) ) ;
#27217 = EDGE_CURVE ( 'NONE', #14650, #9106, #22059, .T. ) ;
#27218 = AXIS2_PLACEMENT_3D ( 'NONE', #8855, #3688, #31937 ) ;
#27219 = PLANE ( 'NONE',  #16010 ) ;
#27220 = CIRCLE ( 'NONE', #12801, 0.4499999999999999001 ) ;
#27221 = FACE_OUTER_BOUND ( 'NONE', #21712, .T. ) ;
#27222 = VERTEX_POINT ( 'NONE', #19538 ) ;
#27223 = ORIENTED_EDGE ( 'NONE', *, *, #6785, .F. ) ;
#27224 = CARTESIAN_POINT ( 'NONE',  ( -3.691385125341854500E-13, 10.85582367538961179, -1.425064293572943619 ) ) ;
#27225 = DIRECTION ( 'NONE',  ( 1.000000000000000000, -0.000000000000000000, -0.000000000000000000 ) ) ;
#27226 = CARTESIAN_POINT ( 'NONE',  ( 24.42249999999999943, -2.378061970571983430, 1.291182301015471712 ) ) ;
#27227 = CARTESIAN_POINT ( 'NONE',  ( 3.866957346989826405, -11.79825661644774826, -1.500000000000000444 ) ) ;
#27229 = ORIENTED_EDGE ( 'NONE', *, *, #28979, .F. ) ;
#27228 = CARTESIAN_POINT ( 'NONE',  ( 6.880159396099833735, 3.754731129947894708, -7.882559112973126503 ) ) ;
#27230 = CARTESIAN_POINT ( 'NONE',  ( -2.687550801365593323, -2.228590825266444586, -2.752080473201636401 ) ) ;
#27231 = DIRECTION ( 'NONE',  ( -0.9896144216807901683, 0.000000000000000000, -0.1437473352845036190 ) ) ;
#27232 = DIRECTION ( 'NONE',  ( 0.000000000000000000, 0.000000000000000000, -1.000000000000000000 ) ) ;
#27233 = CARTESIAN_POINT ( 'NONE',  ( 108.0945118934858158, -19.43030987198200066, -3.536500079605387814 ) ) ;
#27234 = ORIENTED_EDGE ( 'NONE', *, *, #28848, .T. ) ;
#27235 = EDGE_CURVE ( 'NONE', #3025, #28448, #7649, .T. ) ;
#27237 = ORIENTED_EDGE ( 'NONE', *, *, #31726, .F. ) ;
#27236 = CARTESIAN_POINT ( 'NONE',  ( 2.948244102837121794, 0.000000000000000000, 1.325449886338921024 ) ) ;
#27238 = EDGE_CURVE ( 'NONE', #24661, #23691, #21705, .T. ) ;
#27239 = CARTESIAN_POINT ( 'NONE',  ( -7.000050800000000351, 0.000000000000000000, 0.000000000000000000 ) ) ;
#27240 = EDGE_CURVE ( 'NONE', #2902, #4647, #10649, .T. ) ;
#27241 = DIRECTION ( 'NONE',  ( 0.000000000000000000, 0.000000000000000000, 1.000000000000000000 ) ) ;
#27242 = AXIS2_PLACEMENT_3D ( 'NONE', #7677, #15192, #15343 ) ;
#27243 = CARTESIAN_POINT ( 'NONE',  ( 25.36000000136559507, -1.570731468192933633, -2.892927487894330962 ) ) ;
#27244 = AXIS2_PLACEMENT_3D ( 'NONE', #1234, #26623, #31824 ) ;
#27245 = CARTESIAN_POINT ( 'NONE',  ( -24.48050464856572717, 18.90773822806010429, 1.500000000000000000 ) ) ;
#27246 = CARTESIAN_POINT ( 'NONE',  ( -3.175969065750143816, -11.78108755892028015, -1.500000000000000000 ) ) ;
#27247 = CARTESIAN_POINT ( 'NONE',  ( 25.23499999999999943, 0.2613211581691317065, 2.486304738420681559 ) ) ;
#27248 = AXIS2_PLACEMENT_3D ( 'NONE', #4063, #6373, #4561 ) ;
#27249 = LINE ( 'NONE', #16891, #7088 ) ;
#27250 = CYLINDRICAL_SURFACE ( 'NONE', #24723, 4.000000000000001776 ) ;
#27251 = ORIENTED_EDGE ( 'NONE', *, *, #4679, .T. ) ;
#27252 = AXIS2_PLACEMENT_3D ( 'NONE', #19520, #32899, #30376 ) ;
#27253 = CARTESIAN_POINT ( 'NONE',  ( 101.6700243166665842, -2.146915903803417791, 2.784837706280533620 ) ) ;
#27254 = EDGE_LOOP ( 'NONE', ( #29441, #31031 ) ) ;
#27255 = AXIS2_PLACEMENT_3D ( 'NONE', #21123, #11223, #26125 ) ;
#27256 = CARTESIAN_POINT ( 'NONE',  ( 4.262285728429960179E-16, 4.971152295393301834, 0.6226916219172224931 ) ) ;
#27257 = DIRECTION ( 'NONE',  ( -7.770718973608995913E-17, -0.9063077870366526012, 0.4226182617406938902 ) ) ;
#27258 = CYLINDRICAL_SURFACE ( 'NONE', #8589, 0.5000000000000008882 ) ;
#27259 = ORIENTED_EDGE ( 'NONE', *, *, #16861, .T. ) ;
#27260 = DIRECTION ( 'NONE',  ( -1.000000000000000000, 8.574039729943022041E-17, -0.000000000000000000 ) ) ;
#27261 = ORIENTED_EDGE ( 'NONE', *, *, #22732, .F. ) ;
#27262 = PLANE ( 'NONE',  #8669 ) ;
#27264 = ORIENTED_EDGE ( 'NONE', *, *, #2119, .F. ) ;
#27263 = CARTESIAN_POINT ( 'NONE',  ( 18.86043735579395886, -4.737252997097608720, -3.995336671762878211 ) ) ;
#27265 = CIRCLE ( 'NONE', #11253, 11.18125977723849296 ) ;
#27266 = ORIENTED_EDGE ( 'NONE', *, *, #29875, .F. ) ;
#27267 = CIRCLE ( 'NONE', #21407, 0.5000000000000000000 ) ;
#27268 = FACE_OUTER_BOUND ( 'NONE', #12317, .T. ) ;
#27269 = CIRCLE ( 'NONE', #5489, 0.5000000000000004441 ) ;
#27270 = AXIS2_PLACEMENT_3D ( 'NONE', #15566, #25782, #20761 ) ;
#27271 = FACE_OUTER_BOUND ( 'NONE', #4054, .T. ) ;
#27272 = EDGE_CURVE ( 'NONE', #16013, #17299, #26892, .T. ) ;
#27274 = ORIENTED_EDGE ( 'NONE', *, *, #12981, .T. ) ;
#27273 = CARTESIAN_POINT ( 'NONE',  ( -4.547423194604015784, -6.123025915217619186, -1.500000000000000222 ) ) ;
#27275 = CARTESIAN_POINT ( 'NONE',  ( 24.08779030308693692, 18.59272488193695949, -1.500000000000000000 ) ) ;
#27276 = AXIS2_PLACEMENT_3D ( 'NONE', #3644, #8643, #16480 ) ;
#27277 = CARTESIAN_POINT ( 'NONE',  ( 9.350000000000028066, 5.584097191983464876E-14, -1.000000000000000000 ) ) ;
#27278 = DIRECTION ( 'NONE',  ( -1.000000000000000000, -0.000000000000000000, -0.000000000000000000 ) ) ;
#27279 = DIRECTION ( 'NONE',  ( 0.000000000000000000, -0.8660254037844432595, 0.4999999999999918399 ) ) ;
#27280 = ADVANCED_FACE ( 'NONE', ( #4315 ), #6479, .T. ) ;
#27282 = ORIENTED_EDGE ( 'NONE', *, *, #25687, .F. ) ;
#27281 = CARTESIAN_POINT ( 'NONE',  ( 108.0243158295136254, -18.41950401259834891, -4.472575114496686766 ) ) ;
#27283 = CARTESIAN_POINT ( 'NONE',  ( 2.382865613620175349, 0.000000000000000000, 1.000000000000000222 ) ) ;
#27284 = EDGE_CURVE ( 'NONE', #6630, #12161, #1987, .T. ) ;
#27285 = AXIS2_PLACEMENT_3D ( 'NONE', #30636, #31116, #26248 ) ;
#27286 = DIRECTION ( 'NONE',  ( 0.000000000000000000, -0.8191520442889893561, 0.5735764363510496011 ) ) ;
#27287 = CARTESIAN_POINT ( 'NONE',  ( 25.54750000136559507, 3.024605502323846729, -0.3178988483021056854 ) ) ;
#27288 = DIRECTION ( 'NONE',  ( 0.000000000000000000, 0.000000000000000000, -1.000000000000000000 ) ) ;
#27289 = CYLINDRICAL_SURFACE ( 'NONE', #27841, 6.248999999999999666 ) ;
#27290 = LINE ( 'NONE', #4410, #29477 ) ;
#27291 = ORIENTED_EDGE ( 'NONE', *, *, #30669, .T. ) ;
#27292 = LINE ( 'NONE', #24950, #30039 ) ;
#27293 = AXIS2_PLACEMENT_3D ( 'NONE', #27008, #19812, #14936 ) ;
#27294 = CARTESIAN_POINT ( 'NONE',  ( 101.6199812346112878, -1.426307971359241256, -1.526432238268092823 ) ) ;
#27295 = CARTESIAN_POINT ( 'NONE',  ( 2.592584925146038888, -6.844296717724863477, -7.731606906650728028 ) ) ;
#27296 = ORIENTED_EDGE ( 'NONE', *, *, #24923, .T. ) ;
#27297 = AXIS2_PLACEMENT_3D ( 'NONE', #15318, #10317, #6963 ) ;
#27298 = CIRCLE ( 'NONE', #1155, 5.009999999999999787 ) ;
#27299 = CARTESIAN_POINT ( 'NONE',  ( 2.976845970491565296, -5.822399416825358109, 7.079702685456860323 ) ) ;
#27300 = CARTESIAN_POINT ( 'NONE',  ( 3.529825581556955655E-16, 4.116875700062116117, -2.376879293651021019 ) ) ;
#27301 = ORIENTED_EDGE ( 'NONE', *, *, #21991, .F. ) ;
#27303 = FACE_OUTER_BOUND ( 'NONE', #46, .T. ) ;
#27302 = AXIS2_PLACEMENT_3D ( 'NONE', #4596, #12256, #2432 ) ;
#27304 = ORIENTED_EDGE ( 'NONE', *, *, #14733, .T. ) ;
#27305 = CIRCLE ( 'NONE', #17160, 6.248999999999999666 ) ;
#27306 = TOROIDAL_SURFACE ( 'NONE', #29994, 11.18125977723849296, 0.5000000000000000000 ) ;
#27307 = ORIENTED_EDGE ( 'NONE', *, *, #1372, .T. ) ;
#27308 = DIRECTION ( 'NONE',  ( 1.000000000000000000, 0.000000000000000000, 0.000000000000000000 ) ) ;
#27309 = EDGE_CURVE ( 'NONE', #18705, #3656, #14644, .T. ) ;
#27311 = ORIENTED_EDGE ( 'NONE', *, *, #13721, .F. ) ;
#27310 = CARTESIAN_POINT ( 'NONE',  ( 10.00000000000000178, -4.616489984850518979, -1.946309384392642228 ) ) ;
#27312 = EDGE_LOOP ( 'NONE', ( #27890, #28829, #30695, #12637, #27340 ) ) ;
#27313 = CARTESIAN_POINT ( 'NONE',  ( 21.04750000136559507, -3.024605502323851169, 0.3178988483021052969 ) ) ;
#27314 = ORIENTED_EDGE ( 'NONE', *, *, #15244, .F. ) ;
#27315 = CARTESIAN_POINT ( 'NONE',  ( 25.52557118915447987, -17.56218954043521663, -1.000000000000000444 ) ) ;
#27316 = EDGE_CURVE ( 'NONE', #6218, #1608, #27388, .T. ) ;
#27318 = ORIENTED_EDGE ( 'NONE', *, *, #1221, .F. ) ;
#27317 = CARTESIAN_POINT ( 'NONE',  ( 102.2517087015684893, -1.537876043683827909, -1.873789182642617401 ) ) ;
#27319 = CARTESIAN_POINT ( 'NONE',  ( -1.756376981307136376, -0.1572233378491262878, 2.999999999999999556 ) ) ;
#27320 = CIRCLE ( 'NONE', #5958, 4.000000000000002665 ) ;
#27321 = EDGE_CURVE ( 'NONE', #18225, #10070, #14931, .T. ) ;
#27322 = CARTESIAN_POINT ( 'NONE',  ( 23.57316428367674277, -9.051964865549241068, 0.07017451552781736601 ) ) ;
#27323 = ADVANCED_FACE ( 'NONE', ( #6662 ), #16852, .T. ) ;
#27324 = CARTESIAN_POINT ( 'NONE',  ( 22.73500000136559862, 1.570731468192929858, 2.892927487894329186 ) ) ;
#27325 = DIRECTION ( 'NONE',  ( 8.281886410780514724E-17, 0.9659258262890692004, -0.2588190451025176309 ) ) ;
#27326 = AXIS2_PLACEMENT_3D ( 'NONE', #22812, #30346, #30195 ) ;
#27327 = AXIS2_PLACEMENT_3D ( 'NONE', #28725, #10848, #8483 ) ;
#27328 = CARTESIAN_POINT ( 'NONE',  ( 0.004027955751591347049, -11.10248303872634601, -5.485967528433937979 ) ) ;
#27329 = ADVANCED_FACE ( 'NONE', ( #5305 ), #18388, .F. ) ;
#27330 = DIRECTION ( 'NONE',  ( 0.000000000000000000, 0.9510565162951544194, -0.3090169943749448977 ) ) ;
#27331 = DIRECTION ( 'NONE',  ( 0.4999999999999978351, 0.8660254037844398178, 0.000000000000000000 ) ) ;
#27332 = VECTOR ( 'NONE', #1528, 1000.000000000000000 ) ;
#27333 = VECTOR ( 'NONE', #31027, 1000.000000000000000 ) ;
#27334 = CIRCLE ( 'NONE', #641, 302.6457063863958865 ) ;
#27335 = CARTESIAN_POINT ( 'NONE',  ( 2.942345435796908326, 8.982973658106383041, 2.300561732649640589 ) ) ;
#27336 = CARTESIAN_POINT ( 'NONE',  ( 0.000000000000000000, -1.699438267350306120, -9.241976615262172956 ) ) ;
#27337 = CARTESIAN_POINT ( 'NONE',  ( 23.61000000273119070, -1.573300977624594976, 1.942864903642425700 ) ) ;
#27338 = CARTESIAN_POINT ( 'NONE',  ( 9.101556641444268791, 0.000000000000000000, -3.895301350492843540 ) ) ;
#27339 = CARTESIAN_POINT ( 'NONE',  ( -4.350050802731187716, 2.983565686104819648, 0.3135853898029609677 ) ) ;
#27340 = ORIENTED_EDGE ( 'NONE', *, *, #4611, .T. ) ;
#27341 = EDGE_CURVE ( 'NONE', #22797, #23619, #4982, .T. ) ;
#27342 = CARTESIAN_POINT ( 'NONE',  ( -4.400050799999999818, 2.331437884370912705, -1.887961173149511618 ) ) ;
#27343 = CARTESIAN_POINT ( 'NONE',  ( 23.17076521078841367, -21.93622641188920142, -1.056592731017446996 ) ) ;
#27344 = CARTESIAN_POINT ( 'NONE',  ( -3.850050802731187272, -1.887961173149512062, -2.331437884370912261 ) ) ;
#27346 = ORIENTED_EDGE ( 'NONE', *, *, #5441, .T. ) ;
#27345 = AXIS2_PLACEMENT_3D ( 'NONE', #5477, #10637, #28700 ) ;
#27347 = DIRECTION ( 'NONE',  ( 0.000000000000000000, -0.2079116908177664480, 0.9781476007338041345 ) ) ;
#27348 =( LENGTH_UNIT ( ) NAMED_UNIT ( * ) SI_UNIT ( .MILLI., .METRE. ) );
#27349 = AXIS2_PLACEMENT_3D ( 'NONE', #22422, #7225, #32635 ) ;
#27350 = AXIS2_PLACEMENT_3D ( 'NONE', #20845, #28701, #30898 ) ;
#27351 = SHAPE_REPRESENTATION ( 'Part2_handle2', ( #2865 ), #8690 ) ;
#27352 = AXIS2_PLACEMENT_3D ( 'NONE', #977, #28580, #13987 ) ;
#27353 = VERTEX_POINT ( 'NONE', #25493 ) ;
#27354 = CARTESIAN_POINT ( 'NONE',  ( 21.03177542174607240, -17.18603084754166233, 1.753176640694531052 ) ) ;
#27355 = PERSON_AND_ORGANIZATION ( #6766, #25292 ) ;
#27356 = AXIS2_PLACEMENT_3D ( 'NONE', #1546, #11236, #11726 ) ;
#27357 = CARTESIAN_POINT ( 'NONE',  ( 5.612718825656738630, 5.432357446996408434, 6.163864706063968413 ) ) ;
#27358 = ORIENTED_EDGE ( 'NONE', *, *, #26538, .F. ) ;
#27359 = CARTESIAN_POINT ( 'NONE',  ( -3.192893893951263884, -11.75153721369459525, 1.499999999999999556 ) ) ;
#27360 = AXIS2_PLACEMENT_3D ( 'NONE', #30939, #18215, #26077 ) ;
#27361 = CARTESIAN_POINT ( 'NONE',  ( 10.00000000000000178, 3.993798362933351775, -3.024842911000649615 ) ) ;
#27362 = CARTESIAN_POINT ( 'NONE',  ( 69.04806619055770511, -5.668245219703699433, -4.312042181587000478 ) ) ;
#27363 = DIRECTION ( 'NONE',  ( -0.000000000000000000, -0.000000000000000000, -1.000000000000000000 ) ) ;
#27364 = PLANE ( 'NONE',  #21386 ) ;
#27365 = ORIENTED_EDGE ( 'NONE', *, *, #7767, .T. ) ;
#27366 = EDGE_CURVE ( 'NONE', #7714, #29657, #12765, .T. ) ;
#27367 = FACE_OUTER_BOUND ( 'NONE', #9535, .T. ) ;
#27368 = EDGE_CURVE ( 'NONE', #28748, #1705, #26844, .T. ) ;
#27369 = CARTESIAN_POINT ( 'NONE',  ( 7.249760686538667009, 1.391664247347333294, -7.892520144992419162 ) ) ;
#27370 = CARTESIAN_POINT ( 'NONE',  ( -50.60000000000000142, -10.96966150227468972, -1.000000000000000000 ) ) ;
#27372 = VERTEX_POINT ( 'NONE', #12951 ) ;
#27371 = DIRECTION ( 'NONE',  ( 0.1437473352845032581, 0.000000000000000000, -0.9896144216807900573 ) ) ;
#27373 = VECTOR ( 'NONE', #19533, 1000.000000000000000 ) ;
#27374 = CARTESIAN_POINT ( 'NONE',  ( 108.1863125916463986, 19.21562195068647938, -4.729927366917035414 ) ) ;
#27375 = CIRCLE ( 'NONE', #5508, 5.000000000000000000 ) ;
#27376 = CARTESIAN_POINT ( 'NONE',  ( -31.63092319849841871, -21.88241439596123072, 1.340913934978400501 ) ) ;
#27377 = CARTESIAN_POINT ( 'NONE',  ( 10.00000000000000000, -1.476463073999670472, 4.787500056513361635 ) ) ;
#27378 = DIRECTION ( 'NONE',  ( 0.000000000000000000, 1.000000000000000000, 0.000000000000000000 ) ) ;
#27379 = CARTESIAN_POINT ( 'NONE',  ( 101.6506736443863161, -1.868271036809460384, -2.336400895661424393 ) ) ;
#27380 = ADVANCED_FACE ( 'NONE', ( #279 ), #23642, .T. ) ;
#27381 = CIRCLE ( 'NONE', #30073, 6.248999999999999666 ) ;
#27382 = CONICAL_SURFACE ( 'NONE', #22564, 2.099999999999997868, 1.029744258676653867 ) ;
#27383 = DIRECTION ( 'NONE',  ( -0.9960221812693187404, 0.08910563629484180570, 0.000000000000000000 ) ) ;
#27384 = CARTESIAN_POINT ( 'NONE',  ( 5.377543748152548986, -6.139290821770219786, -5.151476664237539360 ) ) ;
#27385 = DIRECTION ( 'NONE',  ( 0.000000000000000000, 0.08715574274765874874, -0.9961946980917455452 ) ) ;
#27386 = CARTESIAN_POINT ( 'NONE',  ( -30.13808104058193749, 10.31370525110837200, 1.976276180383223391 ) ) ;
#27387 = ORIENTED_EDGE ( 'NONE', *, *, #13752, .T. ) ;
#27388 = LINE ( 'NONE', #24213, #16700 ) ;
#27389 = ORIENTED_EDGE ( 'NONE', *, *, #10388, .T. ) ;
#27390 = AXIS2_PLACEMENT_3D ( 'NONE', #21966, #32193, #5662 ) ;
#27391 = EDGE_CURVE ( 'NONE', #15472, #12104, #424, .T. ) ;
#27392 = CARTESIAN_POINT ( 'NONE',  ( -5.454531657079156659, -2.846291840500172921, -1.545410377633947618 ) ) ;
#27393 = APPROVAL ( #777, 'UNKNOWN' ) ;
#27394 = CARTESIAN_POINT ( 'NONE',  ( -28.83037791825872276, 5.159822176738817490, 1.500000000000000000 ) ) ;
#27395 = CARTESIAN_POINT ( 'NONE',  ( 107.5574910143032099, -18.92149487875213865, -4.691804453562030908 ) ) ;
#27396 = DIRECTION ( 'NONE',  ( 0.000000000000000000, 0.000000000000000000, 1.000000000000000000 ) ) ;
#27397 = FACE_OUTER_BOUND ( 'NONE', #29197, .T. ) ;
#27398 = ORIENTED_EDGE ( 'NONE', *, *, #30932, .F. ) ;
#27399 = CARTESIAN_POINT ( 'NONE',  ( -3.830085165118302378E-16, -4.467071865485461757, -1.625881193364742572 ) ) ;
#27400 = AXIS2_PLACEMENT_3D ( 'NONE', #7299, #15161, #25008 ) ;
#27401 = ORIENTED_EDGE ( 'NONE', *, *, #12334, .T. ) ;
#27403 = AXIS2_PLACEMENT_3D ( 'NONE', #1992, #14681, #9484 ) ;
#27402 = DATE_AND_TIME ( #27060, #29570 ) ;
#27404 = B_SPLINE_CURVE_WITH_KNOTS ( 'NONE', 3,
 ( #3625, #26380, #11784, #21667, #21817, #5953, #3780, #952, #3963, #24170 ),
 .UNSPECIFIED., .F., .F.,
 ( 4, 2, 2, 2, 4 ),
 ( 0.000000000000000000, 0.0002027550720618977013, 0.0004055101441237954026, 0.0006082652161856931311, 0.0008110202882475908053 ),
 .UNSPECIFIED. ) ;
#27405 = CARTESIAN_POINT ( 'NONE',  ( 69.07005235690151324, -6.108409966930705259, 4.006107570159479714 ) ) ;
#27406 = AXIS2_PLACEMENT_3D ( 'NONE', #14286, #24481, #29537 ) ;
#27407 = AXIS2_PLACEMENT_3D ( 'NONE', #15031, #25063, #6852 ) ;
#27408 = FACE_BOUND ( 'NONE', #16880, .T. ) ;
#27410 = CARTESIAN_POINT ( 'NONE',  ( 7.249760686538667009, -0.7071067811864522046, -8.721381771256211834 ) ) ;
#27409 = DIRECTION ( 'NONE',  ( 0.000000000000000000, 0.000000000000000000, 1.000000000000000000 ) ) ;
#27411 = VERTEX_POINT ( 'NONE', #26002 ) ;
#27412 = ADVANCED_FACE ( 'NONE', ( #18305 ), #2851, .T. ) ;
#27413 = LOCAL_TIME ( 16, 7, 10.00000000000000000, #17907 ) ;
#27414 = CARTESIAN_POINT ( 'NONE',  ( 24.60999999999999943, -1.942864903642428587, -1.573300977624592756 ) ) ;
#27415 = CARTESIAN_POINT ( 'NONE',  ( 2.970200390936400758, 9.143933199846960846, -0.5647484630024097729 ) ) ;
#27416 = CARTESIAN_POINT ( 'NONE',  ( 21.42249999999999943, -2.378061970571983430, 1.291182301015471712 ) ) ;
#27417 = CARTESIAN_POINT ( 'NONE',  ( 6.718506812351674462, -13.33599551843229669, -1.499999999999999112 ) ) ;
#27419 = ORIENTED_EDGE ( 'NONE', *, *, #427, .F. ) ;
#27418 = CARTESIAN_POINT ( 'NONE',  ( 0.8407900506755994208, -11.56055812333295307, 4.522129901861157819 ) ) ;
#27420 = CARTESIAN_POINT ( 'NONE',  ( -3.237550801365593589, 3.675193018007247403, -1.088641768524161391 ) ) ;
#27421 = FACE_OUTER_BOUND ( 'NONE', #19521, .T. ) ;
#27422 = DIRECTION ( 'NONE',  ( 1.000000000000000000, -8.574039729943018344E-17, -0.000000000000000000 ) ) ;
#27423 = CARTESIAN_POINT ( 'NONE',  ( -8.000050800000000351, 3.673940397442060361E-16, 3.000000000000000444 ) ) ;
#27424 = ORIENTED_EDGE ( 'NONE', *, *, #27663, .T. ) ;
#27426 = ORIENTED_EDGE ( 'NONE', *, *, #1848, .F. ) ;
#27425 = CARTESIAN_POINT ( 'NONE',  ( 13.58264871869483059, 21.92667377881535629, 1.161774810368582767 ) ) ;
#27427 = B_SPLINE_CURVE_WITH_KNOTS ( 'NONE', 3,
 ( #17087, #16933, #29818, #14598 ),
 .UNSPECIFIED., .F., .F.,
 ( 4, 4 ),
 ( 1.640695603511827301E-18, 0.0002986946104689498695 ),
 .UNSPECIFIED. ) ;
#27428 = VECTOR ( 'NONE', #26831, 1000.000000000000000 ) ;
#27429 = CARTESIAN_POINT ( 'NONE',  ( 107.1769020805352142, 16.40214705320008903, 1.508259000770581615 ) ) ;
#27430 = CYLINDRICAL_SURFACE ( 'NONE', #19487, 8.749000000000002331 ) ;
#27431 = CIRCLE ( 'NONE', #19973, 10.43371088333262087 ) ;
#27432 = VECTOR ( 'NONE', #20811, 1000.000000000000114 ) ;
#27433 = CARTESIAN_POINT ( 'NONE',  ( -19.16594587638616076, 17.36640870223476085, 1.500000000000000000 ) ) ;
#27434 = ADVANCED_FACE ( 'NONE', ( #918 ), #7093, .F. ) ;
#27435 = DIRECTION ( 'NONE',  ( 1.000000000000000000, 0.000000000000000000, 0.000000000000000000 ) ) ;
#27436 = CARTESIAN_POINT ( 'NONE',  ( 8.273330302600941266, -18.97014676976608882, -1.749556830060739143 ) ) ;
#27437 = CARTESIAN_POINT ( 'NONE',  ( 6.530491712438077023, 7.168846788212690058, 4.859093986587880387 ) ) ;
#27438 = CIRCLE ( 'NONE', #21050, 5.000000000000000888 ) ;
#27439 = SECURITY_CLASSIFICATION ( '', '', #7327 ) ;
#27440 = CARTESIAN_POINT ( 'NONE',  ( 23.86142584456326432, -3.703306447638166077, 1.529339877387915214 ) ) ;
#27441 = CARTESIAN_POINT ( 'NONE',  ( 0.3076690219785659930, 7.713510465966315621, 6.806638167507657045 ) ) ;
#27442 = ORIENTED_EDGE ( 'NONE', *, *, #30932, .T. ) ;
#27443 = FACE_OUTER_BOUND ( 'NONE', #9156, .T. ) ;
#27444 = VERTEX_POINT ( 'NONE', #8280 ) ;
#27445 = DIRECTION ( 'NONE',  ( -0.1767573132311699990, -0.9842544651762054064, 0.000000000000000000 ) ) ;
#27446 = CARTESIAN_POINT ( 'NONE',  ( 56.97280603064898941, -277.2763395528616002, 1.500000000000000000 ) ) ;
#27447 = VERTEX_POINT ( 'NONE', #18473 ) ;
#27448 = EDGE_CURVE ( 'NONE', #20419, #15831, #3110, .T. ) ;
#27449 = AXIS2_PLACEMENT_3D ( 'NONE', #16921, #9548, #19762 ) ;
#27450 = DIRECTION ( 'NONE',  ( -1.000000000000000000, 0.000000000000000000, 0.000000000000000000 ) ) ;
#27451 = ORIENTED_EDGE ( 'NONE', *, *, #27341, .F. ) ;
#27452 = DIRECTION ( 'NONE',  ( 0.7822388118548813107, -0.4516257885949860884, -0.4291113938172939068 ) ) ;
#27453 = EDGE_CURVE ( 'NONE', #29127, #2157, #19467, .T. ) ;
#27455 = ORIENTED_EDGE ( 'NONE', *, *, #9846, .F. ) ;
#27454 = CARTESIAN_POINT ( 'NONE',  ( 69.01345486998194190, -4.974821740502390455, -4.001041175463363686 ) ) ;
#27456 = ORIENTED_EDGE ( 'NONE', *, *, #23, .F. ) ;
#27457 = DIRECTION ( 'NONE',  ( 0.000000000000000000, -0.5877852522924797984, 0.8090169943749426773 ) ) ;
#27458 = CARTESIAN_POINT ( 'NONE',  ( 102.9705908278152293, -6.440317834495088434, -1.915219082070897638 ) ) ;
#27460 = ORIENTED_EDGE ( 'NONE', *, *, #28151, .T. ) ;
#27459 = CARTESIAN_POINT ( 'NONE',  ( -33.81874022276151237, 20.00000000000000000, 1.977928362984239019 ) ) ;
#27461 = CARTESIAN_POINT ( 'NONE',  ( 22.89387586481974424, 17.41384229090520464, -1.500000000000117906 ) ) ;
#27462 = CARTESIAN_POINT ( 'NONE',  ( 8.886302293890576465, 0.01997115109545568104, -1.161565467022932729 ) ) ;
#27463 = CARTESIAN_POINT ( 'NONE',  ( -4.099820753267308326, -5.441111812974985362, 1.745641719294580563 ) ) ;
#27464 = SECURITY_CLASSIFICATION ( '', '', #31029 ) ;
#27465 = CARTESIAN_POINT ( 'NONE',  ( 8.396671913539110577, -0.7629006742128506824, -1.500000000000000000 ) ) ;
#27467 = ORIENTED_EDGE ( 'NONE', *, *, #31643, .F. ) ;
#27466 = CARTESIAN_POINT ( 'NONE',  ( 108.0280308400905795, -18.47299924072742527, -4.369739108549834050 ) ) ;
#27468 = FACE_OUTER_BOUND ( 'NONE', #57, .T. ) ;
#27469 = CARTESIAN_POINT ( 'NONE',  ( 8.870145747188287189, 0.000000000000000000, 1.000000000000000000 ) ) ;
#27470 = DIRECTION ( 'NONE',  ( 1.000000000000000000, 0.000000000000000000, 0.000000000000000000 ) ) ;
#27471 = CARTESIAN_POINT ( 'NONE',  ( 34.48223484310472031, 0.5000000000000000000, -2.552009564962230304 ) ) ;
#27472 = CARTESIAN_POINT ( 'NONE',  ( 0.000000000000000000, -4.057423117305452465, 8.475820894092962021 ) ) ;
#27473 = DIRECTION ( 'NONE',  ( -1.000000000000000000, 0.000000000000000000, 0.000000000000000000 ) ) ;
#27474 = CIRCLE ( 'NONE', #31754, 5.100000000000000533 ) ;
#27475 = VERTEX_POINT ( 'NONE', #20661 ) ;
#27476 = CARTESIAN_POINT ( 'NONE',  ( 25.75999999999999801, -2.208672634433321348E-15, 0.000000000000000000 ) ) ;
#27477 = CARTESIAN_POINT ( 'NONE',  ( 0.000000000000000000, 0.000000000000000000, 7.500000000000000000 ) ) ;
#27478 = CARTESIAN_POINT ( 'NONE',  ( -7.637550801365593500, -3.675193018007245627, 1.088641768524163389 ) ) ;
#27479 = ORIENTED_EDGE ( 'NONE', *, *, #21805, .F. ) ;
#27480 = B_SPLINE_CURVE_WITH_KNOTS ( 'NONE', 3,
 ( #7866, #5197, #3039, #15542, #23397, #10 ),
 .UNSPECIFIED., .F., .F.,
 ( 4, 2, 4 ),
 ( 0.009531916414662763848, 0.5047659582073313889, 1.000000000000000000 ),
 .UNSPECIFIED. ) ;
#27481 = CARTESIAN_POINT ( 'NONE',  ( 0.000000000000000000, 0.000000000000000000, 0.000000000000000000 ) ) ;
#27482 = CARTESIAN_POINT ( 'NONE',  ( 25.75999999999999801, -2.208672634433321348E-15, 0.000000000000000000 ) ) ;
#27483 = VERTEX_POINT ( 'NONE', #26154 ) ;
#27484 = CARTESIAN_POINT ( 'NONE',  ( 2.303688968543995408, -1.057430054352009208, -1.500000000000000666 ) ) ;
#27485 = ADVANCED_FACE ( 'NONE', ( #8579 ), #13599, .F. ) ;
#27486 = ORIENTED_EDGE ( 'NONE', *, *, #11240, .T. ) ;
#27487 = ADVANCED_FACE ( 'NONE', ( #15796 ), #30866, .F. ) ;
#27488 = ORIENTED_EDGE ( 'NONE', *, *, #31040, .T. ) ;
#27489 = DIRECTION ( 'NONE',  ( 0.000000000000000000, -0.8191520442889951292, 0.5735764363510412744 ) ) ;
#27491 = ORIENTED_EDGE ( 'NONE', *, *, #22972, .F. ) ;
#27490 = CARTESIAN_POINT ( 'NONE',  ( 3.249999999999999556, 6.772677083992387992, 5.538577986808924436 ) ) ;
#27492 = ORIENTED_EDGE ( 'NONE', *, *, #2532, .F. ) ;
#27493 = CARTESIAN_POINT ( 'NONE',  ( 7.249760686538667009, -8.721381771256204729, 0.7071067811865423547 ) ) ;
#27494 = ORIENTED_EDGE ( 'NONE', *, *, #32263, .F. ) ;
#27495 = CARTESIAN_POINT ( 'NONE',  ( 15.11750262208148499, 0.000000000000000000, -5.364851207409463640 ) ) ;
#27496 = CONICAL_SURFACE ( 'NONE', #32313, 10.97000000000001485, 0.1745329251994333364 ) ;
#27498 = VERTEX_POINT ( 'NONE', #2963 ) ;
#27497 = LINE ( 'NONE', #21968, #25098 ) ;
#27499 = CARTESIAN_POINT ( 'NONE',  ( -16.85000000000000142, -10.96966150227469505, -11.00000000000000000 ) ) ;
#27500 = CARTESIAN_POINT ( 'NONE',  ( 102.9885081044300534, -6.698322160490901567, 0.07017451552781736601 ) ) ;
#27501 = CARTESIAN_POINT ( 'NONE',  ( 23.79750000136559507, 0.3178988483021036315, 3.024605502323848949 ) ) ;
#27502 = CARTESIAN_POINT ( 'NONE',  ( 3.499999999999999556, 0.6700234925292691823, 8.473551116235677583 ) ) ;
#27503 = CARTESIAN_POINT ( 'NONE',  ( 5.489321289187128805, 8.118169347437836691, 0.1038943573681802152 ) ) ;
#27504 = DIRECTION ( 'NONE',  ( -1.000000000000000000, 0.000000000000000000, -0.000000000000000000 ) ) ;
#27505 = DIRECTION ( 'NONE',  ( 1.000000000000000000, 0.000000000000000000, -0.000000000000000000 ) ) ;
#27506 = EDGE_CURVE ( 'NONE', #10544, #31825, #5909, .T. ) ;
#27507 = DIRECTION ( 'NONE',  ( 0.000000000000000000, -0.9271838545667855369, -0.3746065934159163446 ) ) ;
#27508 = PLANE ( 'NONE',  #5337 ) ;
#27509 = CYLINDRICAL_SURFACE ( 'NONE', #9706, 3.000000000000000000 ) ;
#27510 = CARTESIAN_POINT ( 'NONE',  ( 84.37491783462850492, -2.359815117480457136, 0.07017451550799885807 ) ) ;
#27511 = B_SPLINE_CURVE_WITH_KNOTS ( 'NONE', 3,
 ( #2029, #29937, #27441, #12201, #9876, #30283, #22401, #32619 ),
 .UNSPECIFIED., .F., .F.,
 ( 4, 2, 2, 4 ),
 ( 5.099451029799539141E-07, 0.001229190215600031548, 0.001843530350848556279, 0.002457870486097081010 ),
 .UNSPECIFIED. ) ;
#27512 = CARTESIAN_POINT ( 'NONE',  ( -8.000050800000000351, 0.000000000000000000, 0.000000000000000000 ) ) ;
#27513 = CARTESIAN_POINT ( 'NONE',  ( -2.650050802731187094, 1.887961173149511618, 2.331437884370912705 ) ) ;
#27514 = ORIENTED_EDGE ( 'NONE', *, *, #25752, .F. ) ;
#27515 = CARTESIAN_POINT ( 'NONE',  ( -8.087550801365594566, 2.752080473201636845, -2.228590825266444142 ) ) ;
#27516 = EDGE_CURVE ( 'NONE', #18705, #17188, #21149, .T. ) ;
#27517 = CARTESIAN_POINT ( 'NONE',  ( 107.2807778896295616, 16.98061326146200045, -2.731285459285014205 ) ) ;
#27518 = CARTESIAN_POINT ( 'NONE',  ( -4.300050800000000173, 2.983565686104819648, 0.3135853898029609677 ) ) ;
#27519 = EDGE_LOOP ( 'NONE', ( #29500, #10211, #9202, #3192 ) ) ;
#27520 = FACE_OUTER_BOUND ( 'NONE', #26579, .T. ) ;
#27521 = CARTESIAN_POINT ( 'NONE',  ( 6.037141879243262288, -5.783072176360604111, -6.194548269014942932 ) ) ;
#27522 = EDGE_LOOP ( 'NONE', ( #23197, #18064, #2618, #22711 ) ) ;
#27523 = CARTESIAN_POINT ( 'NONE',  ( 14.67795211623746354, -16.02380094600420790, 1.499999999999579892 ) ) ;
#27524 = PERSON_AND_ORGANIZATION ( #6766, #25292 ) ;
#27526 = EDGE_CURVE ( 'NONE', #61, #32887, #13119, .T. ) ;
#27525 = CARTESIAN_POINT ( 'NONE',  ( -2.906376978575949455, 0.1572233378491263989, -2.999999999999999556 ) ) ;
#27527 = EDGE_LOOP ( 'NONE', ( #22430, #28612, #6501, #20717 ) ) ;
#27528 = DIRECTION ( 'NONE',  ( -7.023442172597881513E-17, -0.8191520442889946851, 0.5735764363510420516 ) ) ;
#27529 = ORIENTED_EDGE ( 'NONE', *, *, #29562, .F. ) ;
#27530 = CARTESIAN_POINT ( 'NONE',  ( 1.750000000000000000, 8.265874651078044977, -1.981241088980699061 ) ) ;
#27531 = CARTESIAN_POINT ( 'NONE',  ( 28.66539030321571602, -6.714659430093917081, -4.074610069486789499 ) ) ;
#27532 = CARTESIAN_POINT ( 'NONE',  ( 3.249999999999999556, 0.000000000000000000, 0.000000000000000000 ) ) ;
#27533 = DIRECTION ( 'NONE',  ( 4.917867153433058194E-17, 0.5735764363510524877, -0.8191520442889873577 ) ) ;
#27534 = ORIENTED_EDGE ( 'NONE', *, *, #27856, .F. ) ;
#27535 = EDGE_CURVE ( 'NONE', #4750, #8629, #4278, .T. ) ;
#27536 = CARTESIAN_POINT ( 'NONE',  ( -31.80940264096946635, 0.000000000000000000, 4.148259000770580407 ) ) ;
#27537 = LINE ( 'NONE', #2474, #13493 ) ;
#27539 = ORIENTED_EDGE ( 'NONE', *, *, #23778, .T. ) ;
#27538 = CYLINDRICAL_SURFACE ( 'NONE', #16017, 2.999999999999999112 ) ;
#27540 = DIRECTION ( 'NONE',  ( 0.000000000000000000, 0.000000000000000000, 1.000000000000000000 ) ) ;
#27541 = CARTESIAN_POINT ( 'NONE',  ( 12.44989959798868817, 0.000000000000000000, 13.00000000000004441 ) ) ;
#27542 = LINE ( 'NONE', #3996, #23002 ) ;
#27543 = ADVANCED_FACE ( 'NONE', ( #3588 ), #22136, .F. ) ;
#27544 = CARTESIAN_POINT ( 'NONE',  ( 0.3076688720859502846, 0.9727984658936051909, -10.24120291390721427 ) ) ;
#27545 = DIRECTION ( 'NONE',  ( 0.000000000000000000, 1.000000000000000000, 0.000000000000000000 ) ) ;
#27546 = DIRECTION ( 'NONE',  ( 8.574039729943018344E-17, 1.000000000000000000, 0.000000000000000000 ) ) ;
#27547 = DIRECTION ( 'NONE',  ( 0.000000000000000000, 0.000000000000000000, 1.000000000000000000 ) ) ;
#27548 = CARTESIAN_POINT ( 'NONE',  ( -56.72401055955798199, 0.2376380563149646796, -1.445333642338585634 ) ) ;
#27550 = FACE_OUTER_BOUND ( 'NONE', #24235, .T. ) ;
#27549 = UNCERTAINTY_MEASURE_WITH_UNIT (LENGTH_MEASURE( 1.000000000000000082E-05 ), #10458, 'distance_accuracy_value', 'NONE');
#27551 = VERTEX_POINT ( 'NONE', #32173 ) ;
#27552 = EDGE_CURVE ( 'NONE', #8122, #23895, #6043, .T. ) ;
#27553 = VERTEX_POINT ( 'NONE', #24606 ) ;
#27554 = CARTESIAN_POINT ( 'NONE',  ( -6.354531657079158791, -3.105402419394638791, 0.9198621039125867149 ) ) ;
#27555 =( BOUNDED_CURVE ( )  B_SPLINE_CURVE ( 2, ( #17034, #6526, #22395, #24402, #32611, #1521, #9190, #27243, #27083, #4185, #22089, #14353, #4360, #14538, #1873, #1684, #22245, #11880, #32304, #19573, #2023, #6848, #19729, #29929, #12195, #17542, #23067, #30278, #2524, #5528, #25568, #15529, #13184, #23242, #188, #23386, #15363, #15027, #30431, #10180, #25247, #13041, #30784, #28089, #2678, #12846, #8009, #7510, #32951, #27922, #10368, #5035, #28415, #347, #7855, #20232, #2368, #10520, #30933, #20733, #15716, #18050, #20403, #15213, #7735, #25416, #12691, #22896, #17712, #28238, #12542, #30618, #7701, #17896, #25921, #27739, #5187, #3029, #9870 ),
 .UNSPECIFIED., .F., .F. ) 
 B_SPLINE_CURVE_WITH_KNOTS ( ( 3, 2, 2, 2, 2, 2, 2, 2, 2, 2, 2, 2, 2, 2, 2, 2, 2, 2, 2, 2, 2, 2, 2, 2, 2, 2, 2, 2, 2, 2, 2, 2, 2, 2, 2, 2, 2, 2, 2, 3 ),
 ( 0.03266179187250656257, 0.05000000000000000278, 0.07499999999999999722, 0.1000000000000000056, 0.1250000000000000000, 0.1499999999999999944, 0.1749999999999999889, 0.2000000000000000111, 0.2250000000000000056, 0.2500000000000000000, 0.2750000000000000222, 0.2999999999999999889, 0.3250000000000000111, 0.3499999999999999778, 0.3749999999999999445, 0.4000000000000000222, 0.4249999999999999889, 0.4500000000000000111, 0.4749999999999999778, 0.5000000000000000000, 0.5250000000000000222, 0.5500000000000000444, 0.5749999999999999556, 0.5999999999999998668, 0.6250000000000000000, 0.6499999999999999112, 0.6750000000000000444, 0.6999999999999999556, 0.7249999999999998668, 0.7500000000000000000, 0.7749999999999999112, 0.8000000000000000444, 0.8249999999999999556, 0.8499999999999998668, 0.8750000000000000000, 0.8999999999999999112, 0.9250000000000000444, 0.9499999999999999556, 0.9749999999999998668, 1.000000000000000000 ),
 .UNSPECIFIED. ) 
 CURVE ( )  GEOMETRIC_REPRESENTATION_ITEM ( )  RATIONAL_B_SPLINE_CURVE ( ( 0.9676416783621977213, 0.9472082996767436924, 1.000000000000000000, 0.9238795325112867385, 1.000000000000000000, 0.9238795325112867385, 1.000000000000000000, 0.9238795325112867385, 1.000000000000000000, 0.9238795325112867385, 1.000000000000000000, 0.9238795325112867385, 1.000000000000000000, 0.9238795325112867385, 1.000000000000000000, 0.9238795325112867385, 1.000000000000000000, 0.9238795325112867385, 1.000000000000000000, 0.9238795325112867385, 1.000000000000000000, 0.9238795325112867385, 1.000000000000000000, 0.9238795325112867385, 1.000000000000000000, 0.9238795325112867385, 1.000000000000000000, 0.9238795325112867385, 1.000000000000000000, 0.9238795325112867385, 1.000000000000000000, 0.9238795325112867385, 1.000000000000000000, 0.9238795325112867385, 1.000000000000000000, 0.9238795325112867385, 1.000000000000000000, 0.9238795325112867385, 1.000000000000000000, 0.9238795325112867385, 1.000000000000000000, 0.9238795325112867385, 1.000000000000000000, 0.9238795325112867385, 1.000000000000000000, 0.9238795325112867385, 1.000000000000000000, 0.9238795325112867385, 1.000000000000000000, 0.9238795325112867385, 1.000000000000000000, 0.9238795325112867385, 1.000000000000000000, 0.9238795325112867385, 1.000000000000000000, 0.9238795325112867385, 1.000000000000000000, 0.9238795325112867385, 1.000000000000000000, 0.9238795325112867385, 1.000000000000000000, 0.9238795325112867385, 1.000000000000000000, 0.9238795325112867385, 1.000000000000000000, 0.9238795325112867385, 1.000000000000000000, 0.9238795325112867385, 1.000000000000000000, 0.9238795325112867385, 1.000000000000000000, 0.9238795325112867385, 1.000000000000000000, 0.9238795325112867385, 1.000000000000000000, 0.9238795325112867385, 1.000000000000000000, 0.9238795325112867385, 1.000000000000000000 ) ) 
 REPRESENTATION_ITEM ( '' )  );
#27556 = DIRECTION ( 'NONE',  ( 0.5150380749100547106, 0.000000000000000000, -0.8571673007021120005 ) ) ;
#27557 = CARTESIAN_POINT ( 'NONE',  ( 41.43929652434211164, -5.500819839281755996, -5.695980980372493008 ) ) ;
#27558 = ADVANCED_FACE ( 'NONE', ( #11436, #16779 ), #24122, .T. ) ;
#27559 = CARTESIAN_POINT ( 'NONE',  ( 4.550593937914527487, -12.71036632817956225, 1.757020553911816885 ) ) ;
#27560 = ORIENTED_EDGE ( 'NONE', *, *, #1897, .F. ) ;
#27561 = CARTESIAN_POINT ( 'NONE',  ( 3.249999999999999556, 6.807171995660674213, -6.478011392632816445 ) ) ;
#27562 = EDGE_CURVE ( 'NONE', #3016, #3811, #21632, .T. ) ;
#27563 = ORIENTED_EDGE ( 'NONE', *, *, #4347, .T. ) ;
#27564 = DIRECTION ( 'NONE',  ( 0.000000000000000000, -0.9961946980917449901, -0.08715574274766567375 ) ) ;
#27565 = CALENDAR_DATE ( 2026, 6, 10 ) ;
#27566 = CARTESIAN_POINT ( 'NONE',  ( 102.4230146827279668, -3.995787599048658656, 3.999773674144124769 ) ) ;
#27567 = CARTESIAN_POINT ( 'NONE',  ( 5.612974384376776982, 4.279837954023570923, -7.013635602076161213 ) ) ;
#27569 = CYLINDRICAL_SURFACE ( 'NONE', #24646, 3.000000000000000444 ) ;
#27568 = CARTESIAN_POINT ( 'NONE',  ( 6.524595623740806261, 6.215987993068528894, -6.028129343649548666 ) ) ;
#27570 = ORIENTED_EDGE ( 'NONE', *, *, #23541, .T. ) ;
#27571 = CARTESIAN_POINT ( 'NONE',  ( -7.362942409646514363, 1.214281993118000652E-15, 3.000000000000000000 ) ) ;
#27572 = CARTESIAN_POINT ( 'NONE',  ( 2.592584512312228195, 10.27797909968510126, -0.9926283730736131794 ) ) ;
#27573 = CARTESIAN_POINT ( 'NONE',  ( 24.11000000136559862, -2.892927487894331406, 1.570731468192932301 ) ) ;
#27574 = EDGE_CURVE ( 'NONE', #25915, #12626, #31837, .T. ) ;
#27575 = CARTESIAN_POINT ( 'NONE',  ( 6.604716885356828548, -13.59583205938461248, -1.500000000000562661 ) ) ;
#27577 = ORIENTED_EDGE ( 'NONE', *, *, #8777, .T. ) ;
#27576 = CARTESIAN_POINT ( 'NONE',  ( 0.1517578099453105456, -1.375880305419411309, 4.522129901861157819 ) ) ;
#27578 = CARTESIAN_POINT ( 'NONE',  ( -2.937550801365593323, -1.828967928396026510, 3.368539882008728004 ) ) ;
#27579 = DIRECTION ( 'NONE',  ( 0.000000000000000000, 1.000000000000000000, 0.000000000000000000 ) ) ;
#27580 = DIRECTION ( 'NONE',  ( -0.000000000000000000, -0.000000000000000000, -1.000000000000000000 ) ) ;
#27581 = CARTESIAN_POINT ( 'NONE',  ( 102.4237878418678633, -3.999739124949584834, -3.993434327387568317 ) ) ;
#27582 = ORIENTED_EDGE ( 'NONE', *, *, #29612, .F. ) ;
#27584 = VERTEX_POINT ( 'NONE', #1064 ) ;
#27583 = CARTESIAN_POINT ( 'NONE',  ( 24.16865442153403620, -17.43004354390618005, 1.504494863253181602 ) ) ;
#27585 = CARTESIAN_POINT ( 'NONE',  ( 3.020080256209073610, 5.680439424473828325, 6.926136578651334474 ) ) ;
#27586 = CARTESIAN_POINT ( 'NONE',  ( -10.00000000000000000, 0.000000000000000000, 0.000000000000000000 ) ) ;
#27587 = CARTESIAN_POINT ( 'NONE',  ( -31.59999999999999787, -25.43932300454937945, 1.500000000000000000 ) ) ;
#27588 = ADVANCED_FACE ( 'NONE', ( #29153 ), #21465, .T. ) ;
#27589 = CARTESIAN_POINT ( 'NONE',  ( -16.91808550243790066, 10.26716432527312683, 1.977393880026240724 ) ) ;
#27590 = CARTESIAN_POINT ( 'NONE',  ( -23.54713438637982748, 3.520075575296777171, 1.500000000000000000 ) ) ;
#27591 = CARTESIAN_POINT ( 'NONE',  ( -3.353510967526656117, -11.46056164226659924, -1.500000000000000000 ) ) ;
#27592 = CARTESIAN_POINT ( 'NONE',  ( 10.25005080000000035, 0.000000000000000000, 3.499999999999999556 ) ) ;
#27593 = EDGE_CURVE ( 'NONE', #23377, #6237, #194, .T. ) ;
#27594 = CARTESIAN_POINT ( 'NONE',  ( 23.85260150831978265, -3.857138523333644375, 1.873789191099454410 ) ) ;
#27595 = DIRECTION ( 'NONE',  ( 0.000000000000000000, 0.000000000000000000, -1.000000000000000000 ) ) ;
#27596 = ORIENTED_EDGE ( 'NONE', *, *, #16403, .T. ) ;
#27597 = CARTESIAN_POINT ( 'NONE',  ( 8.454317476977939450, 15.00000000000000178, 4.148259000770580407 ) ) ;
#27598 = ORIENTED_EDGE ( 'NONE', *, *, #2472, .F. ) ;
#27599 = ADVANCED_FACE ( 'NONE', ( #4226 ), #24298, .F. ) ;
#27600 = CARTESIAN_POINT ( 'NONE',  ( 10.56183597391177464, -4.753758587302148619, 0.000000000000000000 ) ) ;
#27601 = DIRECTION ( 'NONE',  ( -0.01881412180678018048, -0.9998229987455978796, 6.686078034528572161E-19 ) ) ;
#27602 = CARTESIAN_POINT ( 'NONE',  ( 3.249999999999999556, 0.000000000000000000, 0.000000000000000000 ) ) ;
#27603 = ORIENTED_EDGE ( 'NONE', *, *, #4835, .F. ) ;
#27604 = CARTESIAN_POINT ( 'NONE',  ( 108.0257329329460134, 18.32145104924472889, -5.109022856120751577 ) ) ;
#27605 = ORIENTED_EDGE ( 'NONE', *, *, #9210, .F. ) ;
#27606 = DIRECTION ( 'NONE',  ( -1.000000000000000000, 1.321650053510178573E-16, -0.000000000000000000 ) ) ;
#27608 = ORIENTED_EDGE ( 'NONE', *, *, #30438, .T. ) ;
#27607 = CARTESIAN_POINT ( 'NONE',  ( 54.94622396149055277, -5.386472726642053566, -4.033870040937042489 ) ) ;
#27609 = ORIENTED_EDGE ( 'NONE', *, *, #24542, .F. ) ;
#27610 = DIRECTION ( 'NONE',  ( -0.000000000000000000, -0.000000000000000000, 1.000000000000000000 ) ) ;
#27611 = EDGE_CURVE ( 'NONE', #429, #28913, #4417, .T. ) ;
#27612 = CARTESIAN_POINT ( 'NONE',  ( 102.9361373302715918, -5.944196040818416016, -2.713652344655542059 ) ) ;
#27613 = CC_DESIGN_DATE_AND_TIME_ASSIGNMENT ( #19161, #29354, ( #26379 ) ) ;
#27615 = VERTEX_POINT ( 'NONE', #8906 ) ;
#27614 = CARTESIAN_POINT ( 'NONE',  ( 0.000000000000000000, 5.227991826304090317, 9.620177616658001085 ) ) ;
#27616 = CARTESIAN_POINT ( 'NONE',  ( 107.5617870620230860, -18.98359792954988379, 4.522129899028605848 ) ) ;
#27617 = CARTESIAN_POINT ( 'NONE',  ( 8.950995676490915542, 0.000000000000000000, -1.008084992930270651 ) ) ;
#27618 = CARTESIAN_POINT ( 'NONE',  ( 0.000000000000000000, 0.000000000000000000, 0.000000000000000000 ) ) ;
#27619 = DIRECTION ( 'NONE',  ( -1.000000000000000000, -0.000000000000000000, -0.000000000000000000 ) ) ;
#27621 = ORIENTED_EDGE ( 'NONE', *, *, #4387, .T. ) ;
#27620 = CARTESIAN_POINT ( 'NONE',  ( 107.6641581766472768, -20.45810077038816743, -1.499999999999999556 ) ) ;
#27622 = DIRECTION ( 'NONE',  ( -1.000000000000000000, -0.000000000000000000, -0.000000000000000000 ) ) ;
#27623 = B_SPLINE_CURVE_WITH_KNOTS ( 'NONE', 3,
 ( #7096, #7261, #11955, #24815 ),
 .UNSPECIFIED., .F., .F.,
 ( 4, 4 ),
 ( -6.746902117092110274E-06, 2.872315617932023530E-05 ),
 .UNSPECIFIED. ) ;
#27624 = DIRECTION ( 'NONE',  ( 2.219124775574837589E-17, 0.2588190451025108585, 0.9659258262890709767 ) ) ;
#27625 = CARTESIAN_POINT ( 'NONE',  ( 25.11000000136559507, -3.156283516753370044, -0.9349337715887220401 ) ) ;
#27626 = ADVANCED_FACE ( 'NONE', ( #21946 ), #9244, .T. ) ;
#27627 = CARTESIAN_POINT ( 'NONE',  ( 10.00000000000000178, -0.6226916219171699796, -4.971152295393309828 ) ) ;
#27628 = CARTESIAN_POINT ( 'NONE',  ( 0.7632845268398873451, -5.538577986808840059, -6.772677083992440394 ) ) ;
#27629 = CARTESIAN_POINT ( 'NONE',  ( 20.49917871223744470, -21.72428526870506005, -1.411325660096713230 ) ) ;
#27630 = VERTEX_POINT ( 'NONE', #19282 ) ;
#27631 = FACE_OUTER_BOUND ( 'NONE', #21371, .T. ) ;
#27632 = B_SPLINE_CURVE_WITH_KNOTS ( 'NONE', 3,
 ( #21927, #11912, #4207, #9040, #27106, #27273, #14736, #6723, #16913, #24933, #11566, #19258, #14377, #14229, #21613, #29463, #16759, #24426, #19753, #21764, #9388, #1544, #19599, #17258, #32148, #9220, #29959, #2045, #8889, #24588, #32479, #19449 ),
 .UNSPECIFIED., .F., .F.,
 ( 4, 2, 2, 2, 2, 2, 2, 2, 2, 2, 2, 2, 2, 2, 2, 4 ),
 ( 0.000000000000000000, 0.004348185525199021496, 0.005435231906498774919, 0.006522278287798528341, 0.008696371050398036054, 0.009783417431697791211, 0.01087046381299754637, 0.01195751019429730153, 0.01304455657559705668, 0.01521864933819656700, 0.01630569571949631869, 0.01739274210079607211, 0.02174092762599509621, 0.02608911315119412030, 0.03043729867639314440, 0.03478548420159216503 ),
 .UNSPECIFIED. ) ;
#27633 = DIRECTION ( 'NONE',  ( 0.000000000000000000, -0.5735764363510502672, 0.8191520442889888010 ) ) ;
#27634 = CARTESIAN_POINT ( 'NONE',  ( -6.537550801365592967, 1.828967928396027398, -3.368539882008727115 ) ) ;
#27635 = ORIENTED_EDGE ( 'NONE', *, *, #23525, .F. ) ;
#27636 = CARTESIAN_POINT ( 'NONE',  ( 5.887530180601100227, 7.449245365665851715, -3.870837198608021001 ) ) ;
#27637 = FACE_OUTER_BOUND ( 'NONE', #24607, .T. ) ;
#27638 = ORIENTED_EDGE ( 'NONE', *, *, #28956, .T. ) ;
#27639 = CARTESIAN_POINT ( 'NONE',  ( 107.7876430001691404, 19.84562591319662417, 3.582469705350817435 ) ) ;
#27640 = ORIENTED_EDGE ( 'NONE', *, *, #20957, .T. ) ;
#27641 = VERTEX_POINT ( 'NONE', #19469 ) ;
#27642 = CARTESIAN_POINT ( 'NONE',  ( -3.038890739117073636, -0.3712649131886727183, 1.487764840819179257 ) ) ;
#27644 = EDGE_LOOP ( 'NONE', ( #6178, #6671, #31926, #29407 ) ) ;
#27643 = CARTESIAN_POINT ( 'NONE',  ( -3.167352811678424196, 3.267420276671043357E-12, 1.051912341319082511 ) ) ;
#27645 = ORIENTED_EDGE ( 'NONE', *, *, #20577, .F. ) ;
#27646 = CARTESIAN_POINT ( 'NONE',  ( 22.86000000136559862, -0.9349337715887247047, 3.156283516753367824 ) ) ;
#27647 = ORIENTED_EDGE ( 'NONE', *, *, #1425, .T. ) ;
#27648 = CARTESIAN_POINT ( 'NONE',  ( 4.104821569165004659E-16, 4.787500056513366076, 1.476463073999653819 ) ) ;
#27650 = ORIENTED_EDGE ( 'NONE', *, *, #21919, .F. ) ;
#27649 = CARTESIAN_POINT ( 'NONE',  ( 1.828104818894226380, -1.262475772535087915, 1.500000000000000000 ) ) ;
#27651 = CARTESIAN_POINT ( 'NONE',  ( 7.249760686538667009, 0.8180878109962995692, -8.711672189281419065 ) ) ;
#27652 = DIRECTION ( 'NONE',  ( 1.000000000000000000, -0.000000000000000000, -0.000000000000000000 ) ) ;
#27653 = CARTESIAN_POINT ( 'NONE',  ( 10.55147673363118876, -2.376879293651094294, 4.116875700062075261 ) ) ;
#27654 = DIRECTION ( 'NONE',  ( -1.000000000000000000, 0.000000000000000000, 0.000000000000000000 ) ) ;
#27655 = CARTESIAN_POINT ( 'NONE',  ( 107.4168514414812279, -16.88233545631868182, -3.542414872600711195 ) ) ;
#27656 = CARTESIAN_POINT ( 'NONE',  ( 25.48003164478615190, -17.55790041459374962, 1.000000000000000888 ) ) ;
#27657 = EDGE_CURVE ( 'NONE', #16174, #10288, #26237, .T. ) ;
#27658 = ADVANCED_FACE ( 'NONE', ( #16425 ), #26870, .T. ) ;
#27659 = LINE ( 'NONE', #1774, #32103 ) ;
#27660 = DIRECTION ( 'NONE',  ( 0.000000000000000000, -1.000000000000000000, 0.000000000000000000 ) ) ;
#27661 = DIRECTION ( 'NONE',  ( 0.000000000000000000, 0.000000000000000000, 1.000000000000000000 ) ) ;
#27662 = CARTESIAN_POINT ( 'NONE',  ( 23.50111451137534857, -3.256483526998273983E-15, 2.499999999999998668 ) ) ;
#27663 = EDGE_CURVE ( 'NONE', #2795, #3368, #29816, .T. ) ;
#27664 = CARTESIAN_POINT ( 'NONE',  ( 102.8074457324386515, -4.091069046465106496, 5.695980980372492120 ) ) ;
#27665 = CARTESIAN_POINT ( 'NONE',  ( -1.850050802731187716, 1.887961173149511618, 2.331437884370912705 ) ) ;
#27666 = ORIENTED_EDGE ( 'NONE', *, *, #24477, .T. ) ;
#27667 = CARTESIAN_POINT ( 'NONE',  ( -7.937550801365594211, 3.368539882008727115, 1.828967928396026954 ) ) ;
#27668 = CARTESIAN_POINT ( 'NONE',  ( -34.48223484310472742, 0.5000000000000000000, -2.482234843104710986 ) ) ;
#27669 = CARTESIAN_POINT ( 'NONE',  ( -3.762942409646513386, 4.884725290497410777E-15, -2.999999999999999556 ) ) ;
#27670 = ORIENTED_EDGE ( 'NONE', *, *, #24471, .T. ) ;
#27671 = CARTESIAN_POINT ( 'NONE',  ( 10.55147673363118876, -4.116875700062067267, -2.376879293651108060 ) ) ;
#27672 =( NAMED_UNIT ( * ) PLANE_ANGLE_UNIT ( ) SI_UNIT ( $, .RADIAN. ) );
#27673 = CARTESIAN_POINT ( 'NONE',  ( 107.4763378844003086, -17.74173259612938480, 5.018187998315496223 ) ) ;
#27674 = ORIENTED_EDGE ( 'NONE', *, *, #21268, .F. ) ;
#27675 = CARTESIAN_POINT ( 'NONE',  ( 19.76534894311605228, -16.89703626480067555, 1.499999999996504796 ) ) ;
#27676 = CALENDAR_DATE ( 2026, 6, 10 ) ;
#27677 = CARTESIAN_POINT ( 'NONE',  ( -0.1366093623685602776, -14.96249823008941604, -1.499999999999999556 ) ) ;
#27678 = EDGE_LOOP ( 'NONE', ( #18103, #23141, #9928, #21169 ) ) ;
#27679 = DIRECTION ( 'NONE',  ( -1.000000000000000000, 0.000000000000000000, 0.000000000000000000 ) ) ;
#27680 = ORIENTED_EDGE ( 'NONE', *, *, #4662, .F. ) ;
#27681 = CARTESIAN_POINT ( 'NONE',  ( -59.84585868070823267, -5.753144558333703529, 1.500000000000000000 ) ) ;
#27682 = CARTESIAN_POINT ( 'NONE',  ( 9.192617927958346868, 0.08611596088357059697, -1.322472180771091077 ) ) ;
#27683 = LINE ( 'NONE', #14654, #29428 ) ;
#27684 = DIRECTION ( 'NONE',  ( -2.219124775574993204E-17, -0.2588190451025284555, 0.9659258262890663138 ) ) ;
#27685 = EDGE_LOOP ( 'NONE', ( #27114, #5169, #24384, #27640 ) ) ;
#27686 = DIRECTION ( 'NONE',  ( 1.000000000000000000, 0.000000000000000000, 3.469446951953611033E-15 ) ) ;
#27687 = CARTESIAN_POINT ( 'NONE',  ( 0.000000000000000000, 0.000000000000000000, 0.000000000000000000 ) ) ;
#27688 = EDGE_CURVE ( 'NONE', #11907, #16750, #25593, .T. ) ;
#27689 = EDGE_LOOP ( 'NONE', ( #5418, #21524 ) ) ;
#27690 = LINE ( 'NONE', #2308, #21908 ) ;
#27691 = CARTESIAN_POINT ( 'NONE',  ( 0.000000000000000000, -9.884132761439094139, 4.709950686174575907 ) ) ;
#27692 = CARTESIAN_POINT ( 'NONE',  ( 79.17573959169237696, 22.98125563777605151, -4.612695725900423760 ) ) ;
#27693 = DIRECTION ( 'NONE',  ( 1.000000000000000000, -0.000000000000000000, 0.000000000000000000 ) ) ;
#27694 = CARTESIAN_POINT ( 'NONE',  ( -8.000050800000055418, 1.847639235587218209, 2.786559910703183984 ) ) ;
#27695 = DIRECTION ( 'NONE',  ( 0.000000000000000000, -0.8191520442889844711, -0.5735764363510564845 ) ) ;
#27696 = CARTESIAN_POINT ( 'NONE',  ( -56.77817977891114509, 0.4289077168656530992, -1.500224696652619372 ) ) ;
#27697 = CARTESIAN_POINT ( 'NONE',  ( 23.00622743561894623, -21.91302709721439967, 1.171678142437898584 ) ) ;
#27698 = ORIENTED_EDGE ( 'NONE', *, *, #1597, .T. ) ;
#27699 = CARTESIAN_POINT ( 'NONE',  ( -5.212550801365593678, -1.828967928396026510, 3.368539882008728004 ) ) ;
#27700 = ORIENTED_EDGE ( 'NONE', *, *, #18777, .T. ) ;
#27701 = CARTESIAN_POINT ( 'NONE',  ( -8.154531657079159501, 0.9198621039125853827, 3.105402419394639235 ) ) ;
#27702 = CARTESIAN_POINT ( 'NONE',  ( 108.9281931508044181, 17.68923109249016790, 5.234450355725419612 ) ) ;
#27703 = CARTESIAN_POINT ( 'NONE',  ( 107.6641948605100083, -20.45809826282308208, 1.500000000000000000 ) ) ;
#27704 = CARTESIAN_POINT ( 'NONE',  ( 21.03177542174608661, -17.18603084754167298, 1.753176640694532162 ) ) ;
#27705 = LINE ( 'NONE', #25208, #23654 ) ;
#27706 = ORIENTED_EDGE ( 'NONE', *, *, #11753, .F. ) ;
#27707 = CARTESIAN_POINT ( 'NONE',  ( 21.41577794885431274, -21.75491960302827366, 1.449133755489594000 ) ) ;
#27708 = ORIENTED_EDGE ( 'NONE', *, *, #31411, .F. ) ;
#27709 = CARTESIAN_POINT ( 'NONE',  ( 6.880159329304570193, -5.066480354148979792, 7.110803091624043226 ) ) ;
#27710 = CALENDAR_DATE ( 2026, 6, 10 ) ;
#27711 = CARTESIAN_POINT ( 'NONE',  ( 18.75856847572524444, -5.875942627837241972, 3.998506281399210049 ) ) ;
#27712 = EDGE_CURVE ( 'NONE', #30308, #22652, #32235, .T. ) ;
#27713 = CARTESIAN_POINT ( 'NONE',  ( 18.99198631684116378, -3.266799627756511004, -1.526432259289659532 ) ) ;
#27715 = LINE ( 'NONE', #15194, #19320 ) ;
#27714 = DIRECTION ( 'NONE',  ( 0.000000000000000000, 0.000000000000000000, -1.000000000000000000 ) ) ;
#27716 = EDGE_CURVE ( 'NONE', #16327, #9445, #11837, .T. ) ;
#27717 = ORIENTED_EDGE ( 'NONE', *, *, #12396, .F. ) ;
#27718 = CARTESIAN_POINT ( 'NONE',  ( -8.000050800000000351, -2.963268750767338755, -0.5301859913251431022 ) ) ;
#27719 = DIRECTION ( 'NONE',  ( 0.000000000000000000, -0.7431448254773863615, -0.6691306063588671194 ) ) ;
#27720 = CARTESIAN_POINT ( 'NONE',  ( 23.73500000136559152, 3.156283516753366047, 0.9349337715887203748 ) ) ;
#27721 = CARTESIAN_POINT ( 'NONE',  ( 10.00000000000000000, 0.8254815157535239090, 4.681538312723519724 ) ) ;
#27723 = ORIENTED_EDGE ( 'NONE', *, *, #6697, .T. ) ;
#27722 = CARTESIAN_POINT ( 'NONE',  ( 5.978127801841131017, -13.24614298058319051, 0.9788672205888330202 ) ) ;
#27724 = CARTESIAN_POINT ( 'NONE',  ( -3.587550801365593678, -3.521866450007987037, -0.3701630799359323931 ) ) ;
#27725 = CARTESIAN_POINT ( 'NONE',  ( -41.54914239086199501, -15.55749394147906806, 5.221013518636386408 ) ) ;
#27726 = AXIS2_PLACEMENT_3D ( 'NONE', #23876, #6165, #26890 ) ;
#27727 = CARTESIAN_POINT ( 'NONE',  ( 5.887530252753765403, -6.663910820542616520, 5.105578361685893185 ) ) ;
#27729 = ADVANCED_FACE ( 'NONE', ( #32076, #30087 ), #32421, .T. ) ;
#27728 = FACE_OUTER_BOUND ( 'NONE', #3267, .T. ) ;
#27730 = ORIENTED_EDGE ( 'NONE', *, *, #10095, .T. ) ;
#27732 = VERTEX_POINT ( 'NONE', #29739 ) ;
#27731 = CARTESIAN_POINT ( 'NONE',  ( 23.72064572293002982, -17.26593119145053734, 1.418862781619489644 ) ) ;
#27733 = EDGE_CURVE ( 'NONE', #10967, #26019, #22212, .T. ) ;
#27734 = CIRCLE ( 'NONE', #10648, 8.750000000000000000 ) ;
#27735 =( BOUNDED_CURVE ( )  B_SPLINE_CURVE ( 2, ( #6783, #4468, #14795, #27170, #4620, #7431, #21999, #17630, #12284, #24662, #30036 ),
 .UNSPECIFIED., .F., .F. ) 
 B_SPLINE_CURVE_WITH_KNOTS ( ( 3, 2, 2, 2, 2, 3 ),
 ( 0.8728822619934377691, 0.8750000000000000000, 0.8906250000000000000, 0.9062500000000000000, 0.9218750000000000000, 0.9353822619934377691 ),
 .UNSPECIFIED. ) 
 CURVE ( )  GEOMETRIC_REPRESENTATION_ITEM ( )  RATIONAL_B_SPLINE_CURVE ( ( 0.9821626249036861100, 0.9896829947469995004, 1.000000000000000000, 0.9238795325112867385, 1.000000000000000000, 0.9238795325112867385, 1.000000000000000000, 0.9238795325112867385, 1.000000000000000000, 0.9341965377642872381, 0.9821626249036861100 ) ) 
 REPRESENTATION_ITEM ( '' )  );
#27736 = CARTESIAN_POINT ( 'NONE',  ( 12.72110778810032805, 6.644964735738586370, 1.500000000000000222 ) ) ;
#27737 = DIRECTION ( 'NONE',  ( -1.000000000000000000, -1.369475477426763776E-16, 0.000000000000000000 ) ) ;
#27738 = EDGE_CURVE ( 'NONE', #14263, #32276, #6817, .T. ) ;
#27739 = CARTESIAN_POINT ( 'NONE',  ( 21.11000000136559507, -2.892927487894331406, 1.570731468192932523 ) ) ;
#27740 = CARTESIAN_POINT ( 'NONE',  ( -27.51259159022300693, 5.525525355233276592, 1.500000000001506795 ) ) ;
#27741 = CARTESIAN_POINT ( 'NONE',  ( -3.423542882029046996, -10.69121096831242390, -1.500000000000000444 ) ) ;
#27742 = FACE_OUTER_BOUND ( 'NONE', #15734, .T. ) ;
#27743 = CARTESIAN_POINT ( 'NONE',  ( 8.870145747188287189, 0.000000000000000000, 1.000000000000000000 ) ) ;
#27744 = CARTESIAN_POINT ( 'NONE',  ( 7.249760686538667009, -1.391664247347174754, -7.892520144992448472 ) ) ;
#27745 = ORIENTED_EDGE ( 'NONE', *, *, #4119, .F. ) ;
#27746 = CARTESIAN_POINT ( 'NONE',  ( 40.72654494865490449, -4.620392906571557212, 2.184955499781490840 ) ) ;
#27747 = ADVANCED_FACE ( 'NONE', ( #12018 ), #9483, .T. ) ;
#27748 = AXIS2_PLACEMENT_3D ( 'NONE', #9292, #4275, #27347 ) ;
#27749 = AXIS2_PLACEMENT_3D ( 'NONE', #8782, #10966, #1087 ) ;
#27750 = APPROVAL_ROLE ( '' ) ;
#27751 = ORIENTED_EDGE ( 'NONE', *, *, #22437, .T. ) ;
#27752 = VECTOR ( 'NONE', #21806, 999.9999999999998863 ) ;
#27753 = CARTESIAN_POINT ( 'NONE',  ( -10.00000000000000000, 0.000000000000000000, 0.000000000000000000 ) ) ;
#27754 = ORIENTED_EDGE ( 'NONE', *, *, #19914, .T. ) ;
#27755 = CARTESIAN_POINT ( 'NONE',  ( -23.31977477728428028, 3.998227953278257640, 2.146185852361371715 ) ) ;
#27757 = EDGE_LOOP ( 'NONE', ( #23930, #4558, #13052, #7198 ) ) ;
#27756 = CARTESIAN_POINT ( 'NONE',  ( 28.69317175488845351, -5.632308185119928368, -4.018750267688441902 ) ) ;
#27758 = ORIENTED_EDGE ( 'NONE', *, *, #6126, .F. ) ;
#27759 = CARTESIAN_POINT ( 'NONE',  ( -3.370691070153704949, -1.614088942876946264, -1.500000000000000000 ) ) ;
#27760 = DIRECTION ( 'NONE',  ( -0.1327696077594705815, 0.9911469271785068313, 0.000000000000000000 ) ) ;
#27761 = CARTESIAN_POINT ( 'NONE',  ( 3.499999999999999556, 1.418488851014406693, 6.085876303339381899 ) ) ;
#27762 = DIRECTION ( 'NONE',  ( 0.000000000000000000, 0.000000000000000000, -1.000000000000000000 ) ) ;
#27764 = ORIENTED_EDGE ( 'NONE', *, *, #31997, .F. ) ;
#27763 = CARTESIAN_POINT ( 'NONE',  ( 0.6728001243864736303, 4.913284922774382224, 7.719803900020800747 ) ) ;
#27765 = DIRECTION ( 'NONE',  ( -1.000000000000000000, 6.938893903907221278E-15, -0.000000000000000000 ) ) ;
#27766 = CARTESIAN_POINT ( 'NONE',  ( 13.13178786250159469, -17.31629153505179275, 4.522129901861156931 ) ) ;
#27767 = FACE_OUTER_BOUND ( 'NONE', #1296, .T. ) ;
#27768 = ADVANCED_FACE ( 'NONE', ( #16689 ), #32450, .T. ) ;
#27769 = CARTESIAN_POINT ( 'NONE',  ( 9.437548970008961646, 0.1642588933130686712, -1.000000000000000000 ) ) ;
#27771 = ORIENTED_EDGE ( 'NONE', *, *, #10428, .F. ) ;
#27770 = DIRECTION ( 'NONE',  ( 0.000000000000000000, 0.000000000000000000, -1.000000000000000000 ) ) ;
#27772 = ADVANCED_FACE ( 'NONE', ( #21862 ), #19382, .T. ) ;
#27773 = LINE ( 'NONE', #22125, #16198 ) ;
#27774 = AXIS2_PLACEMENT_3D ( 'NONE', #16488, #8823, #6648 ) ;
#27775 = CIRCLE ( 'NONE', #25122, 0.5000000000000008882 ) ;
#27776 = CARTESIAN_POINT ( 'NONE',  ( 6.038145077921538650, -2.472816103755196782, -8.106170535363476759 ) ) ;
#27777 = CARTESIAN_POINT ( 'NONE',  ( 24.67250000136559507, 2.363507492473148286, 1.913930629741525058 ) ) ;
#27778 = EDGE_CURVE ( 'NONE', #32682, #22025, #14323, .T. ) ;
#27779 = CARTESIAN_POINT ( 'NONE',  ( 107.4505076186455312, 17.92734628881788694, -4.758038775231021589 ) ) ;
#27780 = DIRECTION ( 'NONE',  ( 1.000000000000000000, -0.000000000000000000, -0.000000000000000000 ) ) ;
#27781 = DIRECTION ( 'NONE',  ( -0.8251117619019981975, 0.5649695393302014423, 0.000000000000000000 ) ) ;
#27782 = AXIS2_PLACEMENT_3D ( 'NONE', #8452, #18497, #31373 ) ;
#27783 = ORIENTED_EDGE ( 'NONE', *, *, #12048, .T. ) ;
#27784 = CARTESIAN_POINT ( 'NONE',  ( 6.357667975083868939, -4.790963222208053374, 7.150591204917380317 ) ) ;
#27785 = CARTESIAN_POINT ( 'NONE',  ( -50.60000000000000142, -10.96966150227468972, 6.999999999999999112 ) ) ;
#27786 = CARTESIAN_POINT ( 'NONE',  ( -7.437550801365595099, -1.088641768524163611, -3.675193018007245627 ) ) ;
#27787 = ORIENTED_EDGE ( 'NONE', *, *, #2633, .T. ) ;
#27788 = ADVANCED_FACE ( 'NONE', ( #20199 ), #14986, .F. ) ;
#27789 = CC_DESIGN_DATE_AND_TIME_ASSIGNMENT ( #15948, #13438, ( #8765 ) ) ;
#27790 = DIRECTION ( 'NONE',  ( 1.000000000000000000, -0.000000000000000000, -0.000000000000000000 ) ) ;
#27791 = AXIS2_PLACEMENT_3D ( 'NONE', #29417, #27073, #26924 ) ;
#27792 = LINE ( 'NONE', #2233, #24220 ) ;
#27793 = VECTOR ( 'NONE', #28568, 1000.000000000000114 ) ;
#27794 = DIRECTION ( 'NONE',  ( 0.09975574163943223827, -0.1727820128662104771, 0.9798954883250904357 ) ) ;
#27795 = ORIENTED_EDGE ( 'NONE', *, *, #25835, .T. ) ;
#27796 = CARTESIAN_POINT ( 'NONE',  ( 23.05362332218847143, -16.83301128369467037, 1.000000000000000000 ) ) ;
#27797 = ORIENTED_EDGE ( 'NONE', *, *, #19997, .T. ) ;
#27798 = VECTOR ( 'NONE', #24346, 1000.000000000000000 ) ;
#27799 = DIRECTION ( 'NONE',  ( 0.000000000000000000, 0.000000000000000000, -1.000000000000000000 ) ) ;
#27800 = VECTOR ( 'NONE', #17744, 1000.000000000000000 ) ;
#27801 = VERTEX_POINT ( 'NONE', #13003 ) ;
#27802 = CARTESIAN_POINT ( 'NONE',  ( 7.249760686538667009, 2.741043480755029016, -7.530955069117485579 ) ) ;
#27804 = ORIENTED_EDGE ( 'NONE', *, *, #31043, .T. ) ;
#27803 = CARTESIAN_POINT ( 'NONE',  ( -8.049676575031998738, 8.479088208360996928E-16, 6.923700951379997193 ) ) ;
#27805 = ORIENTED_EDGE ( 'NONE', *, *, #30829, .F. ) ;
#27806 = CARTESIAN_POINT ( 'NONE',  ( 3.249999999999999556, -8.475820894092944258, -4.057423117305486215 ) ) ;
#27807 = EDGE_CURVE ( 'NONE', #16263, #8590, #15681, .T. ) ;
#27808 = ORIENTED_EDGE ( 'NONE', *, *, #1838, .T. ) ;
#27809 = FACE_OUTER_BOUND ( 'NONE', #4052, .T. ) ;
#27811 = ORIENTED_EDGE ( 'NONE', *, *, #568, .F. ) ;
#27810 = DIRECTION ( 'NONE',  ( -0.000000000000000000, -0.000000000000000000, -1.000000000000000000 ) ) ;
#27812 = CARTESIAN_POINT ( 'NONE',  ( 1.404908439943009846, -10.20361334857307511, -1.764679167141864458 ) ) ;
#27813 = EDGE_CURVE ( 'NONE', #1202, #24580, #29787, .T. ) ;
#27814 = FACE_OUTER_BOUND ( 'NONE', #32829, .T. ) ;
#27815 = LINE ( 'NONE', #25328, #32237 ) ;
#27816 = AXIS2_PLACEMENT_3D ( 'NONE', #31718, #21326, #10980 ) ;
#27817 = CARTESIAN_POINT ( 'NONE',  ( 4.749760686538667009, 2.741043480754926875, 7.530955069117522882 ) ) ;
#27818 = CARTESIAN_POINT ( 'NONE',  ( 107.9462823452559945, -17.29584125157618146, -3.322807143007931785 ) ) ;
#27819 = CARTESIAN_POINT ( 'NONE',  ( 25.24493059864584765, -17.53551310887478465, 1.328338028043089203 ) ) ;
#27820 = VECTOR ( 'NONE', #6414, 1000.000000000000000 ) ;
#27821 = AXIS2_PLACEMENT_3D ( 'NONE', #25054, #29766, #2172 ) ;
#27822 = AXIS2_PLACEMENT_3D ( 'NONE', #29568, #16671, #1822 ) ;
#27823 = DIRECTION ( 'NONE',  ( 0.000000000000000000, 0.000000000000000000, -1.000000000000000000 ) ) ;
#27824 = CARTESIAN_POINT ( 'NONE',  ( 29.11693253002209403, -8.303828435806185126, 0.02339150517593243869 ) ) ;
#27825 = CARTESIAN_POINT ( 'NONE',  ( 5.885541615502094537, 8.322568858718552676, 1.090540896198838761 ) ) ;
#27826 = CARTESIAN_POINT ( 'NONE',  ( 101.6022419886208468, -1.170867242066748304, 0.07017451550800647697 ) ) ;
#27827 = CARTESIAN_POINT ( 'NONE',  ( 22.75111450864416085, -1.241879311143409511E-16, -2.499999999999998668 ) ) ;
#27828 = CARTESIAN_POINT ( 'NONE',  ( -1.800050802731187227, 0.9222479816126443186, 3.113457007523260156 ) ) ;
#27829 = ORIENTED_EDGE ( 'NONE', *, *, #15714, .F. ) ;
#27830 = CARTESIAN_POINT ( 'NONE',  ( -5.337550801365593678, -1.828967928396026510, 3.368539882008728004 ) ) ;
#27831 = ADVANCED_FACE ( 'NONE', ( #33065 ), #5309, .F. ) ;
#27832 = AXIS2_PLACEMENT_3D ( 'NONE', #8921, #11275, #28830 ) ;
#27833 = FACE_OUTER_BOUND ( 'NONE', #2540, .T. ) ;
#27834 = CARTESIAN_POINT ( 'NONE',  ( -4.150050802731187538, -0.3135853898029607456, 2.983565686104819648 ) ) ;
#27835 = ORIENTED_EDGE ( 'NONE', *, *, #4219, .T. ) ;
#27836 = DIRECTION ( 'NONE',  ( -1.000000000000000000, 0.000000000000000000, 0.000000000000000000 ) ) ;
#27837 = B_SPLINE_CURVE_WITH_KNOTS ( 'NONE', 3,
 ( #4529, #14529, #14343, #24738, #32603, #17386, #7004, #4029 ),
 .UNSPECIFIED., .F., .F.,
 ( 4, 2, 2, 4 ),
 ( 2.024520226902067482E-07, 0.001261135997420258399, 0.001891602770119042579, 0.002522069542817826325 ),
 .UNSPECIFIED. ) ;
#27838 = ORIENTED_EDGE ( 'NONE', *, *, #16337, .F. ) ;
#27839 = CARTESIAN_POINT ( 'NONE',  ( 10.87895964298158624, -15.23742357220648636, 1.754278677543597231 ) ) ;
#27840 = APPROVAL_ROLE ( '' ) ;
#27841 = AXIS2_PLACEMENT_3D ( 'NONE', #22282, #19768, #29974 ) ;
#27843 = ORIENTED_EDGE ( 'NONE', *, *, #7921, .F. ) ;
#27842 = CARTESIAN_POINT ( 'NONE',  ( 43.89586892125429074, -24.33975351995231051, -0.9788672205760856615 ) ) ;
#27844 = VERTEX_POINT ( 'NONE', #4810 ) ;
#27845 = CARTESIAN_POINT ( 'NONE',  ( -0.9905328349288848866, -13.96290196142417628, 1.744688977348453740 ) ) ;
#27846 = EDGE_CURVE ( 'NONE', #30729, #15643, #11389, .T. ) ;
#27847 = AXIS2_PLACEMENT_3D ( 'NONE', #8793, #16456, #31719 ) ;
#27848 = AXIS2_PLACEMENT_3D ( 'NONE', #24642, #18831, #20150 ) ;
#27849 = ORIENTED_EDGE ( 'NONE', *, *, #18370, .F. ) ;
#27850 = CARTESIAN_POINT ( 'NONE',  ( 24.72695737054825926, 18.91229966141139229, -1.500000000000000000 ) ) ;
#27852 = ORIENTED_EDGE ( 'NONE', *, *, #10400, .F. ) ;
#27851 = CARTESIAN_POINT ( 'NONE',  ( -2.361419555135669590, 0.8502021591709224557, 3.209614657730603060 ) ) ;
#27853 = CIRCLE ( 'NONE', #1682, 0.5000000000000004441 ) ;
#27854 = DIRECTION ( 'NONE',  ( -1.000000000000000000, 0.000000000000000000, -0.000000000000000000 ) ) ;
#27855 = CARTESIAN_POINT ( 'NONE',  ( 0.000000000000000000, -1.425064293572261276, -10.85582367538895632 ) ) ;
#27856 = EDGE_CURVE ( 'NONE', #27014, #18253, #29033, .T. ) ;
#27857 = AXIS2_PLACEMENT_3D ( 'NONE', #23900, #3540, #6190 ) ;
#27858 = CARTESIAN_POINT ( 'NONE',  ( 0.000000000000000000, 0.000000000000000000, 1.500000000000000000 ) ) ;
#27859 = CARTESIAN_POINT ( 'NONE',  ( 10.00000000000000000, -0.2499999999999472089, -5.003758587302151284 ) ) ;
#27860 = CIRCLE ( 'NONE', #20404, 12.49867430706171767 ) ;
#27861 = VECTOR ( 'NONE', #24891, 1000.000000000000000 ) ;
#27862 = ORIENTED_EDGE ( 'NONE', *, *, #1379, .F. ) ;
#27863 = CARTESIAN_POINT ( 'NONE',  ( 21.48500000273118715, 0.2613211581691317065, 2.486304738420681559 ) ) ;
#27864 = DIRECTION ( 'NONE',  ( -1.000000000000000000, 0.000000000000000000, 0.000000000000000000 ) ) ;
#27865 = LINE ( 'NONE', #2127, #16595 ) ;
#27866 = DIRECTION ( 'NONE',  ( 0.9816271834476639757, 0.000000000000000000, 0.1908089953765452762 ) ) ;
#27867 = FACE_OUTER_BOUND ( 'NONE', #31547, .T. ) ;
#27868 = VECTOR ( 'NONE', #28955, 1000.000000000000000 ) ;
#27869 = DIRECTION ( 'NONE',  ( 0.000000000000000000, 0.8660254037844361541, 0.5000000000000041078 ) ) ;
#27870 = CARTESIAN_POINT ( 'NONE',  ( -56.33578448538598593, 0.003046479576510432215, -1.000000000003751888 ) ) ;
#27871 = CARTESIAN_POINT ( 'NONE',  ( 1.787149210215136508, -1.031811077599730231, 1.500000000000000000 ) ) ;
#27872 = ORIENTED_EDGE ( 'NONE', *, *, #16190, .T. ) ;
#27873 = VECTOR ( 'NONE', #17766, 1000.000000000000114 ) ;
#27874 = AXIS2_PLACEMENT_3D ( 'NONE', #23879, #21373, #8671 ) ;
#27875 = CARTESIAN_POINT ( 'NONE',  ( -6.962550801365593678, 2.228590825266444142, 2.752080473201636845 ) ) ;
#27876 = ORIENTED_EDGE ( 'NONE', *, *, #23034, .F. ) ;
#27877 = AXIS2_PLACEMENT_3D ( 'NONE', #30314, #7389, #15400 ) ;
#27878 = AXIS2_PLACEMENT_3D ( 'NONE', #25530, #7820, #14821 ) ;
#27879 = CARTESIAN_POINT ( 'NONE',  ( -8.304531657079156304, 2.975847129947406522, 0.3127741368606808403 ) ) ;
#27880 = CARTESIAN_POINT ( 'NONE',  ( 23.48500000136559862, 0.9349337715887185984, -3.156283516753368268 ) ) ;
#27881 = AXIS2_PLACEMENT_3D ( 'NONE', #8700, #3692, #26266 ) ;
#27882 = CARTESIAN_POINT ( 'NONE',  ( 110.2535626002996310, 19.41193660949216238, 0.4463807625373348298 ) ) ;
#27883 = CARTESIAN_POINT ( 'NONE',  ( 3.431351535095991334, -11.99437772339920016, 1.758550686115804895 ) ) ;
#27884 = CARTESIAN_POINT ( 'NONE',  ( 3.063284526839887167, -8.152713396088739017, -3.174628368996162298 ) ) ;
#27885 = AXIS2_PLACEMENT_3D ( 'NONE', #3150, #20855, #23218 ) ;
#27886 = ORIENTED_EDGE ( 'NONE', *, *, #7087, .T. ) ;
#27887 = CARTESIAN_POINT ( 'NONE',  ( 21.89609018930700302, -21.78725138646900561, 1.499999999999999778 ) ) ;
#27888 = CIRCLE ( 'NONE', #26804, 8.749000000000002331 ) ;
#27889 = LINE ( 'NONE', #22102, #20816 ) ;
#27890 = ORIENTED_EDGE ( 'NONE', *, *, #28056, .F. ) ;
#27891 = FACE_OUTER_BOUND ( 'NONE', #5084, .T. ) ;
#27892 = APPROVAL_STATUS ( 'not_yet_approved' ) ;
#27893 = CARTESIAN_POINT ( 'NONE',  ( 69.06169492441865998, -5.941118961410190913, 4.185348026735250748 ) ) ;
#27894 = EDGE_CURVE ( 'NONE', #29891, #24488, #16202, .T. ) ;
#27895 = ADVANCED_FACE ( 'NONE', ( #10141 ), #2766, .T. ) ;
#27896 = CARTESIAN_POINT ( 'NONE',  ( -10.00000000000000000, 0.000000000000000000, 0.000000000000000000 ) ) ;
#27897 = CIRCLE ( 'NONE', #1226, 8.749000000000002331 ) ;
#27899 = DIRECTION ( 'NONE',  ( 0.000000000000000000, 0.000000000000000000, -1.000000000000000000 ) ) ;
#27898 = CYLINDRICAL_SURFACE ( 'NONE', #28962, 6.000000000000000888 ) ;
#27900 = VECTOR ( 'NONE', #2565, 1000.000000000000000 ) ;
#27901 = ORIENTED_EDGE ( 'NONE', *, *, #4820, .F. ) ;
#27902 = AXIS2_PLACEMENT_3D ( 'NONE', #27198, #27385, #8831 ) ;
#27903 = FACE_OUTER_BOUND ( 'NONE', #18056, .T. ) ;
#27904 = CARTESIAN_POINT ( 'NONE',  ( 10.57125986779756843, -0.8254815157534942660, -4.681538312723525053 ) ) ;
#27905 = VECTOR ( 'NONE', #14171, 1000.000000000000000 ) ;
#27906 = CARTESIAN_POINT ( 'NONE',  ( 24.48500000136559507, 0.9349337715887185984, -3.156283516753368268 ) ) ;
#27907 = AXIS2_PLACEMENT_3D ( 'NONE', #29977, #7071, #2063 ) ;
#27908 = CARTESIAN_POINT ( 'NONE',  ( 18.53099130238707559, -16.42958907273965607, -1.499999999999999778 ) ) ;
#27910 = ORIENTED_EDGE ( 'NONE', *, *, #22336, .F. ) ;
#27909 = CARTESIAN_POINT ( 'NONE',  ( 107.5617944031221640, -18.98359742639815551, 4.522129901861158707 ) ) ;
#27911 = CARTESIAN_POINT ( 'NONE',  ( -7.312550801365594211, -1.088641768524163389, -3.675193018007246071 ) ) ;
#27912 = DIRECTION ( 'NONE',  ( 0.000000000000000000, 0.000000000000000000, 1.000000000000000000 ) ) ;
#27913 = CARTESIAN_POINT ( 'NONE',  ( -53.85782592458283347, 5.498961903950442931, 1.337771607534410601 ) ) ;
#27914 = CARTESIAN_POINT ( 'NONE',  ( 10.56870887191539587, -1.625881193364669297, -4.467071865485488402 ) ) ;
#27915 = AXIS2_PLACEMENT_3D ( 'NONE', #27561, #20550, #25540 ) ;
#27916 = EDGE_LOOP ( 'NONE', ( #27451, #12834, #28739, #6105 ) ) ;
#27918 = ORIENTED_EDGE ( 'NONE', *, *, #26984, .T. ) ;
#27917 = CARTESIAN_POINT ( 'NONE',  ( 0.000000000000000000, 4.709950686174755319, -9.884132761439010650 ) ) ;
#27919 = AXIS2_PLACEMENT_3D ( 'NONE', #11184, #21570, #28749 ) ;
#27920 = CARTESIAN_POINT ( 'NONE',  ( 14.89337309020629085, 18.05463290658611442, -1.491740999229419273 ) ) ;
#27921 = DIRECTION ( 'NONE',  ( 0.000000000000000000, 0.000000000000000000, -1.000000000000000000 ) ) ;
#27922 = CARTESIAN_POINT ( 'NONE',  ( 22.73500000136559862, 3.156283516753366047, 0.9349337715887203748 ) ) ;
#27923 = CARTESIAN_POINT ( 'NONE',  ( -30.17618327032176140, 10.26716432527324407, 1.977393880026174333 ) ) ;
#27924 = CARTESIAN_POINT ( 'NONE',  ( 5.492685119413638795, -18.11000744898911208, -1.500000000000157430 ) ) ;
#27925 = VECTOR ( 'NONE', #11815, 1000.000000000000000 ) ;
#27926 = CARTESIAN_POINT ( 'NONE',  ( 2.274274201625327230, 0.000000000000000000, 0.000000000000000000 ) ) ;
#27927 = B_SPLINE_CURVE_WITH_KNOTS ( 'NONE', 3,
 ( #16819, #3787, #1301, #8948, #11137, #21338, #29347, #9105, #19333, #15137 ),
 .UNSPECIFIED., .F., .F.,
 ( 4, 2, 2, 2, 4 ),
 ( -2.048411440084507189E-05, 0.0009701475628287921241, 0.001960779240058429466, 0.002951410917288066482, 0.003942042594517703932 ),
 .UNSPECIFIED. ) ;
#27928 = AXIS2_PLACEMENT_3D ( 'NONE', #29346, #4904, #8805 ) ;
#27929 = VECTOR ( 'NONE', #13423, 999.9999999999998863 ) ;
#27930 = CARTESIAN_POINT ( 'NONE',  ( 102.2233072702346277, -1.127920370132900807, 0.07017451552782195956 ) ) ;
#27931 = CARTESIAN_POINT ( 'NONE',  ( 18.68265047573912341, -6.724553502642427461, 4.522129901861162260 ) ) ;
#27932 = ORIENTED_EDGE ( 'NONE', *, *, #2657, .T. ) ;
#27933 = CARTESIAN_POINT ( 'NONE',  ( 0.000000000000000000, -7.851777359434021442, 3.255701506262407285 ) ) ;
#27934 = CIRCLE ( 'NONE', #1815, 5.009999999999999787 ) ;
#27935 = EDGE_CURVE ( 'NONE', #22300, #16325, #16322, .T. ) ;
#27936 = AXIS2_PLACEMENT_3D ( 'NONE', #27190, #17347, #27540 ) ;
#27937 = MECHANICAL_CONTEXT ( 'NONE', #20608, 'mechanical' ) ;
#27938 = DIRECTION ( 'NONE',  ( -0.03487826274237476598, -0.9987827659587182882, -0.03487826274237428026 ) ) ;
#27939 = ORIENTED_EDGE ( 'NONE', *, *, #29112, .F. ) ;
#27940 = SPHERICAL_SURFACE ( 'NONE', #17244, 0.5000000000000000000 ) ;
#27941 = EDGE_LOOP ( 'NONE', ( #6343, #29911, #18971, #6590 ) ) ;
#27942 = CARTESIAN_POINT ( 'NONE',  ( -21.98045600181102088, 18.26191254974343536, 1.777803877838809221 ) ) ;
#27944 = ORIENTED_EDGE ( 'NONE', *, *, #9460, .T. ) ;
#27943 = CARTESIAN_POINT ( 'NONE',  ( 28.69326080697081593, -5.628867125850868014, -4.013697994475298181 ) ) ;
#27945 = EDGE_CURVE ( 'NONE', #28295, #29275, #29048, .T. ) ;
#27946 = ORIENTED_EDGE ( 'NONE', *, *, #29823, .T. ) ;
#27947 = CARTESIAN_POINT ( 'NONE',  ( 111.3844470440328251, -20.20075132222358505, 1.500000000000000000 ) ) ;
#27948 = CARTESIAN_POINT ( 'NONE',  ( -6.562550801365594211, -2.228590825266444586, -2.752080473201636401 ) ) ;
#27949 = LINE ( 'NONE', #27761, #18834 ) ;
#27950 = CARTESIAN_POINT ( 'NONE',  ( 107.6641948605228123, -20.45809826282219746, -1.499999999999999556 ) ) ;
#27952 = EDGE_LOOP ( 'NONE', ( #20530, #23474, #12549, #16476, #20597 ) ) ;
#27951 = DIRECTION ( 'NONE',  ( -1.000000000000000000, -0.000000000000000000, 0.000000000000000000 ) ) ;
#27953 = VECTOR ( 'NONE', #19310, 1000.000000000000000 ) ;
#27954 = AXIS2_PLACEMENT_3D ( 'NONE', #20066, #13022, #10506 ) ;
#27955 = DIRECTION ( 'NONE',  ( -1.000000000000000000, 0.000000000000000000, 0.000000000000000000 ) ) ;
#27956 = FACE_OUTER_BOUND ( 'NONE', #11705, .T. ) ;
#27957 = ADVANCED_FACE ( 'NONE', ( #13788 ), #14063, .T. ) ;
#27958 = CARTESIAN_POINT ( 'NONE',  ( -0.05283608181216257332, -14.78963767087145698, 1.745421384833004019 ) ) ;
#27959 = CARTESIAN_POINT ( 'NONE',  ( 6.976285486575450001, -4.435383624113830692, -1.500000000000000000 ) ) ;
#27961 = ORIENTED_EDGE ( 'NONE', *, *, #3881, .T. ) ;
#27960 = CARTESIAN_POINT ( 'NONE',  ( 0.000000000000000000, 0.000000000000000000, 0.000000000000000000 ) ) ;
#27962 = DIRECTION ( 'NONE',  ( -1.000000000000000000, 0.000000000000000000, 0.000000000000000000 ) ) ;
#27963 = AXIS2_PLACEMENT_3D ( 'NONE', #10418, #20777, #30980 ) ;
#27964 = AXIS2_PLACEMENT_3D ( 'NONE', #30959, #23578, #6197 ) ;
#27965 = CARTESIAN_POINT ( 'NONE',  ( 107.3476768466457401, -15.88628154573096651, 1.500000000000000000 ) ) ;
#27966 = CARTESIAN_POINT ( 'NONE',  ( 22.86000000136559507, -0.9349337715887248157, 3.156283516753367824 ) ) ;
#27967 = CC_DESIGN_SECURITY_CLASSIFICATION ( #14051, ( #5017 ) ) ;
#27968 = CARTESIAN_POINT ( 'NONE',  ( 4.749760686538667009, -2.789499415801756586E-14, 8.014274990069656823 ) ) ;
#27969 = CARTESIAN_POINT ( 'NONE',  ( -6.112942406915326643, -3.366872799099910998E-15, -3.000000000000000000 ) ) ;
#27970 = FACE_OUTER_BOUND ( 'NONE', #15886, .T. ) ;
#27971 = VERTEX_POINT ( 'NONE', #18513 ) ;
#27972 = DIRECTION ( 'NONE',  ( 0.000000000000000000, 0.000000000000000000, 1.000000000000000000 ) ) ;
#27973 = EDGE_CURVE ( 'NONE', #12277, #2968, #6587, .T. ) ;
#27974 = CARTESIAN_POINT ( 'NONE',  ( 9.560873106162060372E-17, 1.115095498423308351, 4.884328206559839458 ) ) ;
#27975 = CARTESIAN_POINT ( 'NONE',  ( -7.937550801365593323, 3.368539882008727115, 1.828967928396027176 ) ) ;
#27976 = ORIENTED_EDGE ( 'NONE', *, *, #7221, .T. ) ;
#27977 = CIRCLE ( 'NONE', #24769, 0.5000000000000006661 ) ;
#27978 = CIRCLE ( 'NONE', #7697, 10.01806974338573752 ) ;
#27979 = CARTESIAN_POINT ( 'NONE',  ( 0.000000000000000000, -6.200809695932780308, 0.7745709230444962623 ) ) ;
#27980 = FACE_OUTER_BOUND ( 'NONE', #29169, .T. ) ;
#27981 = EDGE_CURVE ( 'NONE', #13793, #15643, #21516, .T. ) ;
#27982 = CARTESIAN_POINT ( 'NONE',  ( 6.356381451270080696, -8.587653982362812854, 0.5733789922931548100 ) ) ;
#27984 = ORIENTED_EDGE ( 'NONE', *, *, #2829, .T. ) ;
#27983 = CIRCLE ( 'NONE', #3956, 2.999999999999999112 ) ;
#27985 = CARTESIAN_POINT ( 'NONE',  ( 12.41789292056455274, -13.38018177111670504, 1.000000000000000000 ) ) ;
#27986 = EDGE_CURVE ( 'NONE', #11874, #5578, #12239, .T. ) ;
#27987 = ORIENTED_EDGE ( 'NONE', *, *, #26769, .F. ) ;
#27988 = CARTESIAN_POINT ( 'NONE',  ( 4.749760686538667009, -4.007137495034764463, -6.940565734314639634 ) ) ;
#27989 = ORIENTED_EDGE ( 'NONE', *, *, #201, .F. ) ;
#27990 = CARTESIAN_POINT ( 'NONE',  ( 2.274274201625327230, 1.464956435139694868, -10.90201369670497122 ) ) ;
#27992 = EDGE_LOOP ( 'NONE', ( #11510, #29308, #7873, #22531 ) ) ;
#27991 = DIRECTION ( 'NONE',  ( 1.000000000000000000, -0.000000000000000000, -0.000000000000000000 ) ) ;
#27993 = ORIENTED_EDGE ( 'NONE', *, *, #30405, .F. ) ;
#27994 = DIRECTION ( 'NONE',  ( -1.000000000000000000, -0.000000000000000000, 0.000000000000000000 ) ) ;
#27995 = LOCAL_TIME ( 16, 7, 10.00000000000000000, #4817 ) ;
#27996 = ADVANCED_FACE ( 'NONE', ( #13304 ), #26385, .T. ) ;
#27997 = EDGE_LOOP ( 'NONE', ( #16659, #18752, #28370, #28832, #2213 ) ) ;
#27998 = CARTESIAN_POINT ( 'NONE',  ( -0.2059365608663963898, 0.5000000000000000000, -1.000000000000000000 ) ) ;
#28000 = EDGE_LOOP ( 'NONE', ( #3824, #22499, #8179, #13997 ) ) ;
#27999 = CARTESIAN_POINT ( 'NONE',  ( 17.32050807568873552, 10.00000000000002309, -1.500000000000000000 ) ) ;
#28001 = CARTESIAN_POINT ( 'NONE',  ( 2.281627749324420140, -0.2935656086769634077, -1.757435426329174710 ) ) ;
#28002 = CARTESIAN_POINT ( 'NONE',  ( 21.70556107702375570, -21.76510136446086818, -1.556570398780113829 ) ) ;
#28003 = CARTESIAN_POINT ( 'NONE',  ( 48.01729800609908949, -4.703650321870251894, -4.522129901861162260 ) ) ;
#28004 = DIRECTION ( 'NONE',  ( 0.000000000000000000, 0.000000000000000000, 1.000000000000000000 ) ) ;
#28005 = ADVANCED_FACE ( 'NONE', ( #18358 ), #623, .T. ) ;
#28006 = AXIS2_PLACEMENT_3D ( 'NONE', #3954, #9937, #19999 ) ;
#28007 = LINE ( 'NONE', #22963, #1123 ) ;
#28008 = CARTESIAN_POINT ( 'NONE',  ( 3.500000000000000000, 0.000000000000000000, 0.000000000000000000 ) ) ;
#28009 = CARTESIAN_POINT ( 'NONE',  ( 25.14437127914493075, -17.52581659214492404, 1.374992938514359997 ) ) ;
#28010 = CARTESIAN_POINT ( 'NONE',  ( 18.62789956200952446, -21.71817389963752021, 0.9788672205877712029 ) ) ;
#28011 = CARTESIAN_POINT ( 'NONE',  ( 3.541509388326462116, -13.88765124358084968, 4.522129901861156931 ) ) ;
#28012 = B_SPLINE_CURVE_WITH_KNOTS ( 'NONE', 3,
 ( #15313, #28190, #20180, #20528, #12300, #10120, #17488, #17649, #7298, #120, #25181, #7639, #12145, #22344, #9814, #2299, #12489, #32901, #22698, #2473, #5292, #28040, #22515, #22845, #20032, #25366, #33047, #7448 ),
 .UNSPECIFIED., .F., .F.,
 ( 4, 3, 3, 3, 3, 3, 3, 3, 3, 4 ),
 ( 3.469446951953614189E-18, 0.0002206598333029125968, 0.0003690260377615042645, 0.0004687386537139015975, 0.0005359204132811800627, 0.0005814601065133845987, 0.0006257480493229339476, 0.0006439039612560342211, 0.0006584914725869980530, 0.0006666056854015675517 ),
 .UNSPECIFIED. ) ;
#28013 = CARTESIAN_POINT ( 'NONE',  ( -15.59081359172382975, -25.43932300454937945, 1.404595502311726696 ) ) ;
#28014 = CARTESIAN_POINT ( 'NONE',  ( 29.27523314209665628, -3.695744416148424971, 0.02339150516272637745 ) ) ;
#28015 = LOCAL_TIME ( 16, 7, 10.00000000000000000, #22501 ) ;
#28016 = DIRECTION ( 'NONE',  ( 1.000000000000000000, -0.000000000000000000, 0.000000000000000000 ) ) ;
#28017 = EDGE_CURVE ( 'NONE', #21952, #5917, #8626, .T. ) ;
#28018 = CARTESIAN_POINT ( 'NONE',  ( 0.000000000000000000, -9.241976615262146311, -1.699438267350472209 ) ) ;
#28019 = ORIENTED_EDGE ( 'NONE', *, *, #2552, .F. ) ;
#28020 = CARTESIAN_POINT ( 'NONE',  ( -4.187550801365593323, 0.3701630799359330593, -3.521866450007987037 ) ) ;
#28021 = ADVANCED_FACE ( 'NONE', ( #21034 ), #28706, .F. ) ;
#28022 = CARTESIAN_POINT ( 'NONE',  ( 3.499999999999999556, 4.058600654062948898, -7.468451026206158083 ) ) ;
#28023 = ORIENTED_EDGE ( 'NONE', *, *, #13748, .T. ) ;
#28024 = DIRECTION ( 'NONE',  ( -1.000000000000000000, 0.000000000000000000, 0.000000000000000000 ) ) ;
#28025 = CARTESIAN_POINT ( 'NONE',  ( -6.912942406915326465, 7.727249047114547632E-16, -2.999999999999999556 ) ) ;
#28026 = CIRCLE ( 'NONE', #20568, 5.009999999999999787 ) ;
#28027 = ORIENTED_EDGE ( 'NONE', *, *, #30553, .T. ) ;
#28028 = DIRECTION ( 'NONE',  ( -1.000000000000000000, -0.000000000000000000, -0.000000000000000000 ) ) ;
#28030 = ORIENTED_EDGE ( 'NONE', *, *, #18528, .T. ) ;
#28029 = CARTESIAN_POINT ( 'NONE',  ( -2.786590204610738031, -5.640011313469492471, -4.522129901861166701 ) ) ;
#28031 = ORIENTED_EDGE ( 'NONE', *, *, #27235, .T. ) ;
#28032 = CARTESIAN_POINT ( 'NONE',  ( -2.762703010982404006, -11.69547828613897700, 1.743724233132518675 ) ) ;
#28033 = B_SPLINE_CURVE_WITH_KNOTS ( 'NONE', 3,
 ( #17519, #17875, #9849, #27713, #4821, #25546 ),
 .UNSPECIFIED., .F., .F.,
 ( 4, 2, 4 ),
 ( 0.000000000000000000, 0.001111101127397922479, 0.002222202254795844958 ),
 .UNSPECIFIED. ) ;
#28034 = ORIENTED_EDGE ( 'NONE', *, *, #12601, .T. ) ;
#28035 = CARTESIAN_POINT ( 'NONE',  ( 3.499999999999999556, -7.851777359433977921, -3.255701506262513423 ) ) ;
#28037 = ORIENTED_EDGE ( 'NONE', *, *, #31259, .T. ) ;
#28036 = DIRECTION ( 'NONE',  ( 0.000000000000000000, 0.000000000000000000, 1.000000000000000000 ) ) ;
#28038 = CARTESIAN_POINT ( 'NONE',  ( 23.57316428367446193, -9.051964865574909425, 0.07017451552781803215 ) ) ;
#28039 = DIRECTION ( 'NONE',  ( 0.000000000000000000, 0.000000000000000000, 1.000000000000000000 ) ) ;
#28040 = CARTESIAN_POINT ( 'NONE',  ( 21.37407243444119942, -21.76038176774102695, -1.427857905595965926 ) ) ;
#28041 = CARTESIAN_POINT ( 'NONE',  ( 10.52034268205830614, 3.055657119358800244, 3.641590349731939735 ) ) ;
#28042 = ADVANCED_FACE ( 'NONE', ( #1788 ), #3968, .T. ) ;
#28043 = ORIENTED_EDGE ( 'NONE', *, *, #5783, .F. ) ;
#28044 = APPROVAL ( #11673, 'UNSPECIFIED' ) ;
#28045 = CARTESIAN_POINT ( 'NONE',  ( 6.524595623740805372, -6.215987993068485373, 6.028129343649593963 ) ) ;
#28046 = DIRECTION ( 'NONE',  ( -1.000000000000000000, -0.000000000000000000, 0.000000000000000000 ) ) ;
#28047 = DIRECTION ( 'NONE',  ( 0.000000000000000000, 0.2588190451025219607, -0.9659258262890679791 ) ) ;
#28048 = LINE ( 'NONE', #10318, #15153 ) ;
#28049 = CARTESIAN_POINT ( 'NONE',  ( -8.000050800000003903, -1.933527166425570432, 2.356997308372758226 ) ) ;
#28050 = CARTESIAN_POINT ( 'NONE',  ( -7.200050802731187360, -3.113457007523259268, 0.9222479816126455399 ) ) ;
#28051 = CARTESIAN_POINT ( 'NONE',  ( -56.30973635671871591, -3.699839913606783250E-14, -1.000000000020692115 ) ) ;
#28052 = CARTESIAN_POINT ( 'NONE',  ( 22.51665287054298403, -21.85882206146554552, 1.289857144952121448 ) ) ;
#28053 = ORIENTED_EDGE ( 'NONE', *, *, #8449, .F. ) ;
#28054 = CARTESIAN_POINT ( 'NONE',  ( -7.912550801365592967, 3.675193018007247403, -1.088641768524161391 ) ) ;
#28055 = ORIENTED_EDGE ( 'NONE', *, *, #31689, .F. ) ;
#28056 = EDGE_CURVE ( 'NONE', #4832, #17041, #16817, .T. ) ;
#28057 = CARTESIAN_POINT ( 'NONE',  ( -3.304531657079157192, -0.3127741368606806738, 2.975847129947406522 ) ) ;
#28058 = CARTESIAN_POINT ( 'NONE',  ( 22.67250000136559507, 3.024605502323846729, -0.3178988483021056854 ) ) ;
#28059 = EDGE_CURVE ( 'NONE', #32600, #29167, #16621, .T. ) ;
#28060 = CARTESIAN_POINT ( 'NONE',  ( 107.9510396086168811, 17.90552914680446506, 4.858489096870307833 ) ) ;
#28061 = DIRECTION ( 'NONE',  ( -0.000000000000000000, 1.000000000000000000, -0.000000000000000000 ) ) ;
#28062 = FACE_OUTER_BOUND ( 'NONE', #4173, .T. ) ;
#28063 = ORIENTED_EDGE ( 'NONE', *, *, #22164, .F. ) ;
#28064 = CARTESIAN_POINT ( 'NONE',  ( 22.00639167669143603, -21.80013755708273848, 1.500000000000000000 ) ) ;
#28065 = ORIENTED_EDGE ( 'NONE', *, *, #31082, .F. ) ;
#28066 = DIRECTION ( 'NONE',  ( -1.000000000000000000, -1.369475477426764022E-16, 0.000000000000000000 ) ) ;
#28067 = DATE_AND_TIME ( #23033, #13021 ) ;
#28068 = CARTESIAN_POINT ( 'NONE',  ( 69.06756016430726675, -6.058526890254189112, 4.073742241457220636 ) ) ;
#28069 = CARTESIAN_POINT ( 'NONE',  ( -28.35000000000000497, -10.96966150227469505, -1.500000000000000000 ) ) ;
#28071 = CARTESIAN_POINT ( 'NONE',  ( 5.377543748152550762, 7.530955069117551304, -2.741043480754851380 ) ) ;
#28070 = DIRECTION ( 'NONE',  ( -1.000000000000000000, 0.000000000000000000, 0.000000000000000000 ) ) ;
#28072 = ORIENTED_EDGE ( 'NONE', *, *, #22254, .F. ) ;
#28073 = CARTESIAN_POINT ( 'NONE',  ( -8.000050800000002127, -1.705663490921306646, -2.472570538722632882 ) ) ;
#28074 = CARTESIAN_POINT ( 'NONE',  ( 3.499999999999999556, -6.106419733535023653, 3.518755179752782958 ) ) ;
#28075 = CARTESIAN_POINT ( 'NONE',  ( 23.79750000136559507, 2.363507492473148286, 1.913930629741525058 ) ) ;
#28076 = CARTESIAN_POINT ( 'NONE',  ( -41.39035047991316674, -16.40843718609402302, 2.028141679950118625 ) ) ;
#28078 = ORIENTED_EDGE ( 'NONE', *, *, #12990, .F. ) ;
#28077 = CARTESIAN_POINT ( 'NONE',  ( 107.4385791398478744, 17.85938043952733878, 4.629213727441584325 ) ) ;
#28079 = CARTESIAN_POINT ( 'NONE',  ( -5.762550801365593500, -2.228590825266444586, -2.752080473201636401 ) ) ;
#28080 = CARTESIAN_POINT ( 'NONE',  ( 10.55147673363119232, -2.376879293651037006, -4.116875700062107235 ) ) ;
#28081 = CARTESIAN_POINT ( 'NONE',  ( 6.357668022120090079, -6.947679035623489874, 5.080751859797330461 ) ) ;
#28082 = FACE_OUTER_BOUND ( 'NONE', #23295, .T. ) ;
#28083 = VERTEX_POINT ( 'NONE', #32222 ) ;
#28085 = ORIENTED_EDGE ( 'NONE', *, *, #9768, .F. ) ;
#28084 = CARTESIAN_POINT ( 'NONE',  ( 24.37505892580042755, -17.33881490880317244, 1.312584468235632462 ) ) ;
#28086 = CARTESIAN_POINT ( 'NONE',  ( 5.377543748152548986, -4.007137495034764463, -6.940565734314639634 ) ) ;
#28087 = CARTESIAN_POINT ( 'NONE',  ( 2.970200414851742021, -8.870914041964216068, -2.288523046050828569 ) ) ;
#28088 = EDGE_CURVE ( 'NONE', #15521, #29681, #4456, .T. ) ;
#28089 = CARTESIAN_POINT ( 'NONE',  ( 23.11000000136559862, -2.892927487894331406, 1.570731468192932523 ) ) ;
#28090 = EDGE_CURVE ( 'NONE', #7526, #7281, #9288, .T. ) ;
#28091 = CARTESIAN_POINT ( 'NONE',  ( -24.48050464856543584, 3.520075575297991755, 1.500000000000000000 ) ) ;
#28092 = DIRECTION ( 'NONE',  ( -0.1767573132311711093, -0.9842544651762052954, 0.000000000000000000 ) ) ;
#28093 = DIRECTION ( 'NONE',  ( -0.000000000000000000, 0.9659258262890678681, 0.2588190451025219052 ) ) ;
#28094 = EDGE_CURVE ( 'NONE', #1557, #14743, #2340, .T. ) ;
#28095 = DIRECTION ( 'NONE',  ( 0.000000000000000000, 0.000000000000000000, 1.000000000000000000 ) ) ;
#28096 = DIRECTION ( 'NONE',  ( -1.000000000000000000, 0.000000000000000000, 0.000000000000000000 ) ) ;
#28097 = ORIENTED_EDGE ( 'NONE', *, *, #24276, .F. ) ;
#28098 = CARTESIAN_POINT ( 'NONE',  ( 18.96091535642496240, -3.614110606601101949, 2.184956778829998836 ) ) ;
#28099 = CARTESIAN_POINT ( 'NONE',  ( 85.20563808598696198, -3.194259795296082949, 4.522129901861162260 ) ) ;
#28100 = VERTEX_POINT ( 'NONE', #6779 ) ;
#28101 = CARTESIAN_POINT ( 'NONE',  ( -6.962942409646511344, 7.727249047114547632E-16, -2.999999999999999556 ) ) ;
#28102 = ORIENTED_EDGE ( 'NONE', *, *, #7967, .T. ) ;
#28103 = CARTESIAN_POINT ( 'NONE',  ( -16.95333583173749759, 10.33954000514843585, 1.975604575489919412 ) ) ;
#28105 = VERTEX_POINT ( 'NONE', #4272 ) ;
#28104 = CARTESIAN_POINT ( 'NONE',  ( 40.87775850016843293, -5.753518027302250815, -4.001040184496583052 ) ) ;
#28106 = ORIENTED_EDGE ( 'NONE', *, *, #10529, .T. ) ;
#28107 = CARTESIAN_POINT ( 'NONE',  ( -4.365512850963738423, -6.230587388684557304, -1.500000000000000000 ) ) ;
#28108 = CARTESIAN_POINT ( 'NONE',  ( -7.612550801365594033, -1.828967928396026732, 3.368539882008728004 ) ) ;
#28109 = CARTESIAN_POINT ( 'NONE',  ( 6.038145077921539539, -8.106170535363467877, 2.472816103755222095 ) ) ;
#28110 = B_SPLINE_CURVE_WITH_KNOTS ( 'NONE', 3,
 ( #7458, #24867, #4986, #1825, #17498, #7307, #22203, #9473, #19688, #14669 ),
 .UNSPECIFIED., .F., .F.,
 ( 4, 2, 2, 2, 4 ),
 ( 3.512955446118278440E-07, 0.0005479535487287108021, 0.001095555801912809820, 0.001643158055096908838, 0.002190760308281007856 ),
 .UNSPECIFIED. ) ;
#28111 = CARTESIAN_POINT ( 'NONE',  ( 4.749760686538667009, -5.151476664237518044, 6.139290821770238438 ) ) ;
#28113 = EDGE_LOOP ( 'NONE', ( #23927, #27708, #6408 ) ) ;
#28112 = CARTESIAN_POINT ( 'NONE',  ( 22.05656763645045260, 0.8852964313267434049, -2.499999999999998224 ) ) ;
#28114 = FACE_OUTER_BOUND ( 'NONE', #7234, .T. ) ;
#28115 = CARTESIAN_POINT ( 'NONE',  ( 0.8407900506754618641, -11.56055812333405441, 4.522129901861156931 ) ) ;
#28116 = CARTESIAN_POINT ( 'NONE',  ( -0.3079966392002160824, -15.09887389677487057, 1.500000000000000444 ) ) ;
#28117 = CARTESIAN_POINT ( 'NONE',  ( 21.04750000136559507, -1.913930629741527500, 2.363507492473149618 ) ) ;
#28118 = DIRECTION ( 'NONE',  ( -1.000000000000000000, 0.000000000000000000, 0.000000000000000000 ) ) ;
#28120 = VERTEX_POINT ( 'NONE', #12127 ) ;
#28119 = CARTESIAN_POINT ( 'NONE',  ( 108.0284341522745137, -18.47880683584480366, -4.354933216522902661 ) ) ;
#28121 = CARTESIAN_POINT ( 'NONE',  ( -35.00000000000000000, 18.00000000000000355, -0.3702070605508915868 ) ) ;
#28122 = ADVANCED_FACE ( 'NONE', ( #22174 ), #22324, .F. ) ;
#28123 = LINE ( 'NONE', #18248, #12378 ) ;
#28124 = CARTESIAN_POINT ( 'NONE',  ( 22.54750000136559507, 3.024605502323846729, -0.3178988483021056854 ) ) ;
#28125 = DIRECTION ( 'NONE',  ( -1.000000000000000000, -0.000000000000000000, -0.000000000000000000 ) ) ;
#28126 = FACE_OUTER_BOUND ( 'NONE', #8657, .T. ) ;
#28127 = CARTESIAN_POINT ( 'NONE',  ( -38.14293509397969473, 10.97000000000000419, 1.500000000000000000 ) ) ;
#28128 = ORIENTED_EDGE ( 'NONE', *, *, #2985, .T. ) ;
#28129 = CARTESIAN_POINT ( 'NONE',  ( 107.9823351630856934, -17.81499285951132094, 4.403864951703802433 ) ) ;
#28130 = CARTESIAN_POINT ( 'NONE',  ( -34.31843563627105453, 19.51744974835125035, 1.977928362984241017 ) ) ;
#28131 = CARTESIAN_POINT ( 'NONE',  ( -4.937550801365593323, 1.828967928396027398, -3.368539882008727115 ) ) ;
#28132 = ORIENTED_EDGE ( 'NONE', *, *, #17651, .F. ) ;
#28133 = CARTESIAN_POINT ( 'NONE',  ( -10.00000000000000000, 0.000000000000000000, 0.000000000000000000 ) ) ;
#28134 = CARTESIAN_POINT ( 'NONE',  ( 7.249760686538667009, 7.906491560603716273, -3.748318449932209973 ) ) ;
#28135 = CARTESIAN_POINT ( 'NONE',  ( 3.541509388326463004, -13.88765124358303993, -4.522129901861164925 ) ) ;
#28136 = CARTESIAN_POINT ( 'NONE',  ( 48.09670199522223299, -9.430894477028838097, 0.07017451552781736601 ) ) ;
#28137 = ORIENTED_EDGE ( 'NONE', *, *, #22854, .F. ) ;
#28138 = CARTESIAN_POINT ( 'NONE',  ( 0.000000000000000000, -4.709950686174546597, -9.884132761439110126 ) ) ;
#28139 = ORIENTED_EDGE ( 'NONE', *, *, #16016, .T. ) ;
#28140 = CARTESIAN_POINT ( 'NONE',  ( -2.863349216192397240, 0.2791979387067812235, 0.7890172491793814302 ) ) ;
#28142 = VERTEX_POINT ( 'NONE', #26851 ) ;
#28141 = DIRECTION ( 'NONE',  ( -7.472768010111142456E-18, -0.08715574274765799934, -0.9961946980917455452 ) ) ;
#28143 = ADVANCED_FACE ( 'NONE', ( #21822 ), #1601, .T. ) ;
#28144 = EDGE_LOOP ( 'NONE', ( #33038, #20176, #2866, #29966 ) ) ;
#28145 = DIRECTION ( 'NONE',  ( 1.000000000000000000, 0.000000000000000000, 1.734723475976805517E-15 ) ) ;
#28146 = ORIENTED_EDGE ( 'NONE', *, *, #10169, .F. ) ;
#28147 = CARTESIAN_POINT ( 'NONE',  ( 34.71268046341646141, -0.06979899340500209104, -1.021976849372817631 ) ) ;
#28149 = ORIENTED_EDGE ( 'NONE', *, *, #9841, .F. ) ;
#28148 = DIRECTION ( 'NONE',  ( -0.8660254037844409281, 0.4999999999999960587, 0.000000000000000000 ) ) ;
#28150 = CARTESIAN_POINT ( 'NONE',  ( 0.2695511591073790347, -5.141785308971643431, -1.768807166514833051 ) ) ;
#28151 = EDGE_CURVE ( 'NONE', #11370, #21301, #7126, .T. ) ;
#28152 = CARTESIAN_POINT ( 'NONE',  ( 22.51665287054355957, -21.85882206146509432, -1.289857144951130907 ) ) ;
#28153 = CARTESIAN_POINT ( 'NONE',  ( 17.02282544802299213, -15.06900748016021652, -1.500000000000277334 ) ) ;
#28154 = CARTESIAN_POINT ( 'NONE',  ( 7.249760686538667009, 0.8180878109961843281, 8.711672189281429723 ) ) ;
#28155 = DIRECTION ( 'NONE',  ( 1.000000000000000000, 0.000000000000000000, 7.709882115452493155E-15 ) ) ;
#28156 = CARTESIAN_POINT ( 'NONE',  ( -3.691545173129016004E-13, 1.425064293572904539, 10.85582367538961535 ) ) ;
#28157 = CARTESIAN_POINT ( 'NONE',  ( 0.8195958019639205672, -4.591973786415240788, 1.500000000000000000 ) ) ;
#28158 = CARTESIAN_POINT ( 'NONE',  ( 69.12694021457090798, -7.241784863855947663, 2.184957268890977300 ) ) ;
#28159 = ADVANCED_FACE ( 'NONE', ( #14446 ), #19661, .T. ) ;
#28160 = EDGE_CURVE ( 'NONE', #18680, #6546, #1058, .T. ) ;
#28161 = CARTESIAN_POINT ( 'NONE',  ( 0.000000000000000000, 0.000000000000000000, 0.000000000000000000 ) ) ;
#28162 = CARTESIAN_POINT ( 'NONE',  ( 41.20585001718148277, -8.497180311781159290, -0.07017451552783579571 ) ) ;
#28163 = DIRECTION ( 'NONE',  ( 1.000000000000000000, 0.000000000000000000, 0.000000000000000000 ) ) ;
#28164 =( BOUNDED_SURFACE ( )  B_SPLINE_SURFACE ( 1, 3, ( 
 ( #29521, #26661, #31867, #11776 ),
 ( #21660, #21980, #1772, #3771 ) ),
 .UNSPECIFIED., .F., .F., .F. ) 
 B_SPLINE_SURFACE_WITH_KNOTS ( ( 2, 2 ),
 ( 4, 4 ),
 ( 0.000000000000000000, 1.000000000000000000 ),
 ( 0.000000000000000000, 1.000000000000000000 ),
 .UNSPECIFIED. ) 
 GEOMETRIC_REPRESENTATION_ITEM ( )  RATIONAL_B_SPLINE_SURFACE ( (
 ( 1.000000000000000000, 0.9321687722090974404, 0.9321687722090974404, 1.000000000000000000),
 ( 1.000000000000000000, 0.9321687722090974404, 0.9321687722090974404, 1.000000000000000000) ) ) 
 REPRESENTATION_ITEM ( '' )  SURFACE ( )  );
#28165 = CARTESIAN_POINT ( 'NONE',  ( 41.43709133142961321, -4.769546740945158625, 4.522129901861162260 ) ) ;
#28166 = EDGE_CURVE ( 'NONE', #5237, #26955, #22678, .T. ) ;
#28167 = CARTESIAN_POINT ( 'NONE',  ( -2.100050802731186828, 1.549418761218566143, -2.853674364686379583 ) ) ;
#28168 = ORIENTED_EDGE ( 'NONE', *, *, #11415, .F. ) ;
#28169 = CARTESIAN_POINT ( 'NONE',  ( -6.737550801365594033, -3.368539882008727115, -1.828967928396028064 ) ) ;
#28170 = LINE ( 'NONE', #22978, #15692 ) ;
#28171 = CARTESIAN_POINT ( 'NONE',  ( 18.75828436641558028, -5.879118399717574661, -3.993434336035625254 ) ) ;
#28172 = VERTEX_POINT ( 'NONE', #22825 ) ;
#28173 = CARTESIAN_POINT ( 'NONE',  ( 69.09268213438591033, -2.232183665269761086, -0.07017451552781628354 ) ) ;
#28174 =( NAMED_UNIT ( * ) PLANE_ANGLE_UNIT ( ) SI_UNIT ( $, .RADIAN. ) );
#28175 = EDGE_CURVE ( 'NONE', #8919, #16210, #21536, .T. ) ;
#28176 = VERTEX_POINT ( 'NONE', #12956 ) ;
#28177 = CARTESIAN_POINT ( 'NONE',  ( 3.249999999999999556, 0.000000000000000000, 0.000000000000000000 ) ) ;
#28178 = CONTEXT_DEPENDENT_SHAPE_REPRESENTATION ( #26151, #23137 ) ;
#28180 = ORIENTED_EDGE ( 'NONE', *, *, #26158, .F. ) ;
#28179 = CARTESIAN_POINT ( 'NONE',  ( 18.60402535543785518, -7.603424548862136589, 0.07017451552781736601 ) ) ;
#28181 = ORIENTED_EDGE ( 'NONE', *, *, #3149, .T. ) ;
#28182 = CARTESIAN_POINT ( 'NONE',  ( 0.9573829800795973233, -15.55580343830457579, 1.746220095277639661 ) ) ;
#28183 = ORIENTED_EDGE ( 'NONE', *, *, #22854, .T. ) ;
#28184 = LINE ( 'NONE', #3126, #603 ) ;
#28186 = VERTEX_POINT ( 'NONE', #30717 ) ;
#28185 = CARTESIAN_POINT ( 'NONE',  ( 10.52034268205830614, -3.993798362933330015, 3.024842911000676704 ) ) ;
#28187 = CARTESIAN_POINT ( 'NONE',  ( 29.21519671786122885, -8.552672223064927692, 2.713652344655544724 ) ) ;
#28188 = CYLINDRICAL_SURFACE ( 'NONE', #2674, 2.999999999999999112 ) ;
#28189 = ADVANCED_FACE ( 'NONE', ( #7428 ), #17469, .T. ) ;
#28190 = CARTESIAN_POINT ( 'NONE',  ( 21.93333526462830108, -21.79160260970720131, -1.500000000000028644 ) ) ;
#28191 = DIRECTION ( 'NONE',  ( 0.000000000000000000, 0.000000000000000000, -1.000000000000000000 ) ) ;
#28192 = ORIENTED_EDGE ( 'NONE', *, *, #20016, .F. ) ;
#28193 = CYLINDRICAL_SURFACE ( 'NONE', #23511, 3.250000000000002665 ) ;
#28194 = CARTESIAN_POINT ( 'NONE',  ( -4.207304909706596874, 1.062355717592091686, 3.000000000000001332 ) ) ;
#28195 = CARTESIAN_POINT ( 'NONE',  ( 23.62691144362026563, -7.794821506207252781, -1.529339877372910550 ) ) ;
#28196 = PLANE ( 'NONE',  #15177 ) ;
#28197 = ADVANCED_FACE ( 'NONE', ( #98 ), #2278, .T. ) ;
#28198 = EDGE_CURVE ( 'NONE', #29792, #10525, #3416, .T. ) ;
#28199 = CARTESIAN_POINT ( 'NONE',  ( 23.21956321516963229, -21.93898040685625972, 1.019910856439967706 ) ) ;
#28200 = DIRECTION ( 'NONE',  ( 0.000000000000000000, 0.000000000000000000, -1.000000000000000000 ) ) ;
#28201 = CARTESIAN_POINT ( 'NONE',  ( -56.35610254884790038, 0.001801644430070462348, -1.071919094844493214 ) ) ;
#28202 = FACE_OUTER_BOUND ( 'NONE', #8727, .T. ) ;
#28203 = ORIENTED_EDGE ( 'NONE', *, *, #1440, .F. ) ;
#28204 = CARTESIAN_POINT ( 'NONE',  ( -7.562550801365593323, -2.752080473201636845, 2.228590825266444586 ) ) ;
#28205 = ORIENTED_EDGE ( 'NONE', *, *, #22219, .F. ) ;
#28206 = CARTESIAN_POINT ( 'NONE',  ( -4.154531657079156837, 0.9198621039125853827, 3.105402419394639235 ) ) ;
#28207 = DIRECTION ( 'NONE',  ( 0.08343273266574956215, 0.4645863764670183360, 0.8815886103626631165 ) ) ;
#28208 = CARTESIAN_POINT ( 'NONE',  ( 107.9802527803231129, -17.78500706576168611, -4.325704939595124365 ) ) ;
#28209 = CARTESIAN_POINT ( 'NONE',  ( 19.46384663048941377, -15.80031286559597703, 1.500000000000000000 ) ) ;
#28210 = ORIENTED_EDGE ( 'NONE', *, *, #5684, .F. ) ;
#28211 = DIRECTION ( 'NONE',  ( 1.000000000000000000, 0.000000000000000000, 0.000000000000000000 ) ) ;
#28212 = EDGE_CURVE ( 'NONE', #30361, #14569, #32710, .T. ) ;
#28213 = PRODUCT_DEFINITION ( 'UNKNOWN', '', #2373, #29298 ) ;
#28214 = VERTEX_POINT ( 'NONE', #9948 ) ;
#28215 = CARTESIAN_POINT ( 'NONE',  ( 1.997966851997896143, -1.624780761253489691, 1.499999999999999556 ) ) ;
#28216 = PERSON_AND_ORGANIZATION ( #6766, #25292 ) ;
#28217 = CARTESIAN_POINT ( 'NONE',  ( 85.02775175690295839, -5.073181109254185195, 4.150065216364585474 ) ) ;
#28218 = CARTESIAN_POINT ( 'NONE',  ( -56.28351068136514357, 0.000000000000000000, -1.000000000000000000 ) ) ;
#28220 = CARTESIAN_POINT ( 'NONE',  ( 33.81874022276150527, 19.50000000000000000, -1.977928362984232802 ) ) ;
#28219 = CARTESIAN_POINT ( 'NONE',  ( -4.599999999999996980, 1.224646799147353256E-15, 10.00000000000000178 ) ) ;
#28221 = ORIENTED_EDGE ( 'NONE', *, *, #16236, .T. ) ;
#28222 = DIRECTION ( 'NONE',  ( 8.574039729943018344E-17, 1.000000000000000000, 0.000000000000000000 ) ) ;
#28223 = LINE ( 'NONE', #12677, #9656 ) ;
#28224 = EDGE_CURVE ( 'NONE', #16893, #6314, #13821, .T. ) ;
#28225 = CARTESIAN_POINT ( 'NONE',  ( 22.04750000136559507, -1.913930629741527500, 2.363507492473149618 ) ) ;
#28226 = CARTESIAN_POINT ( 'NONE',  ( 19.74803318911342487, -17.01893862700759641, -1.753250791794231933 ) ) ;
#28228 = EDGE_LOOP ( 'NONE', ( #7312, #8689, #4031, #11592 ) ) ;
#28227 = DIRECTION ( 'NONE',  ( 7.023442172597885211E-17, 0.8191520442889951292, -0.5735764363510412744 ) ) ;
#28229 = CARTESIAN_POINT ( 'NONE',  ( -4.962550801365593678, -2.228590825266444586, -2.752080473201636401 ) ) ;
#28230 = DIRECTION ( 'NONE',  ( -1.000000000000000000, 0.000000000000000000, 0.000000000000000000 ) ) ;
#28231 = CARTESIAN_POINT ( 'NONE',  ( 18.68265047573912341, -6.724553502642427461, -4.522129901861164036 ) ) ;
#28232 = CARTESIAN_POINT ( 'NONE',  ( 21.80656763371926488, 0.8852964313267427388, -2.499999999999999112 ) ) ;
#28233 = EDGE_LOOP ( 'NONE', ( #18585, #15606, #29824 ) ) ;
#28234 = VERTEX_POINT ( 'NONE', #14946 ) ;
#28235 = B_SPLINE_CURVE_WITH_KNOTS ( 'NONE', 3,
 ( #306, #14814, #10123, #20690, #12645, #25012, #28045, #12792, #25685, #32905 ),
 .UNSPECIFIED., .F., .F.,
 ( 4, 2, 2, 2, 4 ),
 ( 2.493548413911061648E-07, 0.0005478513795029421162, 0.001095453404164493244, 0.001643055428826044372, 0.002190657453487595066 ),
 .UNSPECIFIED. ) ;
#28236 = CARTESIAN_POINT ( 'NONE',  ( -35.00000000000000000, 0.5000000000000000000, -2.482234843104710986 ) ) ;
#28237 = DIRECTION ( 'NONE',  ( 0.000000000000000000, 0.8090169943749485615, -0.5877852522924714718 ) ) ;
#28238 = CARTESIAN_POINT ( 'NONE',  ( 21.48500000136559507, 0.9349337715887185984, -3.156283516753368268 ) ) ;
#28239 = DIRECTION ( 'NONE',  ( -0.000000000000000000, -1.000000000000000000, -0.000000000000000000 ) ) ;
#28240 = DIRECTION ( 'NONE',  ( 0.000000000000000000, 0.000000000000000000, 1.000000000000000000 ) ) ;
#28241 = CARTESIAN_POINT ( 'NONE',  ( 10.56870887191539587, -1.625881193364728805, 4.467071865485467086 ) ) ;
#28242 = CARTESIAN_POINT ( 'NONE',  ( 102.5437075123491866, -5.726773290143885475, 0.07017451552782749680 ) ) ;
#28243 = ORIENTED_EDGE ( 'NONE', *, *, #11320, .T. ) ;
#28244 = CARTESIAN_POINT ( 'NONE',  ( 84.41210159610582764, -2.963446145457933945, 2.184954676747139057 ) ) ;
#28245 = EDGE_CURVE ( 'NONE', #24410, #11079, #25843, .T. ) ;
#28246 = APPROVAL_ROLE ( '' ) ;
#28247 = CARTESIAN_POINT ( 'NONE',  ( 102.6609843814833027, -1.982062027707615970, 4.522129901861162260 ) ) ;
#28248 = ORIENTED_EDGE ( 'NONE', *, *, #20079, .T. ) ;
#28249 = CARTESIAN_POINT ( 'NONE',  ( 107.6454888467326469, 19.04626834818095915, -4.993545475007672430 ) ) ;
#28250 = ORIENTED_EDGE ( 'NONE', *, *, #27321, .T. ) ;
#28251 = CARTESIAN_POINT ( 'NONE',  ( -17.23523782256200576, 9.003349235486576063, 2.010613759594101602 ) ) ;
#28253 = ORIENTED_EDGE ( 'NONE', *, *, #12649, .T. ) ;
#28252 = CARTESIAN_POINT ( 'NONE',  ( 40.87896744413788497, -5.974071964835635740, -4.215290092872233885 ) ) ;
#28254 = ORIENTED_EDGE ( 'NONE', *, *, #15706, .F. ) ;
#28255 = EDGE_CURVE ( 'NONE', #22155, #18469, #13008, .T. ) ;
#28256 = DIRECTION ( 'NONE',  ( 1.000000000000000000, 0.000000000000000000, 0.000000000000000000 ) ) ;
#28257 = CARTESIAN_POINT ( 'NONE',  ( -7.662550801365593856, -0.3701630799359326152, 3.521866450007987037 ) ) ;
#28258 = EDGE_CURVE ( 'NONE', #6237, #9415, #16755, .T. ) ;
#28259 = CARTESIAN_POINT ( 'NONE',  ( -1.394036994807634510E-16, -1.625881193364727917, 4.467071865485467086 ) ) ;
#28260 = CARTESIAN_POINT ( 'NONE',  ( 102.9885081044300676, -6.698322160490901567, -1.010822989962099960 ) ) ;
#28261 = VECTOR ( 'NONE', #30551, 1000.000000000000000 ) ;
#28263 = EDGE_LOOP ( 'NONE', ( #1931, #25276, #22945, #24595, #21306, #30927 ) ) ;
#28262 = DIRECTION ( 'NONE',  ( 0.000000000000000000, 1.000000000000000000, 0.000000000000000000 ) ) ;
#28264 = DIRECTION ( 'NONE',  ( 0.000000000000000000, 0.000000000000000000, -1.000000000000000000 ) ) ;
#28265 = CARTESIAN_POINT ( 'NONE',  ( 0.1517578099452172036, -1.375880305419571625, 4.522129901861156931 ) ) ;
#28266 = ADVANCED_FACE ( 'NONE', ( #27833 ), #2604, .T. ) ;
#28267 = CARTESIAN_POINT ( 'NONE',  ( -4.499052284343287411, -5.402383032670722507, 1.499999999999999556 ) ) ;
#28268 = CARTESIAN_POINT ( 'NONE',  ( 23.54750000136559507, 3.024605502323846729, -0.3178988483021056854 ) ) ;
#28270 = ORIENTED_EDGE ( 'NONE', *, *, #327, .F. ) ;
#28269 = CARTESIAN_POINT ( 'NONE',  ( 18.64036474505168428, -7.197223105181163483, -1.868788737152627277 ) ) ;
#28271 = CARTESIAN_POINT ( 'NONE',  ( 25.52557118915447987, -17.56218954043521663, 1.000000000000000000 ) ) ;
#28272 = CARTESIAN_POINT ( 'NONE',  ( -25.35132950642825733, 18.20714672489456731, 1.779116719942482883 ) ) ;
#28273 = CARTESIAN_POINT ( 'NONE',  ( 21.54750000136559507, 3.024605502323846729, -0.3178988483021056854 ) ) ;
#28274 = LINE ( 'NONE', #529, #19367 ) ;
#28275 = AXIS2_PLACEMENT_3D ( 'NONE', #8912, #1257, #16600 ) ;
#28276 = CARTESIAN_POINT ( 'NONE',  ( 6.524595551582241804, 7.168326838405008061, -4.857153507487872446 ) ) ;
#28277 = FACE_OUTER_BOUND ( 'NONE', #8230, .T. ) ;
#28278 = ORIENTED_EDGE ( 'NONE', *, *, #14056, .F. ) ;
#28279 = CARTESIAN_POINT ( 'NONE',  ( -52.69999999999999574, -10.96966150227468972, 0.9999999999999991118 ) ) ;
#28280 = VECTOR ( 'NONE', #11598, 1000.000000000000000 ) ;
#28281 = CARTESIAN_POINT ( 'NONE',  ( 3.499999999999999556, 6.226349476952025341, -0.5315761383463578627 ) ) ;
#28282 = ORIENTED_EDGE ( 'NONE', *, *, #15669, .T. ) ;
#28283 = CIRCLE ( 'NONE', #12, 0.5000000000000000000 ) ;
#28284 = CARTESIAN_POINT ( 'NONE',  ( -53.12500000000000000, -10.96966150227468972, 7.500000000000000000 ) ) ;
#28285 = CARTESIAN_POINT ( 'NONE',  ( 7.249760686538667009, -8.437262856154147173, -2.318425219014316419 ) ) ;
#28286 = DIRECTION ( 'NONE',  ( 1.000000000000000000, -8.574039729943018344E-17, -0.000000000000000000 ) ) ;
#28288 = CARTESIAN_POINT ( 'NONE',  ( 107.9692545707511471, -17.62663558376400985, 4.957402666611876008 ) ) ;
#28287 = CARTESIAN_POINT ( 'NONE',  ( 13.56547938923340624, -13.86701005029668288, 1.000000000000000222 ) ) ;
#28289 = ORIENTED_EDGE ( 'NONE', *, *, #27935, .F. ) ;
#28290 = EDGE_CURVE ( 'NONE', #28620, #17825, #28170, .T. ) ;
#28291 = CARTESIAN_POINT ( 'NONE',  ( 10.55147673363118876, -4.208382051008173974, -2.718385644597219208 ) ) ;
#28292 = ORIENTED_EDGE ( 'NONE', *, *, #29748, .F. ) ;
#28293 = CARTESIAN_POINT ( 'NONE',  ( 41.44907012423725234, -8.741883605793594469, 2.713652344655544724 ) ) ;
#28295 = VERTEX_POINT ( 'NONE', #20506 ) ;
#28294 = FACE_OUTER_BOUND ( 'NONE', #32713, .T. ) ;
#28296 = VERTEX_POINT ( 'NONE', #20665 ) ;
#28297 = DIRECTION ( 'NONE',  ( 1.000000000000000000, -0.000000000000000000, -0.000000000000000000 ) ) ;
#28298 = EDGE_CURVE ( 'NONE', #9752, #5237, #728, .T. ) ;
#28299 = EDGE_CURVE ( 'NONE', #3652, #19151, #8103, .T. ) ;
#28300 = EDGE_CURVE ( 'NONE', #17857, #17891, #26157, .T. ) ;
#28301 = CIRCLE ( 'NONE', #13343, 5.009999999999999787 ) ;
#28302 = FACE_OUTER_BOUND ( 'NONE', #6332, .T. ) ;
#28304 = ORIENTED_EDGE ( 'NONE', *, *, #21592, .T. ) ;
#28303 = CARTESIAN_POINT ( 'NONE',  ( 16.80274661516410006, -16.53680364986711737, -1.500000000000000000 ) ) ;
#28305 = EDGE_LOOP ( 'NONE', ( #20104, #15777, #760, #12468, #26990 ) ) ;
#28306 = VECTOR ( 'NONE', #23783, 1000.000000000000000 ) ;
#28307 = DIRECTION ( 'NONE',  ( 7.770718973608924422E-17, 0.9063077870366440525, 0.4226182617407120978 ) ) ;
#28308 = CARTESIAN_POINT ( 'NONE',  ( 22.04243029793069297, -21.80478118307112823, -1.499729010652245620 ) ) ;
#28309 = CARTESIAN_POINT ( 'NONE',  ( 108.0821972398987327, -20.20655521172199798, -1.448620529800456191 ) ) ;
#28310 = CARTESIAN_POINT ( 'NONE',  ( 10.52034268205830614, -3.024842911000663825, -3.993798362933340229 ) ) ;
#28311 = CARTESIAN_POINT ( 'NONE',  ( 107.9766672148941495, -17.73337581556108233, 4.219849370640194053 ) ) ;
#28312 = CIRCLE ( 'NONE', #17106, 0.4499999999999983458 ) ;
#28313 = CARTESIAN_POINT ( 'NONE',  ( 10.00000000000000000, -4.467071865485484850, 1.625881193364682620 ) ) ;
#28314 = CARTESIAN_POINT ( 'NONE',  ( 3.065837323883517929, -11.21675834388424065, 1.499999999999999778 ) ) ;
#28315 = CARTESIAN_POINT ( 'NONE',  ( 54.99820130842444144, -7.257205178600759865, 2.787782628536179530 ) ) ;
#28316 = LINE ( 'NONE', #17804, #17669 ) ;
#28317 = CARTESIAN_POINT ( 'NONE',  ( 2.274274201625327230, -10.90201369670499609, 1.464956435139503022 ) ) ;
#28318 = CARTESIAN_POINT ( 'NONE',  ( 101.6022419886208610, -1.170867242066747416, 0.07017451552782490165 ) ) ;
#28319 = CARTESIAN_POINT ( 'NONE',  ( 6.524595126109738352, -8.613374939462820734, -0.8869162863045405576 ) ) ;
#28320 = CARTESIAN_POINT ( 'NONE',  ( 3.499999999999999556, 4.137773741518454784, -5.705158055754753654 ) ) ;
#28321 = ORIENTED_EDGE ( 'NONE', *, *, #30206, .T. ) ;
#28322 = CARTESIAN_POINT ( 'NONE',  ( -7.187550801365593323, 3.521866450007987037, 0.3701630799359328372 ) ) ;
#28323 = AXIS2_PLACEMENT_3D ( 'NONE', #17029, #8863, #22389 ) ;
#28324 = CIRCLE ( 'NONE', #13344, 10.95101833074431852 ) ;
#28325 = B_SPLINE_CURVE_WITH_KNOTS ( 'NONE', 3,
 ( #21635, #19290, #29002, #18796, #9063, #14252, #8429, #29156 ),
 .UNSPECIFIED., .F., .F.,
 ( 4, 2, 2, 4 ),
 ( 2.213836054372184116E-07, 0.001261154818855338578, 0.001891621536480289894, 0.002522088254105241210 ),
 .UNSPECIFIED. ) ;
#28326 = ADVANCED_FACE ( 'NONE', ( #768 ), #32796, .T. ) ;
#28327 = CARTESIAN_POINT ( 'NONE',  ( 3.249999999999999556, 0.000000000000000000, 0.000000000000000000 ) ) ;
#28328 = DIRECTION ( 'NONE',  ( 1.000000000000000000, 0.000000000000000000, 0.000000000000000000 ) ) ;
#28329 = VERTEX_POINT ( 'NONE', #13428 ) ;
#28330 = CARTESIAN_POINT ( 'NONE',  ( 3.249999999999999556, -8.152713396088785203, 3.174628368996044170 ) ) ;
#28331 = AXIS2_PLACEMENT_3D ( 'NONE', #8300, #12788, #28039 ) ;
#28332 = CIRCLE ( 'NONE', #12310, 2.999999999999999112 ) ;
#28333 = EDGE_CURVE ( 'NONE', #9245, #773, #28513, .T. ) ;
#28334 = ORIENTED_EDGE ( 'NONE', *, *, #969, .T. ) ;
#28335 = CARTESIAN_POINT ( 'NONE',  ( -15.10000000000019327, -21.93932300455815820, 1.500000000001016520 ) ) ;
#28336 = CALENDAR_DATE ( 2026, 6, 10 ) ;
#28338 = VERTEX_POINT ( 'NONE', #16107 ) ;
#28337 = CARTESIAN_POINT ( 'NONE',  ( -3.370691070153704949, -1.614088942876946264, -1.499999999999999556 ) ) ;
#28340 = EDGE_CURVE ( 'NONE', #21513, #18408, #17482, .T. ) ;
#28339 = ORIENTED_EDGE ( 'NONE', *, *, #5326, .T. ) ;
#28341 = CARTESIAN_POINT ( 'NONE',  ( 17.39502519978889694, -21.04076415203780925, 1.751145182513948351 ) ) ;
#28342 = ORIENTED_EDGE ( 'NONE', *, *, #14349, .F. ) ;
#28343 = CARTESIAN_POINT ( 'NONE',  ( 10.00000000000000178, -8.574039729943018837E-16, 0.000000000000000000 ) ) ;
#28345 = VERTEX_POINT ( 'NONE', #23955 ) ;
#28344 = CARTESIAN_POINT ( 'NONE',  ( 0.7212197813410881064, -8.337493976400217832, -3.259817272377353969 ) ) ;
#28346 = CARTESIAN_POINT ( 'NONE',  ( 85.49734435724781179, -7.913007294147517356, 1.010822989962089746 ) ) ;
#28347 = LINE ( 'NONE', #28686, #3712 ) ;
#28348 = CIRCLE ( 'NONE', #9648, 3.000000000000000444 ) ;
#28349 = ADVANCED_FACE ( 'NONE', ( #11099 ), #21296, .T. ) ;
#28350 = CARTESIAN_POINT ( 'NONE',  ( 0.7632845268448663623, 0.4999240074867329353, -8.734705317657697421 ) ) ;
#28351 = CARTESIAN_POINT ( 'NONE',  ( 17.32050807568873552, 10.00000000000002309, 1.500000000000000000 ) ) ;
#28352 = AXIS2_PLACEMENT_3D ( 'NONE', #1820, #7155, #4491 ) ;
#28353 = AXIS2_PLACEMENT_3D ( 'NONE', #3511, #18534, #23870 ) ;
#28354 = ORIENTED_EDGE ( 'NONE', *, *, #24095, .T. ) ;
#28355 = CIRCLE ( 'NONE', #32641, 5.999999999999999112 ) ;
#28356 =( BOUNDED_SURFACE ( )  B_SPLINE_SURFACE ( 3, 2, ( 
 ( #14929, #32371, #25138 ),
 ( #9430, #30344, #19647 ),
 ( #29841, #14621, #1941 ),
 ( #12114, #19804, #15115 ) ),
 .UNSPECIFIED., .F., .F., .F. ) 
 B_SPLINE_SURFACE_WITH_KNOTS ( ( 4, 4 ),
 ( 3, 3 ),
 ( 0.003792662576232288477, 0.007223425640200679260 ),
 ( 0.000000000000000000, 1.000000000000000000 ),
 .UNSPECIFIED. ) 
 GEOMETRIC_REPRESENTATION_ITEM ( )  RATIONAL_B_SPLINE_SURFACE ( (
 ( 1.000000000000000000, 0.7067603058644416070, 1.000000000000000000),
 ( 1.000000000000000000, 0.7067606020011355517, 1.000000000000000000),
 ( 1.000000000000000000, 0.7067612639882813186, 1.000000000000000000),
 ( 1.000000000000000000, 0.7067623105831687402, 1.000000000000000000) ) ) 
 REPRESENTATION_ITEM ( '' )  SURFACE ( )  );
#28357 = DIRECTION ( 'NONE',  ( 1.000000000000000000, 0.000000000000000000, 0.000000000000000000 ) ) ;
#28358 = DIRECTION ( 'NONE',  ( 0.000000000000000000, 0.000000000000000000, 1.000000000000000000 ) ) ;
#28359 = EDGE_CURVE ( 'NONE', #10070, #18803, #1487, .T. ) ;
#28360 = CARTESIAN_POINT ( 'NONE',  ( -14.85000000000000142, -10.96966150227469328, 4.500000000000000888 ) ) ;
#28361 = DIRECTION ( 'NONE',  ( 0.000000000000000000, 0.000000000000000000, 1.000000000000000000 ) ) ;
#28362 = EDGE_CURVE ( 'NONE', #14707, #29348, #15435, .T. ) ;
#28363 = VECTOR ( 'NONE', #32724, 1000.000000000000000 ) ;
#28364 = CARTESIAN_POINT ( 'NONE',  ( 24.40261005161485386, -17.41690598104249688, 1.428369430449265787 ) ) ;
#28365 = LINE ( 'NONE', #23349, #18258 ) ;
#28366 = CARTESIAN_POINT ( 'NONE',  ( 22.61000000273118715, -1.573300977624594976, 1.942864903642425700 ) ) ;
#28367 = CARTESIAN_POINT ( 'NONE',  ( 7.249760686538667009, -7.135485519861965109, -5.064320921489893657 ) ) ;
#28368 = ORIENTED_EDGE ( 'NONE', *, *, #3036, .T. ) ;
#28369 = CARTESIAN_POINT ( 'NONE',  ( -7.462550801365593678, -3.521866450007987037, -0.3701630799359323931 ) ) ;
#28370 = ORIENTED_EDGE ( 'NONE', *, *, #9278, .F. ) ;
#28371 = EDGE_CURVE ( 'NONE', #32072, #7869, #11746, .T. ) ;
#28372 = CARTESIAN_POINT ( 'NONE',  ( -2.704531657079157103, 2.975847129947406522, 0.3127741368606808403 ) ) ;
#28373 = AXIS2_PLACEMENT_3D ( 'NONE', #1405, #1243, #8274 ) ;
#28374 = CARTESIAN_POINT ( 'NONE',  ( 107.4385791398478744, 17.85938043952739918, 4.629213727441584325 ) ) ;
#28375 = CARTESIAN_POINT ( 'NONE',  ( 3.499999999999999556, -5.349675154362342866, 3.229702268444914370 ) ) ;
#28376 = CARTESIAN_POINT ( 'NONE',  ( 17.02282544784813112, -15.06900748075983998, 1.000000000000000000 ) ) ;
#28377 = ORIENTED_EDGE ( 'NONE', *, *, #25708, .T. ) ;
#28378 = CARTESIAN_POINT ( 'NONE',  ( 40.87556030650695504, -5.373140178142064904, -3.390607986867075763 ) ) ;
#28379 = AXIS2_PLACEMENT_3D ( 'NONE', #8188, #23061, #487 ) ;
#28380 = AXIS2_PLACEMENT_3D ( 'NONE', #32205, #8612, #21659 ) ;
#28381 = CIRCLE ( 'NONE', #8609, 5.000000000000001776 ) ;
#28382 = ORIENTED_EDGE ( 'NONE', *, *, #6090, .T. ) ;
#28383 = CARTESIAN_POINT ( 'NONE',  ( 0.3076689118679163393, 9.439351442243307133, 4.089891983576743328 ) ) ;
#28384 = DATE_AND_TIME ( #31549, #21052 ) ;
#28385 = ADVANCED_FACE ( 'NONE', ( #29664 ), #26980, .T. ) ;
#28386 = CARTESIAN_POINT ( 'NONE',  ( 54.97236717404587836, -6.331065523736658207, 4.185347662761127907 ) ) ;
#28387 = VECTOR ( 'NONE', #3896, 1000.000000000000114 ) ;
#28388 = ADVANCED_FACE ( 'NONE', ( #4420 ), #24803, .T. ) ;
#28389 = AXIS2_PLACEMENT_3D ( 'NONE', #28635, #31464, #23774 ) ;
#28390 = CIRCLE ( 'NONE', #21441, 5.009999999999999787 ) ;
#28391 = CARTESIAN_POINT ( 'NONE',  ( 10.56870887191539587, -4.467071865485462645, -1.625881193364742572 ) ) ;
#28393 = CARTESIAN_POINT ( 'NONE',  ( 5.612718825656740407, 6.420171604529186560, 5.126902779943806721 ) ) ;
#28392 = CARTESIAN_POINT ( 'NONE',  ( 107.3476768466458253, -15.88628154573095586, -1.500000000000000000 ) ) ;
#28394 = ORIENTED_EDGE ( 'NONE', *, *, #28752, .F. ) ;
#28395 = EDGE_CURVE ( 'NONE', #11731, #26820, #8738, .T. ) ;
#28396 = CARTESIAN_POINT ( 'NONE',  ( -50.81000000000000227, -10.96999999999998643, 5.500000000000000000 ) ) ;
#28397 = DIRECTION ( 'NONE',  ( -1.000000000000000000, 8.574039729943018344E-17, 0.000000000000000000 ) ) ;
#28398 = CARTESIAN_POINT ( 'NONE',  ( 3.063284526839887167, -6.772677083992345359, -5.538577986808975062 ) ) ;
#28399 = DIRECTION ( 'NONE',  ( 0.4999999999999918954, 0.8660254037844433705, -0.000000000000000000 ) ) ;
#28401 = EDGE_LOOP ( 'NONE', ( #4531, #20817, #6981, #24279 ) ) ;
#28400 = CARTESIAN_POINT ( 'NONE',  ( 0.8032528114568877609, -4.297275870435987244, 0.9788672205888330202 ) ) ;
#28402 = CARTESIAN_POINT ( 'NONE',  ( -6.512550801365594388, -1.088641768524163389, -3.675193018007246071 ) ) ;
#28403 = AXIS2_PLACEMENT_3D ( 'NONE', #26526, #19003, #29189 ) ;
#28404 = DIRECTION ( 'NONE',  ( 1.000000000000000000, -8.574039729943018344E-17, -0.000000000000000000 ) ) ;
#28405 = CARTESIAN_POINT ( 'NONE',  ( 29.20398424897172873, -7.702373504154283346, -2.184956341310761996 ) ) ;
#28406 = ORIENTED_EDGE ( 'NONE', *, *, #851, .T. ) ;
#28407 = ORIENTED_EDGE ( 'NONE', *, *, #10983, .T. ) ;
#28408 = VECTOR ( 'NONE', #14166, 1000.000000000000000 ) ;
#28410 = EDGE_CURVE ( 'NONE', #2361, #12070, #27427, .T. ) ;
#28409 = CONICAL_SURFACE ( 'NONE', #17730, 299.3348442831094189, 0.4915790642873356098 ) ;
#28412 = CIRCLE ( 'NONE', #25205, 8.750000000000000000 ) ;
#28411 = CARTESIAN_POINT ( 'NONE',  ( 0.000000000000000000, 0.000000000000000000, 0.000000000000000000 ) ) ;
#28413 = LINE ( 'NONE', #8663, #30665 ) ;
#28414 = AXIS2_PLACEMENT_3D ( 'NONE', #17919, #12876, #23408 ) ;
#28415 = CARTESIAN_POINT ( 'NONE',  ( 22.54750000136559507, 1.913930629741522838, -2.363507492473150062 ) ) ;
#28416 = AXIS2_PLACEMENT_3D ( 'NONE', #20996, #26166, #3119 ) ;
#28417 = LINE ( 'NONE', #5529, #4957 ) ;
#28418 = CIRCLE ( 'NONE', #14415, 1.799999999999977174 ) ;
#28419 = FACE_OUTER_BOUND ( 'NONE', #26891, .T. ) ;
#28420 = CARTESIAN_POINT ( 'NONE',  ( -2.794738735352966685, 0.000000000000000000, 1.508259000770582059 ) ) ;
#28421 = CARTESIAN_POINT ( 'NONE',  ( 41.35698357845725326, -8.446179956401751454, 0.8105618903072371317 ) ) ;
#28422 = VERTEX_POINT ( 'NONE', #32178 ) ;
#28423 = CYLINDRICAL_SURFACE ( 'NONE', #1209, 4.000000000000001776 ) ;
#28424 = EDGE_CURVE ( 'NONE', #442, #24619, #27983, .T. ) ;
#28425 = AXIS2_PLACEMENT_3D ( 'NONE', #28549, #2812, #23502 ) ;
#28427 = AXIS2_PLACEMENT_3D ( 'NONE', #4767, #22170, #12458 ) ;
#28426 = DATE_AND_TIME ( #20415, #16187 ) ;
#28428 = EDGE_CURVE ( 'NONE', #16327, #19712, #6267, .T. ) ;
#28429 = DIRECTION ( 'NONE',  ( 0.03487826274237457863, -0.9987827659587181772, 0.03487826274237499496 ) ) ;
#28430 = VECTOR ( 'NONE', #26595, 1000.000000000000000 ) ;
#28431 = ORIENTED_EDGE ( 'NONE', *, *, #26025, .T. ) ;
#28432 = AXIS2_PLACEMENT_3D ( 'NONE', #11909, #4713, #12217 ) ;
#28433 = DIRECTION ( 'NONE',  ( 1.000000000000000000, -0.000000000000000000, -0.000000000000000000 ) ) ;
#28434 = CIRCLE ( 'NONE', #4326, 2.999999999999999112 ) ;
#28435 = ORIENTED_EDGE ( 'NONE', *, *, #7132, .T. ) ;
#28436 = CARTESIAN_POINT ( 'NONE',  ( -17.23085155655856582, 13.48267608780297167, 1.895199557107909438 ) ) ;
#28439 = ORIENTED_EDGE ( 'NONE', *, *, #6176, .F. ) ;
#28438 = VECTOR ( 'NONE', #21444, 1000.000000000000114 ) ;
#28437 = CARTESIAN_POINT ( 'NONE',  ( 69.04182551546352897, -5.543251471596328805, -4.312042181584450518 ) ) ;
#28440 = VERTEX_POINT ( 'NONE', #27129 ) ;
#28441 = CIRCLE ( 'NONE', #2833, 8.500000000000000000 ) ;
#28442 = CYLINDRICAL_SURFACE ( 'NONE', #17647, 10.96966150227469328 ) ;
#28443 = CARTESIAN_POINT ( 'NONE',  ( -7.762550801365593500, 2.228590825266444142, 2.752080473201636845 ) ) ;
#28444 = CARTESIAN_POINT ( 'NONE',  ( 8.571721676197487483, -11.50721971753373118, 1.500000000000000222 ) ) ;
#28445 = VECTOR ( 'NONE', #4018, 1000.000000000000000 ) ;
#28446 = CARTESIAN_POINT ( 'NONE',  ( 23.57316428367446193, -9.051964865574909425, -0.07017451552783579571 ) ) ;
#28448 = VERTEX_POINT ( 'NONE', #1740 ) ;
#28447 = CARTESIAN_POINT ( 'NONE',  ( 22.89656613554824105, 17.95482223816882339, -1.500000000000000222 ) ) ;
#28449 = CARTESIAN_POINT ( 'NONE',  ( -2.143509932485295136E-17, -0.2499999999999467648, -5.003758587302151284 ) ) ;
#28450 = CARTESIAN_POINT ( 'NONE',  ( 22.41270750095310049, 17.13964222901159573, 1.499999999999170441 ) ) ;
#28451 = CARTESIAN_POINT ( 'NONE',  ( 0.2699473030965058307, -15.55366081788063681, 1.500000000000000444 ) ) ;
#28452 = CARTESIAN_POINT ( 'NONE',  ( 21.36000000136559507, 0.9349337715887185984, -3.156283516753368268 ) ) ;
#28453 = DIRECTION ( 'NONE',  ( 1.000000000000000000, -8.574039729943018344E-17, -0.000000000000000000 ) ) ;
#28455 = VERTEX_POINT ( 'NONE', #4229 ) ;
#28454 = CARTESIAN_POINT ( 'NONE',  ( 2.274274201625315683, -4.762163868918371179, 9.915734732513216798 ) ) ;
#28456 = DIRECTION ( 'NONE',  ( -1.000000000000000000, 0.000000000000000000, 0.000000000000000000 ) ) ;
#28457 = EDGE_CURVE ( 'NONE', #13484, #9295, #27431, .T. ) ;
#28458 = CC_DESIGN_PERSON_AND_ORGANIZATION_ASSIGNMENT ( #15540, #13050, ( #4466 ) ) ;
#28459 = VECTOR ( 'NONE', #21354, 1000.000000000000000 ) ;
#28460 = AXIS2_PLACEMENT_3D ( 'NONE', #20582, #13045, #3032 ) ;
#28461 = DIRECTION ( 'NONE',  ( 1.000000000000000000, 6.288372600415920195E-15, 0.000000000000000000 ) ) ;
#28462 = CARTESIAN_POINT ( 'NONE',  ( 21.98500000136559507, -2.892927487894331406, 1.570731468192932301 ) ) ;
#28463 = AXIS2_PLACEMENT_3D ( 'NONE', #28018, #5114, #15291 ) ;
#28464 = CIRCLE ( 'NONE', #20449, 3.000000000000000000 ) ;
#28465 = DIRECTION ( 'NONE',  ( -0.03488359650710489562, -0.9989355049964837585, 0.03018263660036206442 ) ) ;
#28466 = AXIS2_PLACEMENT_3D ( 'NONE', #28944, #1524, #19425 ) ;
#28467 = CARTESIAN_POINT ( 'NONE',  ( 6.037141869538510619, 7.104659103919411578, -4.619542287584830653 ) ) ;
#28468 = CARTESIAN_POINT ( 'NONE',  ( -2.745055912661924058, -0.1926413909297530480, -1.404235515124709455 ) ) ;
#28469 = ORIENTED_EDGE ( 'NONE', *, *, #10496, .F. ) ;
#28470 = CARTESIAN_POINT ( 'NONE',  ( 3.063284526839887167, -0.4999240074895051067, 8.734705317681624948 ) ) ;
#28471 = CARTESIAN_POINT ( 'NONE',  ( -48.07500000000000284, -10.96966150227468972, 7.500000000000000000 ) ) ;
#28472 = ORIENTED_EDGE ( 'NONE', *, *, #3865, .F. ) ;
#28473 = EDGE_CURVE ( 'NONE', #15697, #7137, #31199, .T. ) ;
#28474 = DIRECTION ( 'NONE',  ( -1.000000000000000000, -0.000000000000000000, -0.000000000000000000 ) ) ;
#28475 = ADVANCED_FACE ( 'NONE', ( #32502, #9561 ), #29986, .F. ) ;
#28476 = CYLINDRICAL_SURFACE ( 'NONE', #11733, 0.5000000000000004441 ) ;
#28477 = CARTESIAN_POINT ( 'NONE',  ( 0.9306419922191571104, -8.901511148765195003, -0.9788672205888330202 ) ) ;
#28479 = CARTESIAN_POINT ( 'NONE',  ( 107.4707837513502255, -17.66103516835562459, 4.957671652933026252 ) ) ;
#28478 = DIRECTION ( 'NONE',  ( -0.08910563629484158366, -0.9960221812693186294, 0.000000000000000000 ) ) ;
#28480 = VERTEX_POINT ( 'NONE', #13911 ) ;
#28481 = AXIS2_PLACEMENT_3D ( 'NONE', #1093, #1280, #11461 ) ;
#28482 = CARTESIAN_POINT ( 'NONE',  ( -41.86373177837820236, -16.13513036599589867, 5.128141679950118714 ) ) ;
#28483 = ORIENTED_EDGE ( 'NONE', *, *, #3504, .F. ) ;
#28484 = FACE_OUTER_BOUND ( 'NONE', #27312, .T. ) ;
#28485 = CIRCLE ( 'NONE', #7116, 4.000000000000001776 ) ;
#28487 = ORIENTED_EDGE ( 'NONE', *, *, #29112, .T. ) ;
#28486 = CARTESIAN_POINT ( 'NONE',  ( 3.499999999999999556, 4.438567988583082879, 7.249076783337693008 ) ) ;
#28488 = VERTEX_POINT ( 'NONE', #31839 ) ;
#28489 = DIRECTION ( 'NONE',  ( -7.770718973608921957E-17, -0.9063077870366440525, -0.4226182617407121533 ) ) ;
#28490 = VECTOR ( 'NONE', #26633, 1000.000000000000114 ) ;
#28491 = CIRCLE ( 'NONE', #6591, 6.999999999999998224 ) ;
#28492 = CIRCLE ( 'NONE', #14046, 0.5000000000000000000 ) ;
#28493 = DIRECTION ( 'NONE',  ( 1.000000000000000000, -0.000000000000000000, -0.000000000000000000 ) ) ;
#28495 = ORIENTED_EDGE ( 'NONE', *, *, #10100, .F. ) ;
#28494 = CARTESIAN_POINT ( 'NONE',  ( 107.7704433617907398, 16.89989798460841541, 1.595839734757286577 ) ) ;
#28496 = VERTEX_POINT ( 'NONE', #8909 ) ;
#28497 = CARTESIAN_POINT ( 'NONE',  ( -56.34260592272676149, 0.003888339313515875358, -1.002939418600732768 ) ) ;
#28498 = CARTESIAN_POINT ( 'NONE',  ( 18.74163570027171843, -6.065217073546690152, 3.693462925058700552 ) ) ;
#28499 = CC_DESIGN_APPROVAL ( #16568, ( #5017 ) ) ;
#28500 = CARTESIAN_POINT ( 'NONE',  ( 1.394036994807660394E-16, 1.625881193364758337, -4.467071865485455540 ) ) ;
#28501 = DIRECTION ( 'NONE',  ( -4.917867153432989168E-17, -0.5735764363510442720, -0.8191520442889931308 ) ) ;
#28502 = CARTESIAN_POINT ( 'NONE',  ( 2.274274201620947622, 4.762163868927166810, 9.915734732518528105 ) ) ;
#28503 = CARTESIAN_POINT ( 'NONE',  ( -83.35439080561378944, -0.0003384977252891612984, 0.000000000000000000 ) ) ;
#28504 = LINE ( 'NONE', #28802, #3313 ) ;
#28505 = CARTESIAN_POINT ( 'NONE',  ( 35.28555349212377479, -7.422113525903523801, 2.787782628857160105 ) ) ;
#28506 = CARTESIAN_POINT ( 'NONE',  ( 0.7632845268398876781, -0.4999240074893807617, -8.734705317681624948 ) ) ;
#28507 = CARTESIAN_POINT ( 'NONE',  ( 3.750263394063812150, -2.684783474401000736E-05, 0.9948185799301203502 ) ) ;
#28508 = AXIS2_PLACEMENT_3D ( 'NONE', #6420, #29025, #29516 ) ;
#28509 = ORIENTED_EDGE ( 'NONE', *, *, #28088, .F. ) ;
#28510 = AXIS2_PLACEMENT_3D ( 'NONE', #25007, #7958, #2800 ) ;
#28511 = CARTESIAN_POINT ( 'NONE',  ( 7.249760686538667009, 3.647351267791570262, 7.953573330858228374 ) ) ;
#28512 = APPLICATION_CONTEXT ( 'configuration controlled 3d designs of mechanical parts and assemblies' ) ;
#28513 = CIRCLE ( 'NONE', #30126, 6.818740222761507042 ) ;
#28514 = CARTESIAN_POINT ( 'NONE',  ( 29.35001421184127324, -4.582605737176274729, 4.522129901861162260 ) ) ;
#28515 = EDGE_CURVE ( 'NONE', #32366, #8466, #20914, .T. ) ;
#28516 = DIRECTION ( 'NONE',  ( 0.000000000000000000, 0.000000000000000000, -1.000000000000000000 ) ) ;
#28517 = ORIENTED_EDGE ( 'NONE', *, *, #25497, .F. ) ;
#28518 = AXIS2_PLACEMENT_3D ( 'NONE', #1789, #20162, #7429 ) ;
#28519 = ADVANCED_FACE ( 'NONE', ( #27980 ), #22942, .T. ) ;
#28520 = CARTESIAN_POINT ( 'NONE',  ( 2.382865613620175349, 0.000000000000000000, 1.508259000770581615 ) ) ;
#28521 = CARTESIAN_POINT ( 'NONE',  ( 17.39502519979085449, -21.04076415203812189, -1.751145182513949239 ) ) ;
#28522 = CC_DESIGN_SECURITY_CLASSIFICATION ( #10350, ( #1293 ) ) ;
#28523 = ORIENTED_EDGE ( 'NONE', *, *, #9947, .T. ) ;
#28524 = FACE_OUTER_BOUND ( 'NONE', #8335, .T. ) ;
#28525 =( NAMED_UNIT ( * ) SI_UNIT ( $, .STERADIAN. ) SOLID_ANGLE_UNIT ( ) );
#28526 = ORIENTED_EDGE ( 'NONE', *, *, #17101, .F. ) ;
#28527 = LINE ( 'NONE', #10958, #29488 ) ;
#28528 = DATE_AND_TIME ( #18806, #17317 ) ;
#28530 = ORIENTED_EDGE ( 'NONE', *, *, #14567, .F. ) ;
#28529 = CARTESIAN_POINT ( 'NONE',  ( 23.11000000000000298, 1.942864903642424146, 1.573300977624592534 ) ) ;
#28531 = ORIENTED_EDGE ( 'NONE', *, *, #18077, .T. ) ;
#28532 = CARTESIAN_POINT ( 'NONE',  ( -2.373270979209490594, -12.30283429957249552, 1.743844681977045452 ) ) ;
#28533 = ORIENTED_EDGE ( 'NONE', *, *, #7015, .F. ) ;
#28534 = CARTESIAN_POINT ( 'NONE',  ( 3.148734258548781612E-16, 3.672404558090038851, 3.407865132560194077 ) ) ;
#28535 = CIRCLE ( 'NONE', #16226, 5.587650971692158741 ) ;
#28537 = ORIENTED_EDGE ( 'NONE', *, *, #11511, .F. ) ;
#28536 = CARTESIAN_POINT ( 'NONE',  ( 0.5640492184727915470, -8.844377740319856684, -3.576105523038093814 ) ) ;
#28538 = CARTESIAN_POINT ( 'NONE',  ( 0.3076690219785678804, 6.806638167507736092, -7.713510465966239238 ) ) ;
#28539 = DIRECTION ( 'NONE',  ( 0.000000000000000000, 0.000000000000000000, -1.000000000000000000 ) ) ;
#28540 = LINE ( 'NONE', #31522, #30678 ) ;
#28541 = DIRECTION ( 'NONE',  ( -1.000000000000000000, 0.000000000000000000, 0.000000000000000000 ) ) ;
#28542 = ORIENTED_EDGE ( 'NONE', *, *, #21231, .T. ) ;
#28543 = DIRECTION ( 'NONE',  ( 0.5649695393302035518, 0.8251117619019968652, -0.000000000000000000 ) ) ;
#28544 = DIRECTION ( 'NONE',  ( -1.000000000000000000, 0.000000000000000000, -0.000000000000000000 ) ) ;
#28545 = DIRECTION ( 'NONE',  ( 0.9842544651762054064, -0.1767573132311699713, 0.000000000000000000 ) ) ;
#28546 = CARTESIAN_POINT ( 'NONE',  ( 0.7632845268398883443, -7.360373001730875053, -4.729683950898950329 ) ) ;
#28547 = CC_DESIGN_SECURITY_CLASSIFICATION ( #21588, ( #33100 ) ) ;
#28548 = EDGE_CURVE ( 'NONE', #10880, #22618, #30680, .T. ) ;
#28549 = CARTESIAN_POINT ( 'NONE',  ( 4.749760686538667009, 2.741043480755029016, -7.530955069117485579 ) ) ;
#28550 = CARTESIAN_POINT ( 'NONE',  ( 56.97280603064898941, -277.2763395528616002, 0.4463807625373211185 ) ) ;
#28551 = FACE_BOUND ( 'NONE', #11036, .T. ) ;
#28552 = LINE ( 'NONE', #5794, #12936 ) ;
#28553 = CARTESIAN_POINT ( 'NONE',  ( -7.700050802731188249, 1.549418761218566143, -2.853674364686379583 ) ) ;
#28554 = ORIENTED_EDGE ( 'NONE', *, *, #11475, .T. ) ;
#28555 = CARTESIAN_POINT ( 'NONE',  ( -4.054531657079157192, -1.545410377633946286, 2.846291840500174697 ) ) ;
#28556 = AXIS2_PLACEMENT_3D ( 'NONE', #11466, #14275, #4259 ) ;
#28557 = EDGE_CURVE ( 'NONE', #28881, #11175, #20627, .T. ) ;
#28558 = CARTESIAN_POINT ( 'NONE',  ( 107.9095624609269777, -17.54879161072074112, 4.428303208956443804 ) ) ;
#28559 = DIRECTION ( 'NONE',  ( -1.000000000000000000, 0.000000000000000000, 0.000000000000000000 ) ) ;
#28560 = CARTESIAN_POINT ( 'NONE',  ( 23.15368348411500676, -16.86203458189232762, 1.500000000000277778 ) ) ;
#28561 = EDGE_LOOP ( 'NONE', ( #13096, #14700, #18244, #6596 ) ) ;
#28562 = DIRECTION ( 'NONE',  ( -1.000000000000000000, 0.000000000000000000, 0.000000000000000000 ) ) ;
#28563 = ORIENTED_EDGE ( 'NONE', *, *, #21914, .T. ) ;
#28564 = DIRECTION ( 'NONE',  ( 0.8247831655431905329, -0.5654491399202531410, 0.000000000000000000 ) ) ;
#28565 = CALENDAR_DATE ( 2026, 6, 10 ) ;
#28566 = EDGE_CURVE ( 'NONE', #15394, #15974, #27792, .T. ) ;
#28567 = CARTESIAN_POINT ( 'NONE',  ( 69.05921145838347286, -5.891398902068986310, 4.215290682806994482 ) ) ;
#28568 = DIRECTION ( 'NONE',  ( 7.472768010110236499E-18, 0.08715574274764813223, 0.9961946980917464334 ) ) ;
#28570 = DIRECTION ( 'NONE',  ( -1.000000000000000000, 0.000000000000000000, -0.000000000000000000 ) ) ;
#28569 = CARTESIAN_POINT ( 'NONE',  ( 10.90258948330155953, 17.51112508050605854, 4.629213727441584325 ) ) ;
#28571 = ORIENTED_EDGE ( 'NONE', *, *, #26498, .T. ) ;
#28572 = EDGE_CURVE ( 'NONE', #24916, #21064, #763, .T. ) ;
#28573 = DIRECTION ( 'NONE',  ( 0.000000000000000000, 0.000000000000000000, 1.000000000000000000 ) ) ;
#28574 = DIRECTION ( 'NONE',  ( 0.000000000000000000, -0.000000000000000000, -1.000000000000000000 ) ) ;
#28575 = CARTESIAN_POINT ( 'NONE',  ( 22.23500000136559862, -3.156283516753370044, -0.9349337715887220401 ) ) ;
#28577 = ORIENTED_EDGE ( 'NONE', *, *, #8760, .F. ) ;
#28576 = CARTESIAN_POINT ( 'NONE',  ( 108.2286012845016074, 19.45110207874543917, -3.054862429917418520 ) ) ;
#28578 = CARTESIAN_POINT ( 'NONE',  ( -5.512550801365595277, 3.675193018007247403, -1.088641768524161391 ) ) ;
#28579 = EDGE_CURVE ( 'NONE', #9295, #1225, #7700, .T. ) ;
#28580 = DIRECTION ( 'NONE',  ( -1.000000000000000000, -0.000000000000000000, -0.000000000000000000 ) ) ;
#28581 = CARTESIAN_POINT ( 'NONE',  ( 35.29143477761605396, -7.046680052073756251, -3.390608481277731734 ) ) ;
#28582 = ORIENTED_EDGE ( 'NONE', *, *, #20160, .F. ) ;
#28583 = VERTEX_POINT ( 'NONE', #9746 ) ;
#28584 = CARTESIAN_POINT ( 'NONE',  ( 24.29160796521618337, -17.33532173511207830, -1.337584091082468118 ) ) ;
#28585 = DIRECTION ( 'NONE',  ( 0.000000000000000000, -0.9961946980917461003, 0.08715574274765118534 ) ) ;
#28586 = CLOSED_SHELL ( 'NONE', ( #18220, #22225, #26750, #21740, #21666, #30072, #13222, #32112, #13140, #24675, #18166, #30590, #8028, #4637, #9796, #13288, #20909, #1707, #19477, #16059, #19951, #7418, #19784, #21623, #30512, #3551, #27543, #26439, #1, #7253, #1685, #3531, #6269, #2444, #30644, #16014, #985, #31795, #8554, #20194, #28519, #12819, #2218, #17373, #27729, #12231, #23443, #13857, #20737, #31827, #30683, #6720, #15258, #8944, #11463, #30429, #4156, #19205, #26473, #9920, #17987, #9889, #22367, #15089, #19430, #884, #31028, #30482, #27323, #24618, #16335, #14905, #33052, #26411, #26217, #27996, #32543, #1869, #11937, #6881, #28770, #18634, #26088, #7856, #22128, #23468, #32013, #27658, #18998, #2328, #20994, #3068, #18671, #3445, #27086, #30357, #15149, #10159, #24192, #9688, #14715, #19284, #18179, #17995, #17648, #29928, #22444, #13237, #6611, #30156, #13834, #32019, #19438 ) ) ;
#28587 = EDGE_CURVE ( 'NONE', #24201, #1536, #19014, .T. ) ;
#28588 = EDGE_CURVE ( 'NONE', #22005, #6622, #12241, .T. ) ;
#28589 = CARTESIAN_POINT ( 'NONE',  ( 3.249999999999999556, 9.241976615262160522, -1.699438267350404930 ) ) ;
#28590 = CARTESIAN_POINT ( 'NONE',  ( 2.864530965498453430, 2.320611941139924195, 9.276519854389871256 ) ) ;
#28591 = DIRECTION ( 'NONE',  ( 7.472768010111415168E-18, 0.08715574274766135776, -0.9961946980917453232 ) ) ;
#28592 = CARTESIAN_POINT ( 'NONE',  ( 2.632061376486628301, -0.5000000000000000000, -1.500000000000000000 ) ) ;
#28593 = CARTESIAN_POINT ( 'NONE',  ( 35.27024661284173845, -8.402227462205928532, 0.07017451552782133506 ) ) ;
#28594 = ORIENTED_EDGE ( 'NONE', *, *, #2324, .F. ) ;
#28595 = CARTESIAN_POINT ( 'NONE',  ( 2.592584839945472730, -8.898511132913942134, -5.238191131136724188 ) ) ;
#28596 = ORIENTED_EDGE ( 'NONE', *, *, #28579, .F. ) ;
#28597 = APPROVAL_STATUS ( 'not_yet_approved' ) ;
#28598 = CARTESIAN_POINT ( 'NONE',  ( 4.749760686538667009, -4.007137495034861274, 6.940565734314584567 ) ) ;
#28599 = ORIENTED_EDGE ( 'NONE', *, *, #30430, .F. ) ;
#28600 = EDGE_CURVE ( 'NONE', #22010, #19432, #17946, .T. ) ;
#28601 = DIRECTION ( 'NONE',  ( 0.000000000000000000, 0.000000000000000000, -1.000000000000000000 ) ) ;
#28602 = ORIENTED_EDGE ( 'NONE', *, *, #18621, .F. ) ;
#28603 = CARTESIAN_POINT ( 'NONE',  ( 0.5704035821694232178, -9.519055809314989958, 0.6538686328478395815 ) ) ;
#28605 = ORIENTED_EDGE ( 'NONE', *, *, #4060, .F. ) ;
#28604 = CARTESIAN_POINT ( 'NONE',  ( 54.94911284525054640, -5.490851268031983423, -4.150065907156753831 ) ) ;
#28606 = ORIENTED_EDGE ( 'NONE', *, *, #6127, .T. ) ;
#28607 = CARTESIAN_POINT ( 'NONE',  ( -15.02135460118491217, -21.93013659628234890, 1.095404497688272638 ) ) ;
#28608 = CARTESIAN_POINT ( 'NONE',  ( -4.512550801365592612, 1.088641768524161613, 3.675193018007246959 ) ) ;
#28609 = CARTESIAN_POINT ( 'NONE',  ( 6.910673634762098061, -8.774004714863517407, 1.499999999999999778 ) ) ;
#28610 = CARTESIAN_POINT ( 'NONE',  ( 48.09235817783085309, -9.172289267036324745, -1.915219082070897638 ) ) ;
#28612 = ORIENTED_EDGE ( 'NONE', *, *, #21033, .T. ) ;
#28611 = DIRECTION ( 'NONE',  ( -0.000000000000000000, -0.3746065934159164001, 0.9271838545667856479 ) ) ;
#28613 = CARTESIAN_POINT ( 'NONE',  ( -55.91000000000000369, -10.96999999999998643, 5.700000000000000178 ) ) ;
#28614 = CARTESIAN_POINT ( 'NONE',  ( 17.92222975120050776, 13.44085466220149172, 1.050000000000000044 ) ) ;
#28615 = CARTESIAN_POINT ( 'NONE',  ( -1.201782691452277785, -13.92888619398943639, 1.500000000000158984 ) ) ;
#28616 = FACE_OUTER_BOUND ( 'NONE', #29363, .T. ) ;
#28617 = LINE ( 'NONE', #25781, #10138 ) ;
#28618 = ADVANCED_FACE ( 'NONE', ( #15088 ), #20280, .F. ) ;
#28620 = VERTEX_POINT ( 'NONE', #2416 ) ;
#28619 = CARTESIAN_POINT ( 'NONE',  ( 2.976845773540285567, -3.349682859779558264, 8.532418605434719083 ) ) ;
#28621 = DIRECTION ( 'NONE',  ( 0.000000000000000000, 0.5735764363510594821, -0.8191520442889824727 ) ) ;
#28622 = CARTESIAN_POINT ( 'NONE',  ( 107.3477133433398336, -15.88627905081428615, 1.500000000000000000 ) ) ;
#28623 = CARTESIAN_POINT ( 'NONE',  ( 21.67250000136559507, 2.363507492473148286, 1.913930629741525058 ) ) ;
#28624 = EDGE_CURVE ( 'NONE', #9705, #5581, #10894, .T. ) ;
#28625 = ADVANCED_FACE ( 'NONE', ( #10241, #14908 ), #32666, .F. ) ;
#28626 = CARTESIAN_POINT ( 'NONE',  ( -22.70948346437429066, 4.195786794270493836, 1.500000000001212808 ) ) ;
#28627 = CARTESIAN_POINT ( 'NONE',  ( 46.92593983402662872, 24.78664516185572353, 5.412820279296878923 ) ) ;
#28628 = CARTESIAN_POINT ( 'NONE',  ( -2.626726202933311161, 0.09953226261466606439, -1.366272513173331982 ) ) ;
#28629 = DIRECTION ( 'NONE',  ( 0.8660254037844424824, -0.4999999999999933942, 0.000000000000000000 ) ) ;
#28630 = CARTESIAN_POINT ( 'NONE',  ( -28.85000000000000497, -10.96966150227469505, 4.500000000000000888 ) ) ;
#28631 = EDGE_LOOP ( 'NONE', ( #11385, #17213, #8951, #8469 ) ) ;
#28632 = CARTESIAN_POINT ( 'NONE',  ( -5.750050799999999462, 0.000000000000000000, -6.000000000000001776 ) ) ;
#28633 = DIRECTION ( 'NONE',  ( -7.472768010110877448E-18, -0.08715574274765462703, -0.9961946980917457672 ) ) ;
#28634 = LINE ( 'NONE', #22791, #22088 ) ;
#28636 = CARTESIAN_POINT ( 'NONE',  ( 107.9805524956831846, -17.78932289238704811, 4.337499095951103278 ) ) ;
#28635 = CARTESIAN_POINT ( 'NONE',  ( 0.000000000000000000, 18.00000000000000355, 0.000000000000000000 ) ) ;
#28637 = ORIENTED_EDGE ( 'NONE', *, *, #15867, .F. ) ;
#28638 = ADVANCED_FACE ( 'NONE', ( #7570 ), #12420, .T. ) ;
#28639 = APPROVAL ( #4281, 'UNSPECIFIED' ) ;
#28640 = DIRECTION ( 'NONE',  ( -0.000000000000000000, -0.000000000000000000, -1.000000000000000000 ) ) ;
#28641 = ORIENTED_EDGE ( 'NONE', *, *, #9776, .T. ) ;
#28642 = CYLINDRICAL_SURFACE ( 'NONE', #19347, 0.5000000000000004441 ) ;
#28644 = EDGE_LOOP ( 'NONE', ( #20728, #10826, #29261, #897 ) ) ;
#28643 = DIRECTION ( 'NONE',  ( -1.000000000000000000, 0.000000000000000000, 0.000000000000000000 ) ) ;
#28645 = ORIENTED_EDGE ( 'NONE', *, *, #10429, .F. ) ;
#28646 = DIRECTION ( 'NONE',  ( -1.000000000000000000, -0.000000000000000000, -0.000000000000000000 ) ) ;
#28647 = CARTESIAN_POINT ( 'NONE',  ( 7.249760686538667009, 0.000000000000000000, 0.000000000000000000 ) ) ;
#28649 = ORIENTED_EDGE ( 'NONE', *, *, #20856, .F. ) ;
#28648 = FACE_OUTER_BOUND ( 'NONE', #31297, .T. ) ;
#28650 = ORIENTED_EDGE ( 'NONE', *, *, #22060, .T. ) ;
#28651 = DIRECTION ( 'NONE',  ( 1.000000000000000000, -8.574039729943018344E-17, -0.000000000000000000 ) ) ;
#28652 = CARTESIAN_POINT ( 'NONE',  ( 21.34414429286656656, -21.72097900651801083, -1.443623072030687515 ) ) ;
#28653 = CARTESIAN_POINT ( 'NONE',  ( 23.01404055077311028, -17.34213939868426735, -1.500000000000000666 ) ) ;
#28654 = CARTESIAN_POINT ( 'NONE',  ( -2.492109178653469037, -0.3150232093026757996, 2.997245624844496081 ) ) ;
#28655 = LINE ( 'NONE', #30856, #8193 ) ;
#28656 = ADVANCED_FACE ( 'NONE', ( #17770 ), #23128, .T. ) ;
#28657 = DIRECTION ( 'NONE',  ( -1.000000000000000000, 0.000000000000000000, -0.000000000000000000 ) ) ;
#28658 = FACE_OUTER_BOUND ( 'NONE', #14219, .T. ) ;
#28659 = DIRECTION ( 'NONE',  ( -1.000000000000000000, 0.000000000000000000, 0.000000000000000000 ) ) ;
#28660 = CARTESIAN_POINT ( 'NONE',  ( -3.200050800000000528, -2.331437884370912705, 1.887961173149512062 ) ) ;
#28661 = CARTESIAN_POINT ( 'NONE',  ( 3.048228882235579196, 0.5389963249801693612, 1.289664751349846261 ) ) ;
#28662 = EDGE_LOOP ( 'NONE', ( #26808, #32723, #27976, #30402 ) ) ;
#28663 = CARTESIAN_POINT ( 'NONE',  ( 6.883866621640341243, -6.123537914202284327, 6.224335161394995986 ) ) ;
#28664 = CARTESIAN_POINT ( 'NONE',  ( 23.80135741154357731, -5.059951201419131017, 5.695980980372492120 ) ) ;
#28665 = DIRECTION ( 'NONE',  ( 0.000000000000000000, 0.2588190451025100813, 0.9659258262890711988 ) ) ;
#28666 = EDGE_LOOP ( 'NONE', ( #1791, #26694, #2858, #3669 ) ) ;
#28667 = CARTESIAN_POINT ( 'NONE',  ( 23.86000000136559507, 1.570731468192929858, 2.892927487894329186 ) ) ;
#28668 = CARTESIAN_POINT ( 'NONE',  ( 25.49905227492783766, -1.632004223636194684, -2.257790968203141624 ) ) ;
#28669 = DIRECTION ( 'NONE',  ( 0.000000000000000000, 1.000000000000000000, 0.000000000000000000 ) ) ;
#28670 = ORIENTED_EDGE ( 'NONE', *, *, #27738, .T. ) ;
#28671 = DIRECTION ( 'NONE',  ( -1.000000000000000000, -0.000000000000000000, -0.000000000000000000 ) ) ;
#28672 = SHAPE_REPRESENTATION_RELATIONSHIP ( 'NONE' , 'NONE' ,  #6656, #2414 ) ;
#28673 = EDGE_CURVE ( 'NONE', #30996, #6099, #24545, .T. ) ;
#28674 = EDGE_LOOP ( 'NONE', ( #22452, #28743, #8774, #22801 ) ) ;
#28675 = CARTESIAN_POINT ( 'NONE',  ( 19.10390797508228999, -2.015740111943971957, -1.010822989962086416 ) ) ;
#28676 = ITEM_DEFINED_TRANSFORMATION ( 'NONE', 'NONE', #25262,  #2865 ) ;
#28678 = ORIENTED_EDGE ( 'NONE', *, *, #10582, .F. ) ;
#28677 = LINE ( 'NONE', #8592, #29888 ) ;
#28679 = VERTEX_POINT ( 'NONE', #539 ) ;
#28680 = CARTESIAN_POINT ( 'NONE',  ( 24.61000000136559152, 3.156283516753366047, 0.9349337715887203748 ) ) ;
#28681 = ORIENTED_EDGE ( 'NONE', *, *, #26966, .T. ) ;
#28682 = CARTESIAN_POINT ( 'NONE',  ( -7.550050800000000173, 3.113457007523260156, -0.9222479816126439855 ) ) ;
#28684 = ORIENTED_EDGE ( 'NONE', *, *, #26910, .T. ) ;
#28683 = CARTESIAN_POINT ( 'NONE',  ( 54.90142980600692368, -3.782945109527315442, -1.169950777188108137 ) ) ;
#28685 = CARTESIAN_POINT ( 'NONE',  ( 10.49279877231860425, 2.037595134782375084, 1.050000000000000266 ) ) ;
#28686 = CARTESIAN_POINT ( 'NONE',  ( 10.00000000000000000, 0.8254815157535864145, -4.681538312723508177 ) ) ;
#28687 = EDGE_CURVE ( 'NONE', #15557, #11002, #8059, .T. ) ;
#28688 = DIRECTION ( 'NONE',  ( 0.000000000000000000, 0.000000000000000000, -1.000000000000000000 ) ) ;
#28689 = DIRECTION ( 'NONE',  ( -0.000000000000000000, -0.000000000000000000, 1.000000000000000000 ) ) ;
#28690 = EDGE_CURVE ( 'NONE', #19221, #7973, #26163, .T. ) ;
#28691 = EDGE_LOOP ( 'NONE', ( #25762, #13181, #1976, #32037 ) ) ;
#28692 = B_SPLINE_CURVE_WITH_KNOTS ( 'NONE', 3,
 ( #18210, #22899, #15718, #26073, #25419, #349, #15862, #670 ),
 .UNSPECIFIED., .F., .F.,
 ( 4, 2, 2, 4 ),
 ( 0.009544196576262381146, 0.5047720982881314100, 0.7523860491440657050, 1.000000000000000000 ),
 .UNSPECIFIED. ) ;
#28693 = EDGE_CURVE ( 'NONE', #29863, #5623, #13036, .T. ) ;
#28694 = CARTESIAN_POINT ( 'NONE',  ( 10.55147673363119232, 4.116875700062115229, -2.376879293651021019 ) ) ;
#28695 = DIRECTION ( 'NONE',  ( -0.08343273266574513514, -0.4645863764670032925, -0.8815886103626715542 ) ) ;
#28696 = CARTESIAN_POINT ( 'NONE',  ( 29.19213769712790096, -8.050053894908174357, -1.529339505921241349 ) ) ;
#28697 = CARTESIAN_POINT ( 'NONE',  ( 13.62547635268498780, 21.94000000000002970, -1.500000000000000000 ) ) ;
#28698 = CARTESIAN_POINT ( 'NONE',  ( 24.39957246288403070, -17.41407024517256730, 1.423208249768635358 ) ) ;
#28699 = CARTESIAN_POINT ( 'NONE',  ( 10.00000000000000178, -4.458382051008212166, 2.285372942704935628 ) ) ;
#28700 = DIRECTION ( 'NONE',  ( 0.000000000000000000, 0.000000000000000000, 1.000000000000000000 ) ) ;
#28701 = DIRECTION ( 'NONE',  ( 0.7222222222222246524, 0.000000000000000000, -0.6916610887771492688 ) ) ;
#28702 = CARTESIAN_POINT ( 'NONE',  ( 84.94207106226072312, -3.684213880880722769, 3.390607676399204795 ) ) ;
#28703 = CARTESIAN_POINT ( 'NONE',  ( -3.562550801365592879, -2.752080473201636845, 2.228590825266444586 ) ) ;
#28704 = ORIENTED_EDGE ( 'NONE', *, *, #31745, .F. ) ;
#28705 = CARTESIAN_POINT ( 'NONE',  ( -2.754531657079157814, 3.105402419394639235, -0.9198621039125850496 ) ) ;
#28706 = PLANE ( 'NONE',  #14580 ) ;
#28707 = DIRECTION ( 'NONE',  ( -0.000000000000000000, -0.9993908270190956511, -0.03489949670250104552 ) ) ;
#28708 = CARTESIAN_POINT ( 'NONE',  ( 9.126991455998574310, -11.32614230997930882, 1.499999999999998668 ) ) ;
#28709 = ORIENTED_EDGE ( 'NONE', *, *, #3904, .T. ) ;
#28710 = CARTESIAN_POINT ( 'NONE',  ( 68.97545755171863391, -4.219822329608945211, -2.787783122615425935 ) ) ;
#28711 = ORIENTED_EDGE ( 'NONE', *, *, #10745, .T. ) ;
#28712 = CARTESIAN_POINT ( 'NONE',  ( 0.8185896255502229657, -4.595692320205778891, 1.500000000000000000 ) ) ;
#28713 = PERSON_AND_ORGANIZATION_ROLE ( 'creator' ) ;
#28714 = CARTESIAN_POINT ( 'NONE',  ( 18.77836082091593894, -5.654703931404403860, 4.215290389441141095 ) ) ;
#28715 = EDGE_CURVE ( 'NONE', #1346, #4533, #21775, .T. ) ;
#28716 = DIRECTION ( 'NONE',  ( 0.7222222222222212107, 1.305870959400644667E-15, -0.6916610887771528215 ) ) ;
#28717 = CARTESIAN_POINT ( 'NONE',  ( 56.97280603064898941, -277.2763395528616002, 0.4463807625373084065 ) ) ;
#28718 = ORIENTED_EDGE ( 'NONE', *, *, #28166, .F. ) ;
#28719 = CARTESIAN_POINT ( 'NONE',  ( 6.037141812302424526, -8.256172215043587670, 1.911013226338381221 ) ) ;
#28720 = CARTESIAN_POINT ( 'NONE',  ( 26.05758037654617354, 19.05414323982526525, -1.152255141331423705 ) ) ;
#28721 = CARTESIAN_POINT ( 'NONE',  ( 56.97280603064898941, -277.2763395528616002, 0.000000000000000000 ) ) ;
#28723 = ORIENTED_EDGE ( 'NONE', *, *, #29209, .F. ) ;
#28722 = CYLINDRICAL_SURFACE ( 'NONE', #3237, 4.000000000000001776 ) ;
#28724 = CARTESIAN_POINT ( 'NONE',  ( -2.512550801365593056, -1.088641768524163389, -3.675193018007246071 ) ) ;
#28725 = CARTESIAN_POINT ( 'NONE',  ( 12.44989959798878587, 19.50000000000000000, 1.818740222761551451 ) ) ;
#28726 = DIRECTION ( 'NONE',  ( -1.000000000000000000, -0.000000000000000000, 0.000000000000000000 ) ) ;
#28727 = VERTEX_POINT ( 'NONE', #21263 ) ;
#28728 = ORIENTED_EDGE ( 'NONE', *, *, #1288, .F. ) ;
#28729 = CARTESIAN_POINT ( 'NONE',  ( -2.249956573341760357, 1.323625320507108460, 3.284597389080124774 ) ) ;
#28730 = DIRECTION ( 'NONE',  ( -0.1437473352844943209, 0.000000000000000000, 0.9896144216807913896 ) ) ;
#28731 = VERTEX_POINT ( 'NONE', #23289 ) ;
#28732 = DIRECTION ( 'NONE',  ( 1.000000000000000000, -0.000000000000000000, -0.000000000000000000 ) ) ;
#28733 = DIRECTION ( 'NONE',  ( -4.917867153432990401E-17, -0.5735764363510447161, -0.8191520442889927978 ) ) ;
#28734 = FACE_OUTER_BOUND ( 'NONE', #19771, .T. ) ;
#28735 = B_SPLINE_CURVE_WITH_KNOTS ( 'NONE', 3,
 ( #30135, #19241, #14054, #11704, #27091, #19737, #17042, #27253, #4369, #14551 ),
 .UNSPECIFIED., .F., .F.,
 ( 4, 3, 3, 4 ),
 ( 0.000000000000000000, 0.0005352520061641845642, 0.001070504012328367827, 0.002130599830188110912 ),
 .UNSPECIFIED. ) ;
#28736 = CARTESIAN_POINT ( 'NONE',  ( -2.937550801365593323, -1.828967928396026732, 3.368539882008728004 ) ) ;
#28737 = CARTESIAN_POINT ( 'NONE',  ( 0.5640491561200829951, -9.516580665864454502, -0.6680154998155471979 ) ) ;
#28738 = CARTESIAN_POINT ( 'NONE',  ( 69.15470699321893733, -7.794592769514708586, 0.8105619180563019555 ) ) ;
#28739 = ORIENTED_EDGE ( 'NONE', *, *, #21346, .T. ) ;
#28740 = DIRECTION ( 'NONE',  ( -1.000000000000000000, -0.000000000000000000, 0.000000000000000000 ) ) ;
#28741 = EDGE_CURVE ( 'NONE', #2323, #22995, #9575, .T. ) ;
#28742 = B_SPLINE_CURVE_WITH_KNOTS ( 'NONE', 3,
 ( #7971, #26524, #28852, #18507, #313, #10485, #10638, #5952, #20697, #28367 ),
 .UNSPECIFIED., .F., .F.,
 ( 4, 2, 2, 2, 4 ),
 ( 2.493548413898819905E-07, 0.0005478513795029404899, 0.001095453404164491076, 0.001643055428826041770, 0.002190657453487592030 ),
 .UNSPECIFIED. ) ;
#28744 = EDGE_CURVE ( 'NONE', #17768, #17909, #7997, .T. ) ;
#28743 = ORIENTED_EDGE ( 'NONE', *, *, #18207, .T. ) ;
#28745 = COORDINATED_UNIVERSAL_TIME_OFFSET ( 0, 0, .AHEAD. ) ;
#28746 = DIRECTION ( 'NONE',  ( -0.8660254037844418162, 0.4999999999999946154, 0.000000000000000000 ) ) ;
#28747 = DIRECTION ( 'NONE',  ( 0.1908089953765452762, 0.000000000000000000, 0.9816271834476639757 ) ) ;
#28748 = VERTEX_POINT ( 'NONE', #18092 ) ;
#28749 = DIRECTION ( 'NONE',  ( 0.000000000000000000, 0.000000000000000000, -1.000000000000000000 ) ) ;
#28750 = ORIENTED_EDGE ( 'NONE', *, *, #21609, .T. ) ;
#28751 = ORIENTED_EDGE ( 'NONE', *, *, #9523, .T. ) ;
#28752 = EDGE_CURVE ( 'NONE', #30689, #2062, #7456, .T. ) ;
#28753 = DIRECTION ( 'NONE',  ( 0.000000000000000000, -0.9271838545667856479, -0.3746065934159163446 ) ) ;
#28754 = CARTESIAN_POINT ( 'NONE',  ( -3.912550801365593411, 3.675193018007246959, -1.088641768524161391 ) ) ;
#28755 = CARTESIAN_POINT ( 'NONE',  ( 20.07596637266183848, -16.49406355791779077, 1.500000000000000222 ) ) ;
#28756 = FACE_OUTER_BOUND ( 'NONE', #11950, .T. ) ;
#28758 = ORIENTED_EDGE ( 'NONE', *, *, #30491, .T. ) ;
#28757 = DIRECTION ( 'NONE',  ( 0.000000000000000000, 0.000000000000000000, 1.000000000000000000 ) ) ;
#28759 = CARTESIAN_POINT ( 'NONE',  ( -5.987550801365593145, -3.521866450007987037, -0.3701630799359323931 ) ) ;
#28760 = CARTESIAN_POINT ( 'NONE',  ( 14.61912536820988784, 9.825622711161967615, 1.500000000000000000 ) ) ;
#28761 = CARTESIAN_POINT ( 'NONE',  ( 7.249760686538667009, 2.210816291636326092, -8.466096581343458993 ) ) ;
#28762 = CARTESIAN_POINT ( 'NONE',  ( 21.17250000136559507, -2.363507492473152283, -1.913930629741525280 ) ) ;
#28763 = CARTESIAN_POINT ( 'NONE',  ( -3.608283490412349620E-16, -4.208382051008211278, 2.718385644597158812 ) ) ;
#28766 = EDGE_CURVE ( 'NONE', #28105, #6480, #23602, .T. ) ;
#28765 = ORIENTED_EDGE ( 'NONE', *, *, #20628, .F. ) ;
#28764 = FACE_OUTER_BOUND ( 'NONE', #17514, .T. ) ;
#28767 = CARTESIAN_POINT ( 'NONE',  ( 29.11693253002209758, -8.303828435806185126, 0.07017451552781737989 ) ) ;
#28768 = CARTESIAN_POINT ( 'NONE',  ( 22.79750000273118715, -2.594547506269383685, -0.7685399846772043020 ) ) ;
#28769 = CARTESIAN_POINT ( 'NONE',  ( -19.16594587638449099, 5.061405101124994310, 1.500000000000000000 ) ) ;
#28770 = ADVANCED_FACE ( 'NONE', ( #18262 ), #28476, .T. ) ;
#28771 = CARTESIAN_POINT ( 'NONE',  ( 15.28872660057386845, 20.76088595412476678, 4.629213727441584325 ) ) ;
#28772 = CARTESIAN_POINT ( 'NONE',  ( -2.760161469795139322, -0.06813755667441036279, -1.269913365998981192 ) ) ;
#28773 = CARTESIAN_POINT ( 'NONE',  ( 72.25703127509153489, -22.87839253411022611, 1.500000000000000000 ) ) ;
#28774 = CARTESIAN_POINT ( 'NONE',  ( 0.000000000000000000, 0.000000000000000000, 0.000000000000000000 ) ) ;
#28775 = ORIENTED_EDGE ( 'NONE', *, *, #1258, .F. ) ;
#28776 = CARTESIAN_POINT ( 'NONE',  ( 0.000000000000000000, 1.464956435139693758, -10.90201369670496945 ) ) ;
#28777 = CARTESIAN_POINT ( 'NONE',  ( 5.489343958331425632, -7.664144799260931507, -2.678936089601521520 ) ) ;
#28778 = CARTESIAN_POINT ( 'NONE',  ( 18.60402535543785518, -7.603424548862136589, -0.07017451552783579571 ) ) ;
#28780 = CARTESIAN_POINT ( 'NONE',  ( 107.4581749826926398, -17.47794492952237277, 4.757811978365556804 ) ) ;
#28779 = DIRECTION ( 'NONE',  ( -0.7822388118548813107, 0.4516257885949860884, 0.4291113938172937958 ) ) ;
#28781 = VERTEX_POINT ( 'NONE', #14857 ) ;
#28782 = CARTESIAN_POINT ( 'NONE',  ( -4.600050799999999995, -1.887961173149512062, -2.331437884370912261 ) ) ;
#28783 = ORIENTED_EDGE ( 'NONE', *, *, #31232, .T. ) ;
#28784 = FACE_OUTER_BOUND ( 'NONE', #28662, .T. ) ;
#28786 = ORIENTED_EDGE ( 'NONE', *, *, #9329, .T. ) ;
#28785 = FACE_OUTER_BOUND ( 'NONE', #8645, .T. ) ;
#28787 = ORIENTED_EDGE ( 'NONE', *, *, #22706, .F. ) ;
#28788 = CARTESIAN_POINT ( 'NONE',  ( 68.65514544479340486, -4.985459736530871488, 3.993435577424459648 ) ) ;
#28789 = EDGE_CURVE ( 'NONE', #4162, #16869, #32165, .T. ) ;
#28790 = EDGE_CURVE ( 'NONE', #18979, #6904, #30577, .T. ) ;
#28792 = ORIENTED_EDGE ( 'NONE', *, *, #11006, .T. ) ;
#28791 = CARTESIAN_POINT ( 'NONE',  ( -2.541067152580809729, 0.4393720697977929746, -1.497239384009418250 ) ) ;
#28793 = CARTESIAN_POINT ( 'NONE',  ( -5.427698642335591239E-12, -21.93932300456189566, 1.500000000000000000 ) ) ;
#28794 = CARTESIAN_POINT ( 'NONE',  ( 11.84010260670268089, -19.96226796878934451, -1.750548469652316586 ) ) ;
#28795 = DIRECTION ( 'NONE',  ( 0.1908089953765452484, 0.000000000000000000, 0.9816271834476638647 ) ) ;
#28796 = DIRECTION ( 'NONE',  ( -0.000000000000000000, 0.000000000000000000, 1.000000000000000000 ) ) ;
#28797 = ADVANCED_FACE ( 'NONE', ( #5185 ), #20081, .T. ) ;
#28798 = CARTESIAN_POINT ( 'NONE',  ( 101.9216173105994443, -5.769792427975428240, -0.07017451552783622593 ) ) ;
#28799 = DIRECTION ( 'NONE',  ( 0.000000000000000000, 1.000000000000000000, 0.000000000000000000 ) ) ;
#28800 = CIRCLE ( 'NONE', #30974, 15.00000000000000355 ) ;
#28801 = DIRECTION ( 'NONE',  ( 0.000000000000000000, -0.9063077870366508249, -0.4226182617406976094 ) ) ;
#28802 = CARTESIAN_POINT ( 'NONE',  ( -2.619932554246537343E-16, -3.055657119358776264, -3.641590349731960163 ) ) ;
#28803 = CARTESIAN_POINT ( 'NONE',  ( 10.00000000000000000, 1.625881193364757449, -4.467071865485455540 ) ) ;
#28804 = EDGE_CURVE ( 'NONE', #1551, #16558, #25246, .T. ) ;
#28805 = CARTESIAN_POINT ( 'NONE',  ( -48.50000000000000000, -10.96966150227468972, 0.9999999999999991118 ) ) ;
#28806 = CARTESIAN_POINT ( 'NONE',  ( 3.329122376115755344, 0.6654791810447507894, 0.9318852528021189796 ) ) ;
#28807 = VECTOR ( 'NONE', #14927, 1000.000000000000000 ) ;
#28808 =( BOUNDED_SURFACE ( )  B_SPLINE_SURFACE ( 3, 2, ( 
 ( #28983, #16268, #16576 ),
 ( #16085, #26317, #21283 ),
 ( #31187, #8268, #26139 ),
 ( #6082, #23627, #3428 ),
 ( #21137, #31336, #13588 ),
 ( #23794, #906, #26481 ),
 ( #13740, #23942, #1051 ),
 ( #11243, #21449, #3907 ),
 ( #14085, #1906, #11920 ),
 ( #22429, #9395, #32645 ),
 ( #32486, #14742, #14236 ),
 ( #12079, #24432, #29469 ),
 ( #24940, #7056, #9724 ),
 ( #17423, #24785, #29649 ),
 ( #12225, #21770, #6730 ),
 ( #4567, #24284, #4213 ),
 ( #19606, #1550, #29804 ),
 ( #30160, #22123, #32335 ),
 ( #1399, #32154, #6878 ),
 ( #4398, #17067, #9546 ),
 ( #2052, #4069, #22275 ),
 ( #16919, #1721, #19953 ),
 ( #11730, #21934, #26967 ),
 ( #7233, #27113, #31979 ),
 ( #27281, #9046, #14582 ),
 ( #6568, #11572, #9228 ),
 ( #24594, #19760, #19456 ),
 ( #29965, #14383, #17268 ),
 ( #27466, #19265, #16767 ),
 ( #12722, #17928, #32828 ),
 ( #28119, #20611, #32982 ),
 ( #12572, #18078, #25094 ),
 ( #10218, #13073, #23273 ),
 ( #22924, #4721, #7737 ),
 ( #9901, #20440, #30307 ),
 ( #2711, #14891, #7382 ),
 ( #17570, #5218, #32 ),
 ( #5065, #30463, #22617 ) ),
 .UNSPECIFIED., .F., .F., .F. ) 
 B_SPLINE_SURFACE_WITH_KNOTS ( ( 4, 2, 2, 2, 2, 2, 2, 2, 2, 2, 2, 2, 2, 2, 2, 2, 2, 2, 4 ),
 ( 3, 3 ),
 ( 0.007230792593457298703, 0.007246581719258846262, 0.007262370845060393820, 0.007270265407961168033, 0.007278159970861941379, 0.007293949096663488937, 0.007357105599869678304, 0.007483418606282057906, 0.007609731612694438374, 0.007736044619106817975, 0.007862357625519197576, 0.007988670631931578045, 0.008114983638343956779, 0.008178140141550147013, 0.008193929267351695439, 0.008209718393153242130, 0.008217612956054016343, 0.008225507518954788821, 0.008241296644756337247 ),
 ( 0.000000000000000000, 1.000000000000000000 ),
 .UNSPECIFIED. ) 
 GEOMETRIC_REPRESENTATION_ITEM ( )  RATIONAL_B_SPLINE_SURFACE ( (
 ( 1.000000000000000000, 0.7074680672122112268, 1.000000000000000000),
 ( 1.000000000000000000, 0.7074680692382261382, 1.000000000000000000),
 ( 1.000000000000000000, 0.7074680712595373677, 1.000000000000000000),
 ( 1.000000000000000000, 0.7074680752927113847, 1.000000000000000000),
 ( 1.000000000000000000, 0.7074685410474966796, 1.000000000000000000),
 ( 1.000000000000000000, 0.7074678484437120218, 1.000000000000000000),
 ( 1.000000000000000000, 0.7074669202766126208, 1.000000000000000000),
 ( 1.000000000000000000, 0.7074656694464243056, 1.000000000000000000),
 ( 1.000000000000000000, 0.7074650308517693720, 1.000000000000000000),
 ( 1.000000000000000000, 0.7074630745461631953, 1.000000000000000000),
 ( 1.000000000000000000, 0.7074617163714869150, 1.000000000000000000),
 ( 1.000000000000000000, 0.7074546413305010661, 1.000000000000000000),
 ( 1.000000000000000000, 0.7074480833215146536, 1.000000000000000000),
 ( 1.000000000000000000, 0.7074249281477825724, 1.000000000000000000),
 ( 1.000000000000000000, 0.7074047634757077985, 1.000000000000000000),
 ( 1.000000000000000000, 0.7073503653998111096, 1.000000000000000000),
 ( 1.000000000000000000, 0.7073152363876467064, 1.000000000000000000),
 ( 1.000000000000000000, 0.7072250595811295781, 1.000000000000000000),
 ( 1.000000000000000000, 0.7071666794510108600, 1.000000000000000000),
 ( 1.000000000000000000, 0.7070478450249763069, 1.000000000000000000),
 ( 1.000000000000000000, 0.7069901110841356751, 1.000000000000000000),
 ( 1.000000000000000000, 0.7068987577186105487, 1.000000000000000000),
 ( 1.000000000000000000, 0.7068634512106897194, 1.000000000000000000),
 ( 1.000000000000000000, 0.7068087972553998011, 1.000000000000000000),
 ( 1.000000000000000000, 0.7067884384462148617, 1.000000000000000000),
 ( 1.000000000000000000, 0.7067650571034519436, 1.000000000000000000),
 ( 1.000000000000000000, 0.7067584107639131030, 1.000000000000000000),
 ( 1.000000000000000000, 0.7067512283872569023, 1.000000000000000000),
 ( 1.000000000000000000, 0.7067498488587909966, 1.000000000000000000),
 ( 1.000000000000000000, 0.7067471983191341289, 1.000000000000000000),
 ( 1.000000000000000000, 0.7067453388308237994, 1.000000000000000000),
 ( 1.000000000000000000, 0.7067443930682688613, 1.000000000000000000),
 ( 1.000000000000000000, 0.7067447018949120086, 1.000000000000000000),
 ( 1.000000000000000000, 0.7067447029564462024, 1.000000000000000000),
 ( 1.000000000000000000, 0.7067447034884694057, 1.000000000000000000),
 ( 1.000000000000000000, 0.7067447050884115844, 1.000000000000000000),
 ( 1.000000000000000000, 0.7067447061600561353, 1.000000000000000000),
 ( 1.000000000000000000, 0.7067447072368862049, 1.000000000000000000) ) ) 
 REPRESENTATION_ITEM ( '' )  SURFACE ( )  );
#28809 = APPROVAL ( #27137, 'UNKNOWN' ) ;
#28810 = ORIENTED_EDGE ( 'NONE', *, *, #3437, .T. ) ;
#28811 = CARTESIAN_POINT ( 'NONE',  ( 68.56906952848856918, -3.255983411059098831, 0.07017451552782104363 ) ) ;
#28812 = CARTESIAN_POINT ( 'NONE',  ( 107.1769020805352142, 16.40214705320006061, 1.508259000770582725 ) ) ;
#28813 = DIRECTION ( 'NONE',  ( -0.000000000000000000, 0.7071067811865507924, 0.7071067811865441310 ) ) ;
#28814 = VERTEX_POINT ( 'NONE', #30428 ) ;
#28815 = CARTESIAN_POINT ( 'NONE',  ( 23.92250000136559507, 0.3178988483021036315, 3.024605502323848949 ) ) ;
#28816 = B_SPLINE_CURVE_WITH_KNOTS ( 'NONE', 3,
 ( #5327, #7841, #7682, #17880, #2349, #28073, #7333, #2507, #22560, #5018, #7489, #4670, #5170, #20718, #27718, #15196, #333, #2852, #2158, #20215, #12676, #18034, #33082 ),
 .UNSPECIFIED., .F., .F.,
 ( 4, 2, 2, 2, 2, 2, 2, 1, 2, 2, 2, 4 ),
 ( 0.5000000000000000000, 0.5443742905368078588, 0.5887485810736157177, 0.6109357263420195361, 0.6331228716104234655, 0.6774971621472312133, 0.6996843074156350317, 0.7218714526840389611, 0.7440585979524427795, 0.7662457432208467090, 0.8106200337576545678, 0.8549943242944623156 ),
 .UNSPECIFIED. ) ;
#28817 = CARTESIAN_POINT ( 'NONE',  ( 0.000000000000000000, 20.00000000000000000, 0.000000000000000000 ) ) ;
#28818 = CARTESIAN_POINT ( 'NONE',  ( 20.75046113880788923, -21.62010873700192803, -1.554218361998998210 ) ) ;
#28819 = ORIENTED_EDGE ( 'NONE', *, *, #30438, .F. ) ;
#28820 = CARTESIAN_POINT ( 'NONE',  ( 0.6071737056423955892, -7.494373765315226699, -1.499999999999999778 ) ) ;
#28821 = ORIENTED_EDGE ( 'NONE', *, *, #4820, .T. ) ;
#28822 = AXIS2_PLACEMENT_3D ( 'NONE', #20991, #22981, #10609 ) ;
#28823 = VECTOR ( 'NONE', #3085, 1000.000000000000000 ) ;
#28824 = ORIENTED_EDGE ( 'NONE', *, *, #8233, .T. ) ;
#28825 = CARTESIAN_POINT ( 'NONE',  ( 25.10129074173041985, -17.52164282029558962, -1.281897516810667215 ) ) ;
#28826 = APPROVAL_ROLE ( '' ) ;
#28828 = VERTEX_POINT ( 'NONE', #32793 ) ;
#28827 = LINE ( 'NONE', #16438, #3731 ) ;
#28829 = ORIENTED_EDGE ( 'NONE', *, *, #10388, .F. ) ;
#28830 = DIRECTION ( 'NONE',  ( 0.000000000000000000, 0.000000000000000000, -1.000000000000000000 ) ) ;
#28831 = EDGE_CURVE ( 'NONE', #3275, #19087, #3730, .T. ) ;
#28832 = ORIENTED_EDGE ( 'NONE', *, *, #15446, .T. ) ;
#28833 = AXIS2_PLACEMENT_3D ( 'NONE', #5216, #5377, #20760 ) ;
#28834 = CARTESIAN_POINT ( 'NONE',  ( 5.489321289187128805, 0.1038943573682652305, -8.118169347437836691 ) ) ;
#28836 = EDGE_LOOP ( 'NONE', ( #1311, #31471, #13536, #23784, #10363 ) ) ;
#28835 = CARTESIAN_POINT ( 'NONE',  ( 84.85832005755729313, -2.331047133796639859, -0.07017451552781768520 ) ) ;
#28837 = CARTESIAN_POINT ( 'NONE',  ( 21.79750000273118715, -2.594547506269383685, -0.7685399846772043020 ) ) ;
#28838 = LINE ( 'NONE', #13773, #30426 ) ;
#28839 = CARTESIAN_POINT ( 'NONE',  ( 3.499999999999999556, 5.471841788314708133, 3.018103451449746899 ) ) ;
#28840 = DIRECTION ( 'NONE',  ( 3.623545766764145597E-17, 0.4226182617406914477, 0.9063077870366536004 ) ) ;
#28841 = CARTESIAN_POINT ( 'NONE',  ( 108.0265366049212332, -18.45148262600833178, 4.417053837905102753 ) ) ;
#28842 = FACE_OUTER_BOUND ( 'NONE', #14524, .T. ) ;
#28843 = CARTESIAN_POINT ( 'NONE',  ( 3.541509388326463004, -13.88765124358303993, -4.522129901861164925 ) ) ;
#28844 = CARTESIAN_POINT ( 'NONE',  ( 41.35669399755376929, -8.343390166152927279, -1.169951067574412473 ) ) ;
#28845 = CARTESIAN_POINT ( 'NONE',  ( -6.800050802731188782, 3.113457007523260156, -0.9222479816126439855 ) ) ;
#28846 = CIRCLE ( 'NONE', #9622, 6.000000000000001776 ) ;
#28848 = EDGE_CURVE ( 'NONE', #32470, #27641, #20293, .T. ) ;
#28847 = AXIS2_PLACEMENT_3D ( 'NONE', #830, #1138, #6156 ) ;
#28849 = LINE ( 'NONE', #5949, #26740 ) ;
#28850 = CARTESIAN_POINT ( 'NONE',  ( 23.27353278736381981, -21.94187821002792660, 1.000000000000000000 ) ) ;
#28851 = CARTESIAN_POINT ( 'NONE',  ( 0.000000000000000000, 0.000000000000000000, 0.000000000000000000 ) ) ;
#28852 = CARTESIAN_POINT ( 'NONE',  ( 5.612718825656735966, -6.420171604529151921, -5.126902779943848465 ) ) ;
#28853 = VECTOR ( 'NONE', #20643, 1000.000000000000000 ) ;
#28854 = CARTESIAN_POINT ( 'NONE',  ( 21.48499999999999943, -2.486304738420683780, 0.2613211581691335383 ) ) ;
#28855 = CARTESIAN_POINT ( 'NONE',  ( -4.512550801365592612, 1.088641768524161613, 3.675193018007247403 ) ) ;
#28856 = ORIENTED_EDGE ( 'NONE', *, *, #7767, .F. ) ;
#28857 = CARTESIAN_POINT ( 'NONE',  ( -5.000050800000001239, 1.887961173149511618, 2.331437884370912705 ) ) ;
#28858 = VECTOR ( 'NONE', #29879, 1000.000000000000000 ) ;
#28859 = CARTESIAN_POINT ( 'NONE',  ( 2.274274201625327230, 0.000000000000000000, 0.000000000000000000 ) ) ;
#28860 = CARTESIAN_POINT ( 'NONE',  ( 3.063284526839890720, 8.461683424509336859, -2.223716399045483794 ) ) ;
#28861 = CARTESIAN_POINT ( 'NONE',  ( 7.461135469111389362, -4.560857689425765749, 1.500000000000283995 ) ) ;
#28862 = VERTEX_POINT ( 'NONE', #7506 ) ;
#28863 = CARTESIAN_POINT ( 'NONE',  ( 18.86054332783516330, -4.736068442360130248, -3.993434336035624366 ) ) ;
#28864 = EDGE_CURVE ( 'NONE', #27055, #19054, #8008, .T. ) ;
#28865 = VERTEX_POINT ( 'NONE', #20400 ) ;
#28866 = CARTESIAN_POINT ( 'NONE',  ( 7.249760686538667009, -2.318425219014288885, 8.437262856154156054 ) ) ;
#28867 = ADVANCED_FACE ( 'NONE', ( #4842 ), #15995, .F. ) ;
#28868 = APPLICATION_PROTOCOL_DEFINITION ( 'international standard', 'config_control_design', 1994, #30225 ) ;
#28869 = VECTOR ( 'NONE', #10358, 1000.000000000000000 ) ;
#28870 = CARTESIAN_POINT ( 'NONE',  ( 102.3595522875203159, -3.079674301855471974, 4.215290384276481284 ) ) ;
#28871 = AXIS2_PLACEMENT_3D ( 'NONE', #19105, #3247, #11425 ) ;
#28872 = CARTESIAN_POINT ( 'NONE',  ( 8.911384905465473238, 0.2172754300402683358, 1.412391582771866716 ) ) ;
#28873 = AXIS2_PLACEMENT_3D ( 'NONE', #8030, #30296, #7725 ) ;
#28874 = CARTESIAN_POINT ( 'NONE',  ( 13.04731869766886554, 19.33256796700939262, 5.412820279296879811 ) ) ;
#28875 = EDGE_LOOP ( 'NONE', ( #6411, #14914, #5797, #5675 ) ) ;
#28876 = CARTESIAN_POINT ( 'NONE',  ( 4.749760686538667009, 8.014274990069656823, -8.669741416787380218E-17 ) ) ;
#28877 = CARTESIAN_POINT ( 'NONE',  ( 0.7632845268398871230, 8.734705317681626724, -0.4999240074894737984 ) ) ;
#28878 = CARTESIAN_POINT ( 'NONE',  ( 2.437082531750065506, -7.858345965138736844, -7.214115859539328213 ) ) ;
#28879 = AXIS2_PLACEMENT_3D ( 'NONE', #14564, #11903, #9379 ) ;
#28881 = VERTEX_POINT ( 'NONE', #2523 ) ;
#28880 = CARTESIAN_POINT ( 'NONE',  ( 24.39659513448100725, -17.41072360183587264, -1.416990234759457401 ) ) ;
#28882 = CARTESIAN_POINT ( 'NONE',  ( -2.462550801365593678, 0.3701630799359330593, -3.521866450007987037 ) ) ;
#28883 = CARTESIAN_POINT ( 'NONE',  ( -56.27770248097862549, 0.4996615022747108448, -1.050000000000000044 ) ) ;
#28884 = CARTESIAN_POINT ( 'NONE',  ( 54.99820130842492460, -7.257205178588800543, -2.787782628555286468 ) ) ;
#28885 = EDGE_LOOP ( 'NONE', ( #24531, #10580, #10823, #14917, #9176 ) ) ;
#28886 = VERTEX_POINT ( 'NONE', #7348 ) ;
#28887 = CARTESIAN_POINT ( 'NONE',  ( 10.56183597391177464, 5.003758587302147731, 0.2500000000000008882 ) ) ;
#28888 = DIRECTION ( 'NONE',  ( -1.000000000000000000, 0.000000000000000000, 0.000000000000000000 ) ) ;
#28889 = CYLINDRICAL_SURFACE ( 'NONE', #4929, 0.5000000000000000000 ) ;
#28890 = CARTESIAN_POINT ( 'NONE',  ( 41.92799935459299832, -21.01937708444107855, 4.522129901861156931 ) ) ;
#28891 = CIRCLE ( 'NONE', #14455, 8.750000000000000000 ) ;
#28892 = VECTOR ( 'NONE', #510, 1000.000000000000114 ) ;
#28893 = DIRECTION ( 'NONE',  ( 1.000000000000000000, -0.000000000000000000, -0.000000000000000000 ) ) ;
#28894 = AXIS2_PLACEMENT_3D ( 'NONE', #10020, #20229, #5343 ) ;
#28895 = VECTOR ( 'NONE', #5027, 1000.000000000000000 ) ;
#28896 = CARTESIAN_POINT ( 'NONE',  ( 6.524595395369781947, 2.369138865965942031, -8.328507089302155109 ) ) ;
#28897 = CARTESIAN_POINT ( 'NONE',  ( -57.12917293608614955, -2.964366234459023808, 5.871858320049880398 ) ) ;
#28898 = AXIS2_PLACEMENT_3D ( 'NONE', #11494, #21690, #22808 ) ;
#28899 = CARTESIAN_POINT ( 'NONE',  ( -2.987550801365593145, -0.3701630799359326152, 3.521866450007987037 ) ) ;
#28900 = CARTESIAN_POINT ( 'NONE',  ( 7.249760686538667009, -5.151476664237518044, 6.139290821770238438 ) ) ;
#28901 = CARTESIAN_POINT ( 'NONE',  ( 55.02400815819125768, -8.185693696756606741, 0.8105616793101843021 ) ) ;
#28902 = AXIS2_PLACEMENT_3D ( 'NONE', #16260, #18767, #18601 ) ;
#28903 = ORIENTED_EDGE ( 'NONE', *, *, #31075, .F. ) ;
#28904 = EDGE_CURVE ( 'NONE', #26497, #7095, #14192, .T. ) ;
#28905 = CARTESIAN_POINT ( 'NONE',  ( -23.54713438637982748, 8.443947424854778561, 8.182767265444946148 ) ) ;
#28906 = EDGE_CURVE ( 'NONE', #7656, #25302, #12690, .T. ) ;
#28907 = VECTOR ( 'NONE', #15909, 1000.000000000000000 ) ;
#28908 = VECTOR ( 'NONE', #25472, 1000.000000000000227 ) ;
#28909 = ORIENTED_EDGE ( 'NONE', *, *, #28258, .F. ) ;
#28910 = DATE_AND_TIME ( #31594, #11396 ) ;
#28911 = CARTESIAN_POINT ( 'NONE',  ( 54.97716868250573441, -6.504553498923070443, 3.996604662709783540 ) ) ;
#28912 = CARTESIAN_POINT ( 'NONE',  ( 0.7632845268398871230, -2.223716399045513548, -8.461683424509338636 ) ) ;
#28913 = VERTEX_POINT ( 'NONE', #30783 ) ;
#28914 = CARTESIAN_POINT ( 'NONE',  ( 5.772270645472297623, 14.99679128811751916, 2.402751277358659454 ) ) ;
#28915 = EDGE_LOOP ( 'NONE', ( #8843, #13001, #2053 ) ) ;
#28916 = AXIS2_PLACEMENT_3D ( 'NONE', #26278, #3394, #26597 ) ;
#28917 = EDGE_LOOP ( 'NONE', ( #25507, #17017, #20333 ) ) ;
#28918 = CARTESIAN_POINT ( 'NONE',  ( 3.249999999999999556, -6.807171995660538322, -6.478011392632959442 ) ) ;
#28919 = CARTESIAN_POINT ( 'NONE',  ( -3.362550801365593589, -2.228590825266444586, -2.752080473201636401 ) ) ;
#28920 = AXIS2_PLACEMENT_3D ( 'NONE', #4112, #14278, #1948 ) ;
#28921 = CARTESIAN_POINT ( 'NONE',  ( 7.085399849431558650, -9.284427924817970634, 1.499999999999999556 ) ) ;
#28922 = TOROIDAL_SURFACE ( 'NONE', #24084, 301.4345239564033250, 3.999999999999999112 ) ;
#28923 = CARTESIAN_POINT ( 'NONE',  ( 0.3238988396964614935, -5.504238404182476785, -1.499999999999999778 ) ) ;
#28925 = ORIENTED_EDGE ( 'NONE', *, *, #11876, .T. ) ;
#28924 = CARTESIAN_POINT ( 'NONE',  ( -50.60000000000000142, -10.96966150227468972, 7.500000000000000000 ) ) ;
#28926 = CARTESIAN_POINT ( 'NONE',  ( -7.087550801365593678, 2.228590825266444142, 2.752080473201636845 ) ) ;
#28927 = CIRCLE ( 'NONE', #27327, 0.5000000000000000000 ) ;
#28928 = CARTESIAN_POINT ( 'NONE',  ( 3.249999999999999556, 0.000000000000000000, 0.000000000000000000 ) ) ;
#28929 = DIRECTION ( 'NONE',  ( -1.000000000000000000, 2.473959037481237219E-13, 0.000000000000000000 ) ) ;
#28930 = CARTESIAN_POINT ( 'NONE',  ( 20.98500000136559862, -2.892927487894331406, 1.570731468192932301 ) ) ;
#28931 = VECTOR ( 'NONE', #6722, 999.9999999999998863 ) ;
#28933 = ORIENTED_EDGE ( 'NONE', *, *, #25553, .T. ) ;
#28932 = CARTESIAN_POINT ( 'NONE',  ( 2.357329973329931772, -4.593471141847137673, 9.815384016743307072 ) ) ;
#28934 = VECTOR ( 'NONE', #20327, 1000.000000000000000 ) ;
#28935 = B_SPLINE_CURVE_WITH_KNOTS ( 'NONE', 3,
 ( #15906, #18261, #20279, #25617, #26116, #12906, #30483, #17769, #30679, #10725 ),
 .UNSPECIFIED., .F., .F.,
 ( 4, 2, 2, 2, 4 ),
 ( 3.252606517456513302E-19, 0.0009730977530606437073, 0.001946195506121287198, 0.002919293259181930580, 0.003892391012242573962 ),
 .UNSPECIFIED. ) ;
#28936 = VECTOR ( 'NONE', #28489, 1000.000000000000000 ) ;
#28937 = DIRECTION ( 'NONE',  ( -3.623545766764141283E-17, -0.4226182617406913922, -0.9063077870366536004 ) ) ;
#28938 = CARTESIAN_POINT ( 'NONE',  ( 23.17250000273118715, 2.378061970571979433, -1.291182301015470824 ) ) ;
#28939 = FACE_OUTER_BOUND ( 'NONE', #16965, .T. ) ;
#28940 = CARTESIAN_POINT ( 'NONE',  ( 18.70785785862773665, -6.442785551927881826, -3.084862407554554320 ) ) ;
#28941 = DIRECTION ( 'NONE',  ( -0.000000000000000000, -1.000000000000000000, -0.000000000000000000 ) ) ;
#28942 = EDGE_CURVE ( 'NONE', #24335, #5149, #13835, .T. ) ;
#28943 = VECTOR ( 'NONE', #24511, 1000.000000000000114 ) ;
#28944 = CARTESIAN_POINT ( 'NONE',  ( -34.48223484310472031, 0.5000000000000000000, -2.482234843104710986 ) ) ;
#28945 = B_SPLINE_SURFACE_WITH_KNOTS ( 'NONE', 3, 3, ( 
 ( #86, #10276, #20495, #2446, #7781, #28162, #2269, #5264, #15437, #12946 ),
 ( #10446, #23163, #32871, #30861, #9939, #17314, #24982, #2093, #20153, #30349 ),
 ( #22484, #32699, #17618, #9779, #20001, #30198, #17460, #27824, #12614, #12777 ),
 ( #17991, #22834, #4962, #15145, #25667, #20170, #15457, #2786, #25354, #28179 ) ),
 .UNSPECIFIED., .F., .F., .F.,
 ( 4, 4 ),
 ( 4, 3, 3, 4 ),
 ( -1.162439711433475187E-14, 1.000000000000000000 ),
 ( 0.009524646911531629151, 0.5047623234557657712, 0.7523811617278828301, 1.000000000000000000 ),
 .UNSPECIFIED. ) ;
#28946 = CIRCLE ( 'NONE', #32159, 10.97000000000000064 ) ;
#28947 = AXIS2_PLACEMENT_3D ( 'NONE', #22781, #2560, #5071 ) ;
#28948 = CARTESIAN_POINT ( 'NONE',  ( -34.48223484310472031, 0.000000000000000000, -2.482234843104710986 ) ) ;
#28949 = CARTESIAN_POINT ( 'NONE',  ( -6.937550801365595099, -1.828967928396026510, 3.368539882008728004 ) ) ;
#28950 = ORIENTED_EDGE ( 'NONE', *, *, #19200, .T. ) ;
#28951 = ADVANCED_FACE ( 'NONE', ( #5344 ), #20731, .T. ) ;
#28952 = VECTOR ( 'NONE', #18962, 1000.000000000000000 ) ;
#28953 = VECTOR ( 'NONE', #24701, 1000.000000000000000 ) ;
#28954 = TOROIDAL_SURFACE ( 'NONE', #9654, 0.05000000000000002359, 0.4500000000000000111 ) ;
#28955 = DIRECTION ( 'NONE',  ( -1.000000000000000000, 0.000000000000000000, 0.000000000000000000 ) ) ;
#28956 = EDGE_CURVE ( 'NONE', #28865, #28455, #12130, .T. ) ;
#28957 = CARTESIAN_POINT ( 'NONE',  ( 25.75999999999999801, -2.208672634433321348E-15, -2.499999999999997780 ) ) ;
#28960 = CARTESIAN_POINT ( 'NONE',  ( 107.4494258168277554, -17.35106999866604127, 4.497200797759677293 ) ) ;
#28959 = CARTESIAN_POINT ( 'NONE',  ( 0.1255855353732055757, -9.314797388894898944, 5.239665997526856245 ) ) ;
#28958 = AXIS2_PLACEMENT_3D ( 'NONE', #9335, #12022, #22216 ) ;
#28961 = VERTEX_POINT ( 'NONE', #17472 ) ;
#28962 = AXIS2_PLACEMENT_3D ( 'NONE', #17520, #2654, #27714 ) ;
#28963 = CARTESIAN_POINT ( 'NONE',  ( -31.80959807272228090, -0.0003384977252905707612, 0.000000000000000000 ) ) ;
#28964 = ORIENTED_EDGE ( 'NONE', *, *, #18951, .F. ) ;
#28965 = DIRECTION ( 'NONE',  ( -0.000000000000000000, 0.000000000000000000, 1.000000000000000000 ) ) ;
#28966 = ORIENTED_EDGE ( 'NONE', *, *, #22824, .F. ) ;
#28967 = ADVANCED_FACE ( 'NONE', ( #24992 ), #19509, .F. ) ;
#28968 = ORIENTED_EDGE ( 'NONE', *, *, #10267, .F. ) ;
#28969 = DIRECTION ( 'NONE',  ( 1.000000000000000000, -8.574039729943018344E-17, -0.000000000000000000 ) ) ;
#28970 = AXIS2_PLACEMENT_3D ( 'NONE', #6995, #9167, #12178 ) ;
#28971 = B_SPLINE_CURVE_WITH_KNOTS ( 'NONE', 3,
 ( #14849, #25049, #12837, #33093, #28081, #30925, #27727, #4836, #22888, #177 ),
 .UNSPECIFIED., .F., .F.,
 ( 4, 2, 2, 2, 4 ),
 ( 1.968338519012285402E-07, 0.0005467926089500457082, 0.001093388384048190210, 0.001639984159146334712, 0.002186579934244479214 ),
 .UNSPECIFIED. ) ;
#28972 = DIRECTION ( 'NONE',  ( 0.000000000000000000, 0.000000000000000000, 1.000000000000000000 ) ) ;
#28974 = EDGE_LOOP ( 'NONE', ( #15950, #18017, #19064, #7665 ) ) ;
#28973 = CARTESIAN_POINT ( 'NONE',  ( 7.249760686538667009, -4.007137495034764463, -6.940565734314639634 ) ) ;
#28975 = VECTOR ( 'NONE', #8973, 1000.000000000000114 ) ;
#28976 = CARTESIAN_POINT ( 'NONE',  ( 12.22604216760896989, 4.899348760700370065, -1.050000000000000044 ) ) ;
#28977 = CARTESIAN_POINT ( 'NONE',  ( -3.348814662102636230, -1.982334143703736062, -1.747785174145542575 ) ) ;
#28978 = VECTOR ( 'NONE', #8055, 999.9999999999998863 ) ;
#28979 = EDGE_CURVE ( 'NONE', #3016, #25317, #29342, .T. ) ;
#28980 = DIRECTION ( 'NONE',  ( -1.000000000000000000, -0.000000000000000000, -0.000000000000000000 ) ) ;
#28981 = VECTOR ( 'NONE', #842, 1000.000000000000000 ) ;
#28982 = CARTESIAN_POINT ( 'NONE',  ( 6.653983693897041363, -6.711078333448701194, -1.500000000000000000 ) ) ;
#28983 = CARTESIAN_POINT ( 'NONE',  ( 107.9801098452135335, -17.78294883574212548, -4.320080270629262031 ) ) ;
#28984 = CARTESIAN_POINT ( 'NONE',  ( -4.750050802731187183, -2.983565686104819648, -0.3135853898029605791 ) ) ;
#28985 = AXIS2_PLACEMENT_3D ( 'NONE', #10370, #31272, #5825 ) ;
#28986 = CIRCLE ( 'NONE', #16674, 6.000000000000000888 ) ;
#28987 = EDGE_CURVE ( 'NONE', #6030, #3357, #24485, .T. ) ;
#28988 = CARTESIAN_POINT ( 'NONE',  ( -7.077711312404032898E-17, -0.8254815157534933778, -4.681538312723525053 ) ) ;
#28989 = CARTESIAN_POINT ( 'NONE',  ( 35.29731606331253602, -6.671246578258705817, 3.993434333679761306 ) ) ;
#28990 = CARTESIAN_POINT ( 'NONE',  ( -2.819379691724115400, -6.927609664242504017, 4.522129901861158707 ) ) ;
#28991 = DIRECTION ( 'NONE',  ( 0.000000000000000000, 0.000000000000000000, 1.000000000000000000 ) ) ;
#28992 = ORIENTED_EDGE ( 'NONE', *, *, #22420, .T. ) ;
#28993 = DIRECTION ( 'NONE',  ( -1.000000000000000000, 0.000000000000000000, 0.000000000000000000 ) ) ;
#28994 = EDGE_CURVE ( 'NONE', #29455, #25356, #31486, .T. ) ;
#28995 = DIRECTION ( 'NONE',  ( -0.000000000000000000, 0.000000000000000000, 1.000000000000000000 ) ) ;
#28996 = EDGE_CURVE ( 'NONE', #23130, #8778, #530, .T. ) ;
#28997 = CARTESIAN_POINT ( 'NONE',  ( 2.589202797589367222, 10.26630467377258604, 1.003524335601056139 ) ) ;
#28998 = ORIENTED_EDGE ( 'NONE', *, *, #13931, .T. ) ;
#28999 = CIRCLE ( 'NONE', #8706, 5.009999999999999787 ) ;
#29000 = CIRCLE ( 'NONE', #26338, 6.249000000000000554 ) ;
#29001 = CARTESIAN_POINT ( 'NONE',  ( 25.29462333114494044, -1.188618013303065268, 2.273567320650588641 ) ) ;
#29002 = CARTESIAN_POINT ( 'NONE',  ( 2.864531019710238269, 8.868883597856997980, 3.575186956654012427 ) ) ;
#29004 = ORIENTED_EDGE ( 'NONE', *, *, #1446, .F. ) ;
#29003 = AXIS2_PLACEMENT_3D ( 'NONE', #11347, #28732, #3172 ) ;
#29005 = DIRECTION ( 'NONE',  ( 0.4999999999999977796, 0.8660254037844399289, 0.000000000000000000 ) ) ;
#29006 = ADVANCED_FACE ( 'NONE', ( #27520 ), #24840, .F. ) ;
#29007 = ORIENTED_EDGE ( 'NONE', *, *, #25772, .F. ) ;
#29008 = AXIS2_PLACEMENT_3D ( 'NONE', #11517, #1491, #18892 ) ;
#29009 = ORIENTED_EDGE ( 'NONE', *, *, #6346, .F. ) ;
#29010 = CARTESIAN_POINT ( 'NONE',  ( 24.35085591271539229, -17.33674746172404824, -1.318654801572369584 ) ) ;
#29011 = APPROVAL_DATE_TIME ( #20997, #8983 ) ;
#29013 = VERTEX_POINT ( 'NONE', #20164 ) ;
#29012 = CARTESIAN_POINT ( 'NONE',  ( 4.749760686538667009, -5.151476664237435443, -6.139290821770307716 ) ) ;
#29014 = ORIENTED_EDGE ( 'NONE', *, *, #2990, .T. ) ;
#29015 = DIRECTION ( 'NONE',  ( 0.000000000000000000, 0.08715574274766894891, -0.9961946980917446570 ) ) ;
#29016 = CC_DESIGN_APPROVAL ( #8398, ( #1036 ) ) ;
#29017 = EDGE_CURVE ( 'NONE', #25797, #29167, #1599, .T. ) ;
#29018 = EDGE_LOOP ( 'NONE', ( #2999, #9801 ) ) ;
#29019 = LINE ( 'NONE', #14420, #54 ) ;
#29021 = VERTEX_POINT ( 'NONE', #25161 ) ;
#29020 = CARTESIAN_POINT ( 'NONE',  ( 68.93909985280586739, -3.497255374392172822, -1.529340295388946336 ) ) ;
#29022 = CARTESIAN_POINT ( 'NONE',  ( -4.912942406915327354, -5.022711880624455567E-15, 2.999999999999999556 ) ) ;
#29023 = CARTESIAN_POINT ( 'NONE',  ( 1.750000000000000222, 6.745408891279541130, 5.171987904998129437 ) ) ;
#29024 = CARTESIAN_POINT ( 'NONE',  ( 10.56870887191539587, 1.625881193364696831, 4.467071865485476856 ) ) ;
#29025 = DIRECTION ( 'NONE',  ( 6.062761635205510427E-17, 0.7071067811865392461, 0.7071067811865558994 ) ) ;
#29026 = FACE_OUTER_BOUND ( 'NONE', #10395, .T. ) ;
#29027 =( BOUNDED_CURVE ( )  B_SPLINE_CURVE ( 2, ( #22520, #15613, #30060, #2123, #12303, #9817, #6379, #31483, #8566, #16416, #26788 ),
 .UNSPECIFIED., .F., .F. ) 
 B_SPLINE_CURVE_WITH_KNOTS ( ( 3, 2, 2, 2, 2, 3 ),
 ( 0.6853822619934377691, 0.6875000000000000000, 0.7031250000000000000, 0.7187500000000000000, 0.7343750000000000000, 0.7478822619934377691 ),
 .UNSPECIFIED. ) 
 CURVE ( )  GEOMETRIC_REPRESENTATION_ITEM ( )  RATIONAL_B_SPLINE_CURVE ( ( 0.9821626249036861100, 0.9896829947469995004, 1.000000000000000000, 0.9238795325112867385, 1.000000000000000000, 0.9238795325112867385, 1.000000000000000000, 0.9238795325112867385, 1.000000000000000000, 0.9341965377642872381, 0.9821626249036861100 ) ) 
 REPRESENTATION_ITEM ( '' )  );
#29028 = VECTOR ( 'NONE', #941, 1000.000000000000000 ) ;
#29029 = DIRECTION ( 'NONE',  ( -0.000000000000000000, 0.8191520442889933529, -0.5735764363510439390 ) ) ;
#29030 = CARTESIAN_POINT ( 'NONE',  ( -34.48223484310472031, 0.5000000000000000000, -2.482234843104710986 ) ) ;
#29031 = CARTESIAN_POINT ( 'NONE',  ( 55.02400815819124347, -8.185693696756027649, -0.8105616793142609300 ) ) ;
#29032 = DIRECTION ( 'NONE',  ( 1.000000000000000000, 0.000000000000000000, 0.000000000000000000 ) ) ;
#29033 = CIRCLE ( 'NONE', #30099, 296.4345239564032113 ) ;
#29034 = EDGE_CURVE ( 'NONE', #19511, #3232, #21334, .T. ) ;
#29035 = CIRCLE ( 'NONE', #231, 4.000000000000001776 ) ;
#29036 = VECTOR ( 'NONE', #1145, 1000.000000000000000 ) ;
#29037 = CARTESIAN_POINT ( 'NONE',  ( -23.54713438637982748, 8.275374457817619600, 8.600000000000003197 ) ) ;
#29038 = CARTESIAN_POINT ( 'NONE',  ( 24.39659513448100725, -17.41072360183587264, -1.416990234759457401 ) ) ;
#29039 = CARTESIAN_POINT ( 'NONE',  ( 24.17249999999999943, 1.291182301015469047, 2.378061970571981654 ) ) ;
#29040 = CARTESIAN_POINT ( 'NONE',  ( -15.12340757463330654, -27.93932300454937590, -1.000000000000000000 ) ) ;
#29041 = EDGE_CURVE ( 'NONE', #18803, #9165, #27735, .T. ) ;
#29042 = LOCAL_TIME ( 16, 7, 10.00000000000000000, #29707 ) ;
#29043 = DIRECTION ( 'NONE',  ( -1.000000000000000000, 8.574039729943018344E-17, -0.000000000000000000 ) ) ;
#29044 = EDGE_CURVE ( 'NONE', #5581, #30729, #4797, .T. ) ;
#29045 = CARTESIAN_POINT ( 'NONE',  ( -4.712550801365592790, 3.675193018007247403, -1.088641768524161391 ) ) ;
#29046 = EDGE_LOOP ( 'NONE', ( #19746, #2691, #1678, #24631, #17466 ) ) ;
#29047 = CARTESIAN_POINT ( 'NONE',  ( -7.300050800000001061, -0.3135853898029607456, 2.983565686104819648 ) ) ;
#29048 = LINE ( 'NONE', #15977, #1810 ) ;
#29049 = CYLINDRICAL_SURFACE ( 'NONE', #1778, 4.000000000000001776 ) ;
#29050 = CARTESIAN_POINT ( 'NONE',  ( 7.154313482939235413, -6.723190066307162205, 1.499999999999999112 ) ) ;
#29051 = ORIENTED_EDGE ( 'NONE', *, *, #16475, .T. ) ;
#29052 = CARTESIAN_POINT ( 'NONE',  ( 28.69355067552991656, -5.615744008499413908, -3.993434336023910625 ) ) ;
#29053 = VECTOR ( 'NONE', #27962, 1000.000000000000000 ) ;
#29054 = AXIS2_PLACEMENT_3D ( 'NONE', #28396, #5666, #18675 ) ;
#29055 = ORIENTED_EDGE ( 'NONE', *, *, #16319, .F. ) ;
#29056 = CARTESIAN_POINT ( 'NONE',  ( 4.773472048928010025, -12.83524871782340959, 1.756822611201597661 ) ) ;
#29057 = COORDINATED_UNIVERSAL_TIME_OFFSET ( 0, 0, .AHEAD. ) ;
#29058 = CARTESIAN_POINT ( 'NONE',  ( 54.96823639739091760, -6.181812932795780924, 4.275175837987727157 ) ) ;
#29059 = EDGE_CURVE ( 'NONE', #24998, #17028, #1605, .T. ) ;
#29060 = APPROVAL ( #15222, 'UNSPECIFIED' ) ;
#29061 = CARTESIAN_POINT ( 'NONE',  ( 3.499999999999999556, -7.673322273190748888, 3.656518192455052052 ) ) ;
#29062 = DIRECTION ( 'NONE',  ( 1.000000000000000000, -8.574039729943018344E-17, -0.000000000000000000 ) ) ;
#29063 = DIRECTION ( 'NONE',  ( -1.000000000000000000, 0.000000000000000000, 0.000000000000000000 ) ) ;
#29064 = ORIENTED_EDGE ( 'NONE', *, *, #32934, .F. ) ;
#29065 = LOCAL_TIME ( 16, 7, 10.00000000000000000, #12475 ) ;
#29066 = DIRECTION ( 'NONE',  ( -1.000000000000000000, 0.000000000000000000, 0.000000000000000000 ) ) ;
#29067 = CARTESIAN_POINT ( 'NONE',  ( 25.79765260763087298, 19.02692269782062340, -1.329833256668973229 ) ) ;
#29068 = CARTESIAN_POINT ( 'NONE',  ( 110.5397548702477764, 21.00556809464030650, 2.806473568333438084 ) ) ;
#29070 = ORIENTED_EDGE ( 'NONE', *, *, #24429, .F. ) ;
#29069 = DIRECTION ( 'NONE',  ( 0.000000000000000000, 0.000000000000000000, -1.000000000000000000 ) ) ;
#29071 = CARTESIAN_POINT ( 'NONE',  ( -3.062550801365593323, 3.521866450007987037, 0.3701630799359328372 ) ) ;
#29072 = CARTESIAN_POINT ( 'NONE',  ( 17.32050807568873552, 10.00000000000002309, -1.500000000000000000 ) ) ;
#29073 = CARTESIAN_POINT ( 'NONE',  ( 3.499999999999999556, -1.471047635026823786, -6.892461014225975013 ) ) ;
#29074 = VERTEX_POINT ( 'NONE', #32227 ) ;
#29075 = EDGE_CURVE ( 'NONE', #19878, #19600, #9049, .T. ) ;
#29076 = DIRECTION ( 'NONE',  ( 1.000000000000000000, -0.000000000000000000, -0.000000000000000000 ) ) ;
#29077 = VECTOR ( 'NONE', #23161, 1000.000000000000000 ) ;
#29078 = DIRECTION ( 'NONE',  ( 0.000000000000000000, -0.9961946980917465444, 0.08715574274764703588 ) ) ;
#29079 = PLANE ( 'NONE',  #27726 ) ;
#29080 = EDGE_CURVE ( 'NONE', #13277, #4411, #1959, .T. ) ;
#29081 = DIRECTION ( 'NONE',  ( 0.000000000000000000, -0.5877852522924624790, -0.8090169943749553338 ) ) ;
#29082 = VERTEX_POINT ( 'NONE', #22177 ) ;
#29083 = CARTESIAN_POINT ( 'NONE',  ( 5.489343958331427409, 2.678936089601548165, -7.664144799260921737 ) ) ;
#29084 = CARTESIAN_POINT ( 'NONE',  ( -57.62025439570817298, -2.863290445579637300, 5.500000000000000000 ) ) ;
#29085 = CARTESIAN_POINT ( 'NONE',  ( -3.537550801365593411, -3.368539882008727115, -1.828967928396027842 ) ) ;
#29086 = LINE ( 'NONE', #13825, #4949 ) ;
#29087 = CARTESIAN_POINT ( 'NONE',  ( 0.3076689308762635688, -5.232617538234820564, -8.857103639579413823 ) ) ;
#29088 = ORIENTED_EDGE ( 'NONE', *, *, #4642, .T. ) ;
#29089 = DIRECTION ( 'NONE',  ( -1.000000000000000000, -0.000000000000000000, -0.000000000000000000 ) ) ;
#29090 = ORIENTED_EDGE ( 'NONE', *, *, #13748, .F. ) ;
#29091 = PERSON_AND_ORGANIZATION ( #6766, #25292 ) ;
#29092 = CARTESIAN_POINT ( 'NONE',  ( 9.331062908042635939, 15.00000000000000178, -4.612695725900422872 ) ) ;
#29093 = CIRCLE ( 'NONE', #9319, 8.750000000000000000 ) ;
#29094 = LINE ( 'NONE', #6181, #1265 ) ;
#29095 = ORIENTED_EDGE ( 'NONE', *, *, #3734, .T. ) ;
#29096 = DIRECTION ( 'NONE',  ( 1.000000000000000000, -8.574039729943018344E-17, -0.000000000000000000 ) ) ;
#29097 = EDGE_LOOP ( 'NONE', ( #22413, #16182 ) ) ;
#29098 = VERTEX_POINT ( 'NONE', #17137 ) ;
#29099 = CARTESIAN_POINT ( 'NONE',  ( 17.36028307726380504, -18.11957666779667875, -4.522129901861164925 ) ) ;
#29100 = CARTESIAN_POINT ( 'NONE',  ( -2.912550801365593411, 1.088641768524161613, 3.675193018007246959 ) ) ;
#29101 = CARTESIAN_POINT ( 'NONE',  ( 25.73499999999999943, -0.2613211581691358698, -2.486304738420681559 ) ) ;
#29102 = CARTESIAN_POINT ( 'NONE',  ( 10.00000000000000000, 2.376879293651121383, -4.116875700062057497 ) ) ;
#29104 = VERTEX_POINT ( 'NONE', #32387 ) ;
#29103 = CARTESIAN_POINT ( 'NONE',  ( 6.524595395369783724, 7.902859683906662269, -3.538595500939507144 ) ) ;
#29105 = CARTESIAN_POINT ( 'NONE',  ( -7.037550801365593856, 1.088641768524161613, 3.675193018007247403 ) ) ;
#29106 = CARTESIAN_POINT ( 'NONE',  ( 4.262285728429967575E-16, 4.971152295393310716, -0.6226916219171529931 ) ) ;
#29107 = CARTESIAN_POINT ( 'NONE',  ( 7.580875386713984199, -18.74596882399356446, 1.749278895650158372 ) ) ;
#29108 = DIRECTION ( 'NONE',  ( 1.000000000000000000, 0.000000000000000000, -0.000000000000000000 ) ) ;
#29109 = EDGE_CURVE ( 'NONE', #1745, #8635, #13320, .T. ) ;
#29111 = ORIENTED_EDGE ( 'NONE', *, *, #23019, .F. ) ;
#29110 = DIRECTION ( 'NONE',  ( 0.000000000000000000, -0.9510565162951502005, -0.3090169943749573878 ) ) ;
#29112 = EDGE_CURVE ( 'NONE', #22455, #28961, #15801, .T. ) ;
#29113 = ADVANCED_FACE ( 'NONE', ( #28524 ), #7618, .T. ) ;
#29114 = FACE_OUTER_BOUND ( 'NONE', #4001, .T. ) ;
#29115 = CARTESIAN_POINT ( 'NONE',  ( 21.48500000273118715, 0.2613211581691317065, 2.486304738420681559 ) ) ;
#29116 = CARTESIAN_POINT ( 'NONE',  ( 25.52557118915447987, -17.56218954043521663, 1.000000000000000000 ) ) ;
#29117 = CARTESIAN_POINT ( 'NONE',  ( 18.67456084474389399, -6.814979340958942977, -2.484925321738187698 ) ) ;
#29118 = CARTESIAN_POINT ( 'NONE',  ( -3.686257773765320600, -9.650692365544669471, -1.743566994282037541 ) ) ;
#29119 = DIRECTION ( 'NONE',  ( -0.1327696077594705815, 0.9911469271785068313, 0.000000000000000000 ) ) ;
#29120 = CARTESIAN_POINT ( 'NONE',  ( 9.300322098500100054, 0.2432316347765305364, 1.049936813265543556 ) ) ;
#29121 = CARTESIAN_POINT ( 'NONE',  ( -2.287550801365593856, 2.228590825266444142, 2.752080473201636845 ) ) ;
#29122 = VERTEX_POINT ( 'NONE', #3116 ) ;
#29123 = FACE_OUTER_BOUND ( 'NONE', #257, .T. ) ;
#29124 = CARTESIAN_POINT ( 'NONE',  ( 0.000000000000000000, 0.000000000000000000, 0.000000000000000000 ) ) ;
#29126 = CARTESIAN_POINT ( 'NONE',  ( 5.887530180601100227, -7.449245365665823293, 3.870837198608072072 ) ) ;
#29125 = FACE_OUTER_BOUND ( 'NONE', #19024, .T. ) ;
#29127 = VERTEX_POINT ( 'NONE', #5120 ) ;
#29128 = DIRECTION ( 'NONE',  ( -1.000000000000000000, 0.000000000000000000, -0.000000000000000000 ) ) ;
#29129 = EDGE_LOOP ( 'NONE', ( #23395, #3705, #4519, #29597 ) ) ;
#29130 = CARTESIAN_POINT ( 'NONE',  ( -7.900050800000000706, -2.983565686104819648, -0.3135853898029605791 ) ) ;
#29132 = ORIENTED_EDGE ( 'NONE', *, *, #28094, .T. ) ;
#29131 = CARTESIAN_POINT ( 'NONE',  ( 56.97280603064898941, -277.2763395528616002, 0.000000000000000000 ) ) ;
#29133 = ORIENTED_EDGE ( 'NONE', *, *, #9066, .T. ) ;
#29134 = CARTESIAN_POINT ( 'NONE',  ( -8.000050800000002127, 3.541248556864417196, 0.01107501445590582979 ) ) ;
#29135 = APPLICATION_CONTEXT ( 'configuration controlled 3d designs of mechanical parts and assemblies' ) ;
#29136 = CARTESIAN_POINT ( 'NONE',  ( 22.52203367452234062, -21.86037836540921830, -1.499999999999999556 ) ) ;
#29137 = EDGE_CURVE ( 'NONE', #16174, #12210, #17985, .T. ) ;
#29139 = ORIENTED_EDGE ( 'NONE', *, *, #7336, .F. ) ;
#29138 = CARTESIAN_POINT ( 'NONE',  ( -28.85000000000000497, -10.96966150227469505, 4.000000000000000000 ) ) ;
#29140 = CARTESIAN_POINT ( 'NONE',  ( 9.302055952181039089, 0.2457637073014076190, -1.500000000000000000 ) ) ;
#29141 = DIRECTION ( 'NONE',  ( 0.000000000000000000, 1.000000000000000000, 0.000000000000000000 ) ) ;
#29142 = DIRECTION ( 'NONE',  ( -0.000000000000000000, -0.3746065934159164001, 0.9271838545667856479 ) ) ;
#29143 = CARTESIAN_POINT ( 'NONE',  ( 7.289999265596935452, -8.244573099839797692, -1.499999999999714673 ) ) ;
#29144 = CARTESIAN_POINT ( 'NONE',  ( 107.9778899347920600, -17.75098267791648610, -4.255947362158985392 ) ) ;
#29145 = CARTESIAN_POINT ( 'NONE',  ( -4.562942409646513653, -3.366872799099910998E-15, -3.000000000000000000 ) ) ;
#29146 = CARTESIAN_POINT ( 'NONE',  ( 12.44989959798879831, 18.00000000000000355, 0.3702070605509401036 ) ) ;
#29147 = CARTESIAN_POINT ( 'NONE',  ( 7.249760686538667009, 0.000000000000000000, 0.000000000000000000 ) ) ;
#29148 = CARTESIAN_POINT ( 'NONE',  ( 7.064423637758999952, 8.437262856155495427, 2.318425219013635630 ) ) ;
#29149 = CARTESIAN_POINT ( 'NONE',  ( 0.000000000000000000, -0.1221666339524086348, 6.247805719894683918 ) ) ;
#29150 = ORIENTED_EDGE ( 'NONE', *, *, #25725, .F. ) ;
#29151 = CARTESIAN_POINT ( 'NONE',  ( -6.157304906975411107, -1.062355717592097015, -2.999999999999998668 ) ) ;
#29152 = CARTESIAN_POINT ( 'NONE',  ( -8.000050800000000351, 0.000000000000000000, 0.000000000000000000 ) ) ;
#29153 = FACE_OUTER_BOUND ( 'NONE', #4544, .T. ) ;
#29154 = VERTEX_POINT ( 'NONE', #15296 ) ;
#29155 = CARTESIAN_POINT ( 'NONE',  ( 25.43504868974586941, -2.579632542568791376, -0.8162045923261349589 ) ) ;
#29156 = CARTESIAN_POINT ( 'NONE',  ( 2.274274201625327230, 9.915734732513220351, 4.762163868918306342 ) ) ;
#29157 = VERTEX_POINT ( 'NONE', #5624 ) ;
#29158 = CARTESIAN_POINT ( 'NONE',  ( 5.532756613957264591, -12.77534133546009087, -1.500000000000000666 ) ) ;
#29159 = CARTESIAN_POINT ( 'NONE',  ( -23.35000000000007603, -10.96966150227471459, -12.24999999999999645 ) ) ;
#29160 = ORIENTED_EDGE ( 'NONE', *, *, #4106, .F. ) ;
#29161 = ORIENTED_EDGE ( 'NONE', *, *, #16890, .T. ) ;
#29162 = B_SPLINE_CURVE_WITH_KNOTS ( 'NONE', 3,
 ( #6387, #14392, #32342, #11738, #16585, #26796, #21941, #3917 ),
 .UNSPECIFIED., .F., .F.,
 ( 4, 2, 2, 4 ),
 ( 5.099451029781804389E-07, 0.001229190215587242516, 0.001843530350829372839, 0.002457870486071503380 ),
 .UNSPECIFIED. ) ;
#29163 = CARTESIAN_POINT ( 'NONE',  ( 10.55147673363119054, 4.116875700062082366, 2.376879293651078751 ) ) ;
#29164 = EDGE_CURVE ( 'NONE', #6888, #19163, #13766, .T. ) ;
#29166 = ORIENTED_EDGE ( 'NONE', *, *, #23084, .F. ) ;
#29165 = CARTESIAN_POINT ( 'NONE',  ( 23.17250000000000298, 1.291182301015469047, 2.378061970571981654 ) ) ;
#29167 = VERTEX_POINT ( 'NONE', #25853 ) ;
#29168 = PLANE ( 'NONE',  #19851 ) ;
#29169 = EDGE_LOOP ( 'NONE', ( #10929, #1080, #27389, #16789, #25965, #32447, #25029 ) ) ;
#29170 = CARTESIAN_POINT ( 'NONE',  ( -2.223027892448374399, -2.927336879245633572, 4.522129901861158707 ) ) ;
#29171 = CARTESIAN_POINT ( 'NONE',  ( -5.427698642335591239E-12, -21.93932300456189566, -1.000000000000000000 ) ) ;
#29173 = ORIENTED_EDGE ( 'NONE', *, *, #32319, .F. ) ;
#29172 = CARTESIAN_POINT ( 'NONE',  ( 35.34214449212195319, -3.792788106923375757, -0.07017451552787916380 ) ) ;
#29174 = DIRECTION ( 'NONE',  ( -0.9896144216807899463, 0.000000000000000000, -0.1437473352845038410 ) ) ;
#29175 = CARTESIAN_POINT ( 'NONE',  ( 5.489321289187125252, -0.1038943573682082760, 8.118169347437836691 ) ) ;
#29176 = EDGE_CURVE ( 'NONE', #14830, #8629, #17602, .T. ) ;
#29177 = CARTESIAN_POINT ( 'NONE',  ( -56.61259478326383743, 0.1231456938264295642, 1.516656275171373469 ) ) ;
#29178 = EDGE_CURVE ( 'NONE', #4283, #28828, #29883, .T. ) ;
#29179 = CARTESIAN_POINT ( 'NONE',  ( 2.592584839944457986, 5.238191131136629153, -8.898511132916340216 ) ) ;
#29180 = CARTESIAN_POINT ( 'NONE',  ( 108.0285047196611430, -18.47982298865751005, 4.352162063355596189 ) ) ;
#29181 = CARTESIAN_POINT ( 'NONE',  ( -2.613459990200682537, -0.04407919770141072169, -1.513648816985697199 ) ) ;
#29182 = CARTESIAN_POINT ( 'NONE',  ( 23.61515526891511740, -8.000136145882661864, -0.8105616806143508546 ) ) ;
#29183 = LINE ( 'NONE', #24161, #9294 ) ;
#29184 = EDGE_CURVE ( 'NONE', #20812, #2621, #1426, .T. ) ;
#29185 = DIRECTION ( 'NONE',  ( 0.1767573132311711093, 0.9842544651762052954, 0.000000000000000000 ) ) ;
#29186 = CARTESIAN_POINT ( 'NONE',  ( 23.25968157276533788, -21.94039639456149970, 1.058068383262721790 ) ) ;
#29187 = CARTESIAN_POINT ( 'NONE',  ( 0.000000000000000000, 0.000000000000000000, 1.500000000000000000 ) ) ;
#29188 = CARTESIAN_POINT ( 'NONE',  ( 10.00000000000000000, -2.376879293651094294, 4.116875700062075261 ) ) ;
#29189 = DIRECTION ( 'NONE',  ( -1.000000000000000000, 0.000000000000000000, 0.000000000000000000 ) ) ;
#29190 = CARTESIAN_POINT ( 'NONE',  ( -7.500050802731188071, 2.853674364686379583, 1.549418761218565921 ) ) ;
#29191 = EDGE_LOOP ( 'NONE', ( #13387, #27961, #705, #7669 ) ) ;
#29192 = ADVANCED_FACE ( 'NONE', ( #20813 ), #30872, .T. ) ;
#29193 = CARTESIAN_POINT ( 'NONE',  ( -7.800050800000000173, -1.887961173149512062, -2.331437884370912261 ) ) ;
#29194 = CARTESIAN_POINT ( 'NONE',  ( 107.7140348563909669, -17.39211855127401307, 4.500745083103332433 ) ) ;
#29195 = CARTESIAN_POINT ( 'NONE',  ( -8.125050801365594211, 0.3701630799359330593, -3.521866450007987037 ) ) ;
#29196 = FACE_OUTER_BOUND ( 'NONE', #5833, .T. ) ;
#29197 = EDGE_LOOP ( 'NONE', ( #23057, #12734, #5770, #14024, #12095 ) ) ;
#29198 = CARTESIAN_POINT ( 'NONE',  ( 6.910673634762011908, -8.774004714863222532, -1.500000000000000444 ) ) ;
#29199 = ORIENTED_EDGE ( 'NONE', *, *, #11023, .T. ) ;
#29200 = CARTESIAN_POINT ( 'NONE',  ( 0.1308125268056005985, -6.172912210551425360, 1.772480729299952928 ) ) ;
#29201 = COORDINATED_UNIVERSAL_TIME_OFFSET ( 0, 0, .AHEAD. ) ;
#29202 = EDGE_LOOP ( 'NONE', ( #6489, #996 ) ) ;
#29203 = CARTESIAN_POINT ( 'NONE',  ( 40.88087200079529282, -6.322651088349340753, 4.312042181584448741 ) ) ;
#29204 = DIRECTION ( 'NONE',  ( 0.000000000000000000, 1.000000000000000000, 0.000000000000000000 ) ) ;
#29205 = CARTESIAN_POINT ( 'NONE',  ( 18.85216891279196361, -4.829677595303946802, -4.112224495641408240 ) ) ;
#29206 = CARTESIAN_POINT ( 'NONE',  ( 23.30969226767547298, -17.20274083179951674, -1.451821733976820239 ) ) ;
#29207 = CARTESIAN_POINT ( 'NONE',  ( 2.661997850953048417, 5.196702353893204673, 8.696442646092039652 ) ) ;
#29208 = VERTEX_POINT ( 'NONE', #15140 ) ;
#29209 = EDGE_CURVE ( 'NONE', #8190, #19301, #25347, .T. ) ;
#29210 = CYLINDRICAL_SURFACE ( 'NONE', #16749, 296.4345239564032681 ) ;
#29211 = EDGE_CURVE ( 'NONE', #14221, #27844, #6208, .T. ) ;
#29212 = CARTESIAN_POINT ( 'NONE',  ( 0.5704035821693393959, 9.519055809315281280, -0.6538686328479882404 ) ) ;
#29213 = DIRECTION ( 'NONE',  ( 0.000000000000000000, 0.000000000000000000, 1.000000000000000000 ) ) ;
#29215 = ORIENTED_EDGE ( 'NONE', *, *, #19047, .T. ) ;
#29214 = DIRECTION ( 'NONE',  ( 0.000000000000000000, -0.03489949670250130920, -0.9993908270190957621 ) ) ;
#29216 = DIRECTION ( 'NONE',  ( 0.1290991311231024230, 0.9916316928896837801, 0.000000000000000000 ) ) ;
#29217 = B_SPLINE_CURVE_WITH_KNOTS ( 'NONE', 3,
 ( #1850, #9495, #31930, #12028, #8996, #19888, #2155, #19210, #6500, #26913 ),
 .UNSPECIFIED., .F., .F.,
 ( 4, 2, 2, 2, 4 ),
 ( 1.968338519004493228E-07, 0.0005467926395225673275, 0.001093388445193233666, 0.001639984250863899895, 0.002186580056534566125 ),
 .UNSPECIFIED. ) ;
#29218 = B_SPLINE_SURFACE_WITH_KNOTS ( 'NONE', 3, 3, ( 
 ( #21186, #30619, #25061, #15029, #25417, #15364, #12543 ),
 ( #25570, #28702, #12849, #2525, #7857, #20579, #12365 ),
 ( #30279, #7512, #13471, #30432, #806, #25248, #10369 ),
 ( #22584, #2370, #22747, #20233, #6642, #18508, #32953 ) ),
 .UNSPECIFIED., .F., .F., .F.,
 ( 4, 4 ),
 ( 4, 3, 4 ),
 ( -7.485815332815247898E-12, 1.000000000000005551 ),
 ( 0.003594141869010686677, 0.5017970709347674418, 1.000000000000524247 ),
 .UNSPECIFIED. ) ;
#29219 = DIRECTION ( 'NONE',  ( 0.000000000000000000, 0.000000000000000000, -1.000000000000000000 ) ) ;
#29220 = CARTESIAN_POINT ( 'NONE',  ( 2.976845726615121368, -2.305279507610546119, -8.871766062375181505 ) ) ;
#29221 = DIRECTION ( 'NONE',  ( 0.8660254037844409281, -0.4999999999999960587, 0.000000000000000000 ) ) ;
#29222 = CARTESIAN_POINT ( 'NONE',  ( 7.249760686538667009, 7.530955069117551304, -2.741043480754851380 ) ) ;
#29223 = DIRECTION ( 'NONE',  ( 0.000000000000000000, 1.000000000000000000, 0.000000000000000000 ) ) ;
#29224 = DIRECTION ( 'NONE',  ( 0.000000000000000000, -1.000000000000000000, 0.000000000000000000 ) ) ;
#29225 = CARTESIAN_POINT ( 'NONE',  ( 17.97422212135272801, -19.86246923125032637, 4.522129901861159595 ) ) ;
#29226 = VERTEX_POINT ( 'NONE', #286 ) ;
#29227 = CARTESIAN_POINT ( 'NONE',  ( 0.000000000000000000, 4.057423117305515525, -8.475820894092930047 ) ) ;
#29228 = ORIENTED_EDGE ( 'NONE', *, *, #5481, .F. ) ;
#29229 = EDGE_CURVE ( 'NONE', #29021, #21819, #1054, .T. ) ;
#29230 = PLANE ( 'NONE',  #29503 ) ;
#29231 = APPROVAL ( #6442, 'UNSPECIFIED' ) ;
#29232 = CARTESIAN_POINT ( 'NONE',  ( -2.019764013714869577, 0.9872008099554112626, 3.231313631359007399 ) ) ;
#29233 =( BOUNDED_CURVE ( )  B_SPLINE_CURVE ( 2, ( #7154, #30560, #27863, #9819, #7302, #5141, #30891, #9974, #25369, #2807, #10477 ),
 .UNSPECIFIED., .F., .F. ) 
 B_SPLINE_CURVE_WITH_KNOTS ( ( 3, 2, 2, 2, 2, 3 ),
 ( 0.7966116191895004084, 0.8000000000000000444, 0.8249999999999999556, 0.8499999999999999778, 0.8750000000000000000, 0.8966116191895003862 ),
 .UNSPECIFIED. ) 
 CURVE ( )  GEOMETRIC_REPRESENTATION_ITEM ( )  RATIONAL_B_SPLINE_CURVE ( ( 0.9821626249036858880, 0.9896829947469992783, 1.000000000000000000, 0.9238795325112867385, 1.000000000000000000, 0.9238795325112867385, 1.000000000000000000, 0.9238795325112867385, 1.000000000000000000, 0.9341965377642874602, 0.9821626249036858880 ) ) 
 REPRESENTATION_ITEM ( '' )  );
#29234 = CARTESIAN_POINT ( 'NONE',  ( -2.687550801365593323, -2.228590825266444586, -2.752080473201636401 ) ) ;
#29235 = CARTESIAN_POINT ( 'NONE',  ( 3.660726896358641902, 3.599890025830775825E-17, -1.077884872112069292 ) ) ;
#29236 = CARTESIAN_POINT ( 'NONE',  ( 29.20401286873546809, -7.702374816464193863, 2.184956341613425224 ) ) ;
#29237 = ORIENTED_EDGE ( 'NONE', *, *, #26540, .T. ) ;
#29238 = CARTESIAN_POINT ( 'NONE',  ( 107.1769020805352142, 16.40214705320006061, -1.491740999229420161 ) ) ;
#29239 = ORIENTED_EDGE ( 'NONE', *, *, #8798, .T. ) ;
#29240 = PERSON_AND_ORGANIZATION_ROLE ( 'creator' ) ;
#29241 = B_SPLINE_CURVE_WITH_KNOTS ( 'NONE', 3,
 ( #22180, #30212, #9611, #17141, #24995, #12474, #14646, #32888, #20168, #4960 ),
 .UNSPECIFIED., .F., .F.,
 ( 4, 2, 2, 2, 4 ),
 ( 0.000000000000000000, 0.0003410365069687240733, 0.0006820730139374481466, 0.001023109520906172274, 0.001364146027874896293 ),
 .UNSPECIFIED. ) ;
#29242 = CARTESIAN_POINT ( 'NONE',  ( 102.4231811201833438, -3.998190225786205421, 3.995970699063716491 ) ) ;
#29243 = EDGE_CURVE ( 'NONE', #29157, #5623, #23990, .T. ) ;
#29244 = CARTESIAN_POINT ( 'NONE',  ( 7.177184080414120260, -7.491031434833116620, -1.000000000000000000 ) ) ;
#29245 = EDGE_LOOP ( 'NONE', ( #31687, #20502, #12749, #23105, #10195, #15422, #11686, #23801, #9074, #20806, #14854, #31567 ) ) ;
#29246 = DIRECTION ( 'NONE',  ( 0.000000000000000000, 0.000000000000000000, 1.000000000000000000 ) ) ;
#29247 = ORIENTED_EDGE ( 'NONE', *, *, #26530, .T. ) ;
#29248 = EDGE_LOOP ( 'NONE', ( #32217, #1930, #24568, #14639 ) ) ;
#29249 = DIRECTION ( 'NONE',  ( -1.000000000000000000, 0.000000000000000000, -0.000000000000000000 ) ) ;
#29250 = CARTESIAN_POINT ( 'NONE',  ( -4.962550801365593678, -2.228590825266444586, -2.752080473201636401 ) ) ;
#29251 = CARTESIAN_POINT ( 'NONE',  ( 25.48499999999999943, -2.486304738420683780, 0.2613211581691335383 ) ) ;
#29252 = PLANE ( 'NONE',  #27857 ) ;
#29254 = EDGE_LOOP ( 'NONE', ( #32008, #8762, #29199 ) ) ;
#29253 = CARTESIAN_POINT ( 'NONE',  ( -10.00000000000000000, 0.000000000000000000, 0.000000000000000000 ) ) ;
#29255 = CARTESIAN_POINT ( 'NONE',  ( -5.937550801365592434, -3.368539882008727115, -1.828967928396028064 ) ) ;
#29256 = CARTESIAN_POINT ( 'NONE',  ( 19.82965097529934084, 15.28209255204611594, 1.049999999999883027 ) ) ;
#29257 = CARTESIAN_POINT ( 'NONE',  ( 6.357667697713668353, 2.056386458247386528, -8.357963647880058744 ) ) ;
#29258 = DIRECTION ( 'NONE',  ( 0.000000000000000000, 0.000000000000000000, -1.000000000000000000 ) ) ;
#29259 = ORIENTED_EDGE ( 'NONE', *, *, #14033, .T. ) ;
#29261 = ORIENTED_EDGE ( 'NONE', *, *, #30008, .F. ) ;
#29260 = DIRECTION ( 'NONE',  ( 0.000000000000000000, 0.08715574274765541807, -0.9961946980917457672 ) ) ;
#29262 = CARTESIAN_POINT ( 'NONE',  ( 21.17250000273118715, 2.378061970571979433, -1.291182301015470824 ) ) ;
#29263 = LINE ( 'NONE', #31453, #1199 ) ;
#29264 = CARTESIAN_POINT ( 'NONE',  ( 18.69120935168668041, -6.628882446443490117, -2.784893864646371231 ) ) ;
#29265 = CARTESIAN_POINT ( 'NONE',  ( -3.910356079379007088, -9.341596471033172477, -1.500000000000000000 ) ) ;
#29266 = CARTESIAN_POINT ( 'NONE',  ( 10.00000000000000000, 4.116875700062082366, 2.376879293651078751 ) ) ;
#29267 = CARTESIAN_POINT ( 'NONE',  ( 7.249760686538667009, -6.139290821770219786, -5.151476664237539360 ) ) ;
#29268 = CARTESIAN_POINT ( 'NONE',  ( -2.787550801365593411, -3.521866450007987037, -0.3701630799359323931 ) ) ;
#29269 = ORIENTED_EDGE ( 'NONE', *, *, #24835, .T. ) ;
#29270 = CARTESIAN_POINT ( 'NONE',  ( 20.53274989849606769, -21.72776571847631999, 1.408906953170992127 ) ) ;
#29271 = CARTESIAN_POINT ( 'NONE',  ( 0.000000000000000000, 1.418488851014487073, -6.085876303339362359 ) ) ;
#29273 = CARTESIAN_POINT ( 'NONE',  ( 7.064632940817598517, -7.906491560603691404, 3.748318449932268148 ) ) ;
#29272 = CARTESIAN_POINT ( 'NONE',  ( 3.249999999999999556, -6.772677083992345359, -5.538577986808975062 ) ) ;
#29274 = ADVANCED_FACE ( 'NONE', ( #26640 ), #26496, .T. ) ;
#29275 = VERTEX_POINT ( 'NONE', #26161 ) ;
#29276 = EDGE_CURVE ( 'NONE', #8881, #22866, #13426, .T. ) ;
#29277 = B_SPLINE_CURVE_WITH_KNOTS ( 'NONE', 3,
 ( #310, #2995, #28199, #10322, #10805, #22855, #5646, #13148, #25691, #29325, #5933, #19134, #4102, #938, #6605, #10968 ),
 .UNSPECIFIED., .F., .F.,
 ( 4, 2, 2, 2, 2, 2, 2, 4 ),
 ( 0.000000000000000000, 3.093269050410396288E-05, 6.186538100820792576E-05, 0.0001237307620164256093, 0.0002474615240328612476, 0.0004949230480657320361, 0.0009898460961314727458, 0.001979692192262965007 ),
 .UNSPECIFIED. ) ;
#29278 = CARTESIAN_POINT ( 'NONE',  ( 2.274274201627289216, 9.680994141364161365, 5.222868219167314585 ) ) ;
#29279 = ORIENTED_EDGE ( 'NONE', *, *, #20687, .F. ) ;
#29280 = CARTESIAN_POINT ( 'NONE',  ( 0.7632845268451443621, 5.538577986791731078, -6.772677083973650092 ) ) ;
#29281 = EDGE_CURVE ( 'NONE', #24417, #901, #5457, .T. ) ;
#29283 = ORIENTED_EDGE ( 'NONE', *, *, #13463, .T. ) ;
#29282 = CARTESIAN_POINT ( 'NONE',  ( 54.94553969879451927, -5.361749600163809859, -3.997238534717083347 ) ) ;
#29284 = EDGE_LOOP ( 'NONE', ( #12513, #18516, #25314, #21426 ) ) ;
#29285 = LINE ( 'NONE', #17200, #26273 ) ;
#29286 = CARTESIAN_POINT ( 'NONE',  ( 0.000000000000000000, -7.958834565716711218, -7.593217523260666901 ) ) ;
#29288 = ORIENTED_EDGE ( 'NONE', *, *, #22169, .T. ) ;
#29287 = CARTESIAN_POINT ( 'NONE',  ( 25.75999999999999801, 2.805042440084548172, 1.132414195126726364 ) ) ;
#29289 = CARTESIAN_POINT ( 'NONE',  ( 17.54326037877522637, 13.05023557613625584, -1.050000000000000044 ) ) ;
#29290 = CARTESIAN_POINT ( 'NONE',  ( -4.062288539342293170, -5.105566185483802144, -1.745843300479905436 ) ) ;
#29291 = DIRECTION ( 'NONE',  ( 0.9947025833170223263, 0.1027947991993880261, 0.000000000000000000 ) ) ;
#29292 = CARTESIAN_POINT ( 'NONE',  ( 13.85437446117461491, -14.51384729145977204, -1.499999999999999334 ) ) ;
#29294 = ORIENTED_EDGE ( 'NONE', *, *, #7742, .F. ) ;
#29293 = CARTESIAN_POINT ( 'NONE',  ( 107.8806307222008627, -16.35047421165092985, -1.384330804613826293 ) ) ;
#29295 = CARTESIAN_POINT ( 'NONE',  ( 18.58227844715246135, -7.846511338401735536, -2.713652344655542947 ) ) ;
#29296 = CARTESIAN_POINT ( 'NONE',  ( -7.000050800000000351, 7.347880794884120722E-16, 6.000000000000000888 ) ) ;
#29297 = CARTESIAN_POINT ( 'NONE',  ( 47.93076651534872923, -6.701564465771713941, 3.993434086975188979 ) ) ;
#29298 = DESIGN_CONTEXT ( 'detailed design', #15890, 'design' ) ;
#29299 = CARTESIAN_POINT ( 'NONE',  ( 6.448894291894883501, -17.04229596238074507, 4.522129901861158707 ) ) ;
#29300 = CARTESIAN_POINT ( 'NONE',  ( 2.382865613620175349, 0.000000000000000000, 1.508259000770581615 ) ) ;
#29301 = ORIENTED_EDGE ( 'NONE', *, *, #12943, .T. ) ;
#29302 = CARTESIAN_POINT ( 'NONE',  ( 3.250000000000001332, 0.000000000000000000, 0.000000000000000000 ) ) ;
#29303 = FACE_OUTER_BOUND ( 'NONE', #25622, .T. ) ;
#29304 = CARTESIAN_POINT ( 'NONE',  ( 4.749760686538667009, 1.391664247347228045, 7.892520144992438702 ) ) ;
#29305 = ORIENTED_EDGE ( 'NONE', *, *, #17371, .F. ) ;
#29306 = CARTESIAN_POINT ( 'NONE',  ( 25.23500000000000654, 2.486304733690583912, -0.2613212031729839624 ) ) ;
#29307 = CARTESIAN_POINT ( 'NONE',  ( 10.00000000000000000, -4.884328206559844787, 1.115095498423292364 ) ) ;
#29308 = ORIENTED_EDGE ( 'NONE', *, *, #25703, .F. ) ;
#29309 = DIRECTION ( 'NONE',  ( -0.9164966213036979115, 0.4000424266736042900, 0.000000000000000000 ) ) ;
#29310 = EDGE_CURVE ( 'NONE', #22866, #25302, #27860, .T. ) ;
#29311 = EDGE_LOOP ( 'NONE', ( #852, #27797, #29805, #3290 ) ) ;
#29312 = ADVANCED_FACE ( 'NONE', ( #11443 ), #6400, .F. ) ;
#29313 = VERTEX_POINT ( 'NONE', #11593 ) ;
#29314 = CARTESIAN_POINT ( 'NONE',  ( 85.13613392229179055, -2.069934983084471103, -2.713652344655540727 ) ) ;
#29315 = DATE_TIME_ROLE ( 'classification_date' ) ;
#29317 = ORIENTED_EDGE ( 'NONE', *, *, #29431, .F. ) ;
#29316 = CARTESIAN_POINT ( 'NONE',  ( 5.887529755120530339, -8.323904922804405970, 1.089605374054344544 ) ) ;
#29318 = ORIENTED_EDGE ( 'NONE', *, *, #12541, .T. ) ;
#29319 = CARTESIAN_POINT ( 'NONE',  ( 25.29750000136559507, -0.3178988483021076838, -3.024605502323848949 ) ) ;
#29320 = ORIENTED_EDGE ( 'NONE', *, *, #2480, .F. ) ;
#29321 = CARTESIAN_POINT ( 'NONE',  ( 12.44989959798868817, 18.00000000000000355, 13.00000000000004441 ) ) ;
#29322 = CARTESIAN_POINT ( 'NONE',  ( 13.62547635268498780, 21.94000000000002970, 1.500000000000000000 ) ) ;
#29324 = ORIENTED_EDGE ( 'NONE', *, *, #10873, .F. ) ;
#29323 = CARTESIAN_POINT ( 'NONE',  ( 54.89716490669064797, -3.628845007888692020, -0.07017451552781811541 ) ) ;
#29325 = CARTESIAN_POINT ( 'NONE',  ( 22.93781638691914182, -21.92296000134991729, 1.128554389308254136 ) ) ;
#29326 = LINE ( 'NONE', #29023, #22939 ) ;
#29327 = CARTESIAN_POINT ( 'NONE',  ( 101.8146265438530520, -4.229152002780746322, 3.693462844207877627 ) ) ;
#29328 = CARTESIAN_POINT ( 'NONE',  ( 6.038145268433179780, 5.096160642893651449, 6.771555838910872538 ) ) ;
#29329 = CARTESIAN_POINT ( 'NONE',  ( 108.0605219787248643, -18.94086355428285984, 4.544875792429381889 ) ) ;
#29330 = CIRCLE ( 'NONE', #25592, 0.5000000000000000000 ) ;
#29331 = CARTESIAN_POINT ( 'NONE',  ( -0.9232102171129827894, 0.000000000000000000, -4.522129901861166701 ) ) ;
#29332 = CARTESIAN_POINT ( 'NONE',  ( 0.7632845268398871230, 0.000000000000000000, 0.000000000000000000 ) ) ;
#29333 = LINE ( 'NONE', #6769, #17859 ) ;
#29334 = CARTESIAN_POINT ( 'NONE',  ( 2.593512329575641137E-16, 3.024842911000690471, 3.993798362933319357 ) ) ;
#29335 = CARTESIAN_POINT ( 'NONE',  ( 0.04279322307214343535, 9.518551034997546623, 5.235773223809417232 ) ) ;
#29336 = DIRECTION ( 'NONE',  ( 0.000000000000000000, -0.9659258262890720870, 0.2588190451025066952 ) ) ;
#29337 = EDGE_CURVE ( 'NONE', #22172, #25587, #9834, .T. ) ;
#29338 = DIRECTION ( 'NONE',  ( 1.000000000000000000, -8.574039729943018344E-17, -0.000000000000000000 ) ) ;
#29339 = CARTESIAN_POINT ( 'NONE',  ( -4.550050802731187005, 0.3135853898029611342, -2.983565686104819648 ) ) ;
#29340 = VERTEX_POINT ( 'NONE', #32181 ) ;
#29341 = CARTESIAN_POINT ( 'NONE',  ( -7.850050800000000883, -2.853674364686378695, -1.549418761218566809 ) ) ;
#29342 = CIRCLE ( 'NONE', #21872, 6.248999999999999666 ) ;
#29343 = EDGE_CURVE ( 'NONE', #31349, #11409, #29492, .T. ) ;
#29344 = CIRCLE ( 'NONE', #1055, 4.000000000000001776 ) ;
#29345 = CARTESIAN_POINT ( 'NONE',  ( -29.34654203815345141, 5.078599898679035718, 1.213362788697829542 ) ) ;
#29346 = CARTESIAN_POINT ( 'NONE',  ( 0.000000000000000000, 0.000000000000000000, 0.000000000000000000 ) ) ;
#29347 = CARTESIAN_POINT ( 'NONE',  ( -40.96618937992463572, -13.73263466181244041, 5.759795317147328397 ) ) ;
#29348 = VERTEX_POINT ( 'NONE', #19975 ) ;
#29349 = CARTESIAN_POINT ( 'NONE',  ( 7.565496255526688252, -10.23852490753150768, -1.499999999999999778 ) ) ;
#29350 = EDGE_CURVE ( 'NONE', #2361, #4711, #22294, .T. ) ;
#29351 = AXIS2_PLACEMENT_3D ( 'NONE', #19645, #13932, #11770 ) ;
#29352 = VERTEX_POINT ( 'NONE', #17288 ) ;
#29353 = CARTESIAN_POINT ( 'NONE',  ( 0.3239945992768507033, -5.503618096412950855, 1.499999999999858558 ) ) ;
#29354 = DATE_TIME_ROLE ( 'classification_date' ) ;
#29356 = EDGE_CURVE ( 'NONE', #7768, #1159, #4587, .T. ) ;
#29355 = DIRECTION ( 'NONE',  ( -1.000000000000000000, 0.000000000000000000, 0.000000000000000000 ) ) ;
#29357 = VERTEX_POINT ( 'NONE', #29667 ) ;
#29358 = CARTESIAN_POINT ( 'NONE',  ( 40.87800967743321934, -5.799281926994868996, 4.074609548159814132 ) ) ;
#29359 = DIRECTION ( 'NONE',  ( 0.000000000000000000, 1.000000000000000000, 0.000000000000000000 ) ) ;
#29360 = CARTESIAN_POINT ( 'NONE',  ( 40.87796467563064340, -5.791092821954919145, -4.053847216751194971 ) ) ;
#29361 = CARTESIAN_POINT ( 'NONE',  ( 3.499999999999999556, 6.226349476952025341, -0.5315761383463578627 ) ) ;
#29362 = CARTESIAN_POINT ( 'NONE',  ( 10.90258948330155953, 17.51112508050605854, 4.629213727441584325 ) ) ;
#29363 = EDGE_LOOP ( 'NONE', ( #12911, #5495 ) ) ;
#29364 = EDGE_CURVE ( 'NONE', #12752, #24872, #32145, .T. ) ;
#29365 = CARTESIAN_POINT ( 'NONE',  ( 23.12748570787497826, -21.92617700502155387, -1.175810055043982061 ) ) ;
#29366 = DIRECTION ( 'NONE',  ( -0.000000000000000000, -0.000000000000000000, -1.000000000000000000 ) ) ;
#29367 = CARTESIAN_POINT ( 'NONE',  ( 2.589203020517539144, -5.222514179739437878, -8.895471158038722237 ) ) ;
#29368 = AXIS2_PLACEMENT_3D ( 'NONE', #26920, #11685, #10165 ) ;
#29370 = ORIENTED_EDGE ( 'NONE', *, *, #15284, .T. ) ;
#29369 = CARTESIAN_POINT ( 'NONE',  ( -14.51685907258683983, -28.43932300454937590, -1.000000000000000000 ) ) ;
#29371 = CARTESIAN_POINT ( 'NONE',  ( 25.82046699000660439, 24.17190842697641529, 2.806473568333438084 ) ) ;
#29372 = TOROIDAL_SURFACE ( 'NONE', #3218, 10.43371088333261731, 0.4500000000000000111 ) ;
#29373 = CARTESIAN_POINT ( 'NONE',  ( 3.499999999999999556, -2.834406817834963732, 8.013497238472769624 ) ) ;
#29374 = DIRECTION ( 'NONE',  ( 0.000000000000000000, 0.000000000000000000, 1.000000000000000000 ) ) ;
#29375 = FACE_OUTER_BOUND ( 'NONE', #8360, .T. ) ;
#29376 = CARTESIAN_POINT ( 'NONE',  ( 107.2615523761464260, 16.89492944954590214, 0.000000000000000000 ) ) ;
#29377 = ADVANCED_FACE ( 'NONE', ( #27303 ), #10059, .T. ) ;
#29378 = AXIS2_PLACEMENT_3D ( 'NONE', #17493, #15164, #14972 ) ;
#29379 = CYLINDRICAL_SURFACE ( 'NONE', #8651, 4.000000000000001776 ) ;
#29380 = CARTESIAN_POINT ( 'NONE',  ( 2.274274201625327230, -9.915734732513254102, 4.762163868918234400 ) ) ;
#29381 = PLANE ( 'NONE',  #27902 ) ;
#29382 = CARTESIAN_POINT ( 'NONE',  ( 42.67399297346871379, -22.27808837059998481, 5.485967528433935314 ) ) ;
#29383 = VERTEX_POINT ( 'NONE', #7082 ) ;
#29384 = ADVANCED_FACE ( 'NONE', ( #22453 ), #22643, .F. ) ;
#29385 = CARTESIAN_POINT ( 'NONE',  ( 20.50111451137534857, -3.256483526998273983E-15, 2.499999999999998668 ) ) ;
#29386 = ORIENTED_EDGE ( 'NONE', *, *, #5346, .F. ) ;
#29387 = CARTESIAN_POINT ( 'NONE',  ( 6.880159540721329847, 2.328896285337303418, -8.414807581959433236 ) ) ;
#29388 = CARTESIAN_POINT ( 'NONE',  ( -1.867022907593409276, 0.3751246966288243057, 3.134367353446092963 ) ) ;
#29389 = VECTOR ( 'NONE', #10047, 1000.000000000000000 ) ;
#29390 = CARTESIAN_POINT ( 'NONE',  ( -4.437550801365594211, -3.675193018007245627, 1.088641768524163389 ) ) ;
#29391 = EDGE_CURVE ( 'NONE', #8063, #681, #24450, .T. ) ;
#29392 = AXIS2_PLACEMENT_3D ( 'NONE', #29404, #19207, #32091 ) ;
#29393 = DIRECTION ( 'NONE',  ( 0.9816271834476644198, 0.000000000000000000, 0.1908089953765420288 ) ) ;
#29394 = FACE_OUTER_BOUND ( 'NONE', #1377, .T. ) ;
#29395 = ORIENTED_EDGE ( 'NONE', *, *, #20606, .F. ) ;
#29396 = CARTESIAN_POINT ( 'NONE',  ( -31.63092319849839029, -25.68921844201284088, 1.340913934978428035 ) ) ;
#29397 = EDGE_CURVE ( 'NONE', #15831, #4708, #9750, .T. ) ;
#29398 = AXIS2_PLACEMENT_3D ( 'NONE', #2399, #23104, #20264 ) ;
#29399 = ORIENTED_EDGE ( 'NONE', *, *, #19584, .T. ) ;
#29400 = PERSON_AND_ORGANIZATION_ROLE ( 'classification_officer' ) ;
#29401 = CARTESIAN_POINT ( 'NONE',  ( 26.27358061090003361, 19.78731608622335969, -0.4463807625373608645 ) ) ;
#29402 = EDGE_CURVE ( 'NONE', #29122, #19723, #20926, .T. ) ;
#29403 = VECTOR ( 'NONE', #28640, 1000.000000000000000 ) ;
#29404 = CARTESIAN_POINT ( 'NONE',  ( 34.48223484310469900, 0.5000000000000000000, 2.482234843104950350 ) ) ;
#29405 = ORIENTED_EDGE ( 'NONE', *, *, #22049, .F. ) ;
#29406 = CARTESIAN_POINT ( 'NONE',  ( 6.880159329304570193, 6.224287131858889488, -6.122988934091214475 ) ) ;
#29407 = ORIENTED_EDGE ( 'NONE', *, *, #4642, .F. ) ;
#29408 = ORIENTED_EDGE ( 'NONE', *, *, #29178, .T. ) ;
#29409 = CARTESIAN_POINT ( 'NONE',  ( 0.3749743548326617271, -0.8908839545093775181, -10.05686762493553310 ) ) ;
#29410 = CARTESIAN_POINT ( 'NONE',  ( 2.795120610031291530, 9.728666380680506265, -0.7443816538168457342 ) ) ;
#29411 = CARTESIAN_POINT ( 'NONE',  ( 25.04750000000000298, 2.594547506269380133, 0.7685399846772031918 ) ) ;
#29412 = EDGE_CURVE ( 'NONE', #28440, #21586, #16864, .T. ) ;
#29413 = CARTESIAN_POINT ( 'NONE',  ( -23.35000000000000142, -10.96966150227469505, -11.00000000000000000 ) ) ;
#29415 = ORIENTED_EDGE ( 'NONE', *, *, #17322, .F. ) ;
#29414 = DIRECTION ( 'NONE',  ( 0.000000000000000000, 0.000000000000000000, 1.000000000000000000 ) ) ;
#29416 = CARTESIAN_POINT ( 'NONE',  ( -8.037550801365592079, 3.675193018007247403, -1.088641768524161391 ) ) ;
#29417 = CARTESIAN_POINT ( 'NONE',  ( -8.000050800000000351, 0.000000000000000000, 0.000000000000000000 ) ) ;
#29418 = CIRCLE ( 'NONE', #24604, 5.000000000000001776 ) ;
#29419 = CARTESIAN_POINT ( 'NONE',  ( 5.887529755120530339, 1.823049025159297232, -8.194579018285272909 ) ) ;
#29420 = DIRECTION ( 'NONE',  ( 0.1587661886298589176, 0.9873162094020071500, 0.000000000000000000 ) ) ;
#29421 = AXIS2_PLACEMENT_3D ( 'NONE', #297, #20680, #30883 ) ;
#29422 = ORIENTED_EDGE ( 'NONE', *, *, #3986, .F. ) ;
#29424 = VERTEX_POINT ( 'NONE', #12910 ) ;
#29423 = FACE_OUTER_BOUND ( 'NONE', #21213, .T. ) ;
#29425 = VECTOR ( 'NONE', #11542, 1000.000000000000000 ) ;
#29426 = VECTOR ( 'NONE', #21848, 1000.000000000000000 ) ;
#29428 = VECTOR ( 'NONE', #19844, 1000.000000000000000 ) ;
#29427 = CYLINDRICAL_SURFACE ( 'NONE', #23028, 4.000000000000001776 ) ;
#29429 =( BOUNDED_CURVE ( )  B_SPLINE_CURVE ( 2, ( #21847, #29727, #6805, #32062, #4302, #6652, #19364, #1979, #9975, #28194, #20185 ),
 .UNSPECIFIED., .F., .F. ) 
 B_SPLINE_CURVE_WITH_KNOTS ( ( 3, 2, 2, 2, 2, 3 ),
 ( 0.4978822619934377136, 0.5000000000000000000, 0.5156250000000000000, 0.5312500000000000000, 0.5468750000000000000, 0.5603822619934377691 ),
 .UNSPECIFIED. ) 
 CURVE ( )  GEOMETRIC_REPRESENTATION_ITEM ( )  RATIONAL_B_SPLINE_CURVE ( ( 0.9821626249036857770, 0.9896829947469991673, 1.000000000000000000, 0.9238795325112867385, 1.000000000000000000, 0.9238795325112867385, 1.000000000000000000, 0.9238795325112867385, 1.000000000000000000, 0.9341965377642872381, 0.9821626249036861100 ) ) 
 REPRESENTATION_ITEM ( '' )  );
#29430 = CARTESIAN_POINT ( 'NONE',  ( 21.42250000273118715, 1.291182301015469047, 2.378061970571981654 ) ) ;
#29431 = EDGE_CURVE ( 'NONE', #14007, #4750, #640, .T. ) ;
#29432 = CARTESIAN_POINT ( 'NONE',  ( 12.44989959798879831, 0.000000000000000000, 0.9987809114024006618 ) ) ;
#29433 = CARTESIAN_POINT ( 'NONE',  ( -24.43722099606875275, 18.60133783399176011, 1.500000000000506040 ) ) ;
#29434 = CARTESIAN_POINT ( 'NONE',  ( -23.35000000000000142, -10.96966150227469505, -11.50000000000000000 ) ) ;
#29435 = CONICAL_SURFACE ( 'NONE', #15002, 5.999999999999999112, 0.08726646259971666819 ) ;
#29436 = CARTESIAN_POINT ( 'NONE',  ( 0.000000000000000000, -9.314797388894900720, 1.239665997526854468 ) ) ;
#29437 = ADVANCED_FACE ( 'NONE', ( #30682 ), #6530, .T. ) ;
#29438 = CARTESIAN_POINT ( 'NONE',  ( 23.87320362639557203, -3.497993740964699949, 0.8105616805983073547 ) ) ;
#29439 = DIRECTION ( 'NONE',  ( -1.000000000000000000, -0.000000000000000000, -0.000000000000000000 ) ) ;
#29440 = DIRECTION ( 'NONE',  ( -1.000000000000000000, -0.000000000000000000, -0.000000000000000000 ) ) ;
#29441 = ORIENTED_EDGE ( 'NONE', *, *, #19148, .F. ) ;
#29442 = CARTESIAN_POINT ( 'NONE',  ( 7.249760686538667009, 6.147671362329302447, -6.226446564517854831 ) ) ;
#29443 = AXIS2_PLACEMENT_3D ( 'NONE', #17935, #383, #13081 ) ;
#29444 = CARTESIAN_POINT ( 'NONE',  ( -18.30155664144426453, 4.770368330595423290E-16, 3.895301350492843540 ) ) ;
#29446 = DIRECTION ( 'NONE',  ( 1.000000000000000000, -0.000000000000000000, -0.000000000000000000 ) ) ;
#29445 = CARTESIAN_POINT ( 'NONE',  ( -3.357304906975409953, 1.062355717592091686, 3.000000000000001332 ) ) ;
#29447 = VERTEX_POINT ( 'NONE', #22793 ) ;
#29448 = CIRCLE ( 'NONE', #629, 6.000000000000001776 ) ;
#29449 = CYLINDRICAL_SURFACE ( 'NONE', #24042, 3.499999999999999556 ) ;
#29450 = CIRCLE ( 'NONE', #15559, 2.499999999999998224 ) ;
#29452 = VERTEX_POINT ( 'NONE', #20283 ) ;
#29451 = B_SPLINE_CURVE_WITH_KNOTS ( 'NONE', 3,
 ( #3693, #20759, #23414, #521, #20921, #31141, #8226, #18426 ),
 .UNSPECIFIED., .F., .F.,
 ( 4, 2, 2, 4 ),
 ( 2.737843117451997097E-07, 0.001228034957219390367, 0.001841915543673211444, 0.002455796130127031220 ),
 .UNSPECIFIED. ) ;
#29453 = CARTESIAN_POINT ( 'NONE',  ( -23.35000000000000142, -10.96966150227469505, -1.499999999999999556 ) ) ;
#29455 = VERTEX_POINT ( 'NONE', #23129 ) ;
#29454 = CARTESIAN_POINT ( 'NONE',  ( 18.86033062536104055, -4.738446029132363790, -3.997238537406878844 ) ) ;
#29456 = ORIENTED_EDGE ( 'NONE', *, *, #4138, .F. ) ;
#29457 = AXIS2_PLACEMENT_3D ( 'NONE', #23934, #1044, #31654 ) ;
#29458 = CIRCLE ( 'NONE', #5439, 4.999999999999999112 ) ;
#29459 = EDGE_CURVE ( 'NONE', #30955, #30284, #17773, .T. ) ;
#29461 = CIRCLE ( 'NONE', #24126, 5.009999999999999787 ) ;
#29460 = CARTESIAN_POINT ( 'NONE',  ( 22.00639167669224960, -21.80013755708282730, -1.499999999999999556 ) ) ;
#29462 = PRODUCT_RELATED_PRODUCT_CATEGORY ( 'detail', '', ( #5241 ) ) ;
#29464 = ORIENTED_EDGE ( 'NONE', *, *, #31481, .T. ) ;
#29463 = CARTESIAN_POINT ( 'NONE',  ( -2.807293726618242946, -12.37543429821833385, -1.499999999999999556 ) ) ;
#29465 = CARTESIAN_POINT ( 'NONE',  ( 10.00000000000000000, 2.376879293651063652, 4.116875700062091248 ) ) ;
#29466 = DIRECTION ( 'NONE',  ( 0.000000000000000000, 0.000000000000000000, 1.000000000000000000 ) ) ;
#29467 = PLANE ( 'NONE',  #18757 ) ;
#29468 = CARTESIAN_POINT ( 'NONE',  ( 7.166310627377574072, -7.340520188494797260, -1.499999999999856559 ) ) ;
#29470 = ORIENTED_EDGE ( 'NONE', *, *, #24551, .T. ) ;
#29469 = CARTESIAN_POINT ( 'NONE',  ( 107.4526306908116879, -17.39749363332668608, -4.613092379735242332 ) ) ;
#29471 = CARTESIAN_POINT ( 'NONE',  ( -4.900050802731187538, -1.549418761218565255, 2.853674364686380471 ) ) ;
#29472 = AXIS2_PLACEMENT_3D ( 'NONE', #28133, #8057, #30834 ) ;
#29473 = AXIS2_PLACEMENT_3D ( 'NONE', #11622, #31537, #8621 ) ;
#29474 = CARTESIAN_POINT ( 'NONE',  ( 10.52034268205830614, -3.055657119358777152, -3.641590349731960163 ) ) ;
#29475 = DIRECTION ( 'NONE',  ( -6.062761635205655873E-17, -0.7071067811865558994, 0.7071067811865392461 ) ) ;
#29476 = ADVANCED_FACE ( 'NONE', ( #18265 ), #10419, .T. ) ;
#29477 = VECTOR ( 'NONE', #29480, 1000.000000000000000 ) ;
#29478 = VECTOR ( 'NONE', #2133, 1000.000000000000000 ) ;
#29479 = CARTESIAN_POINT ( 'NONE',  ( 33.00121834596181714, -0.06979899340500209104, -3.000000000000002665 ) ) ;
#29480 = DIRECTION ( 'NONE',  ( -1.000000000000000000, 8.574039729943018344E-17, 0.000000000000000000 ) ) ;
#29481 = VERTEX_POINT ( 'NONE', #15592 ) ;
#29482 = CARTESIAN_POINT ( 'NONE',  ( 18.93617721851659041, -3.890633339435721982, -4.522129901861162260 ) ) ;
#29483 = CIRCLE ( 'NONE', #5966, 7.634842307437897269 ) ;
#29484 = EDGE_CURVE ( 'NONE', #6718, #17929, #25806, .T. ) ;
#29485 = AXIS2_PLACEMENT_3D ( 'NONE', #10393, #30809, #7877 ) ;
#29486 = CARTESIAN_POINT ( 'NONE',  ( 2.274274201625327230, -7.593217523260523016, -7.958834565716851550 ) ) ;
#29487 = EDGE_LOOP ( 'NONE', ( #5351, #4712, #24768, #16405 ) ) ;
#29488 = VECTOR ( 'NONE', #15455, 999.9999999999998863 ) ;
#29489 = DIRECTION ( 'NONE',  ( 0.000000000000000000, 0.000000000000000000, -1.000000000000000000 ) ) ;
#29490 = CARTESIAN_POINT ( 'NONE',  ( 108.8978791464556508, 17.52043075494136204, -4.999054092451819642 ) ) ;
#29491 = ORIENTED_EDGE ( 'NONE', *, *, #12012, .T. ) ;
#29492 = LINE ( 'NONE', #24614, #31076 ) ;
#29493 = ORIENTED_EDGE ( 'NONE', *, *, #24064, .F. ) ;
#29494 = VECTOR ( 'NONE', #23750, 1000.000000000000114 ) ;
#29495 = ORIENTED_EDGE ( 'NONE', *, *, #15477, .T. ) ;
#29496 = CARTESIAN_POINT ( 'NONE',  ( 6.883866557622099869, 3.625395379390193629, -7.943335131954968986 ) ) ;
#29497 = CIRCLE ( 'NONE', #24690, 10.94895958125474245 ) ;
#29499 = ORIENTED_EDGE ( 'NONE', *, *, #29651, .F. ) ;
#29498 = CARTESIAN_POINT ( 'NONE',  ( 6.883866482134012976, -8.691827696555163740, 0.8319830743950369367 ) ) ;
#29500 = ORIENTED_EDGE ( 'NONE', *, *, #24264, .F. ) ;
#29501 = CARTESIAN_POINT ( 'NONE',  ( 21.42250000136559507, 1.913930629741522838, -2.363507492473150062 ) ) ;
#29502 = AXIS2_PLACEMENT_3D ( 'NONE', #12894, #23116, #7554 ) ;
#29503 = AXIS2_PLACEMENT_3D ( 'NONE', #24519, #1645, #24026 ) ;
#29504 = CIRCLE ( 'NONE', #18844, 8.749000000000002331 ) ;
#29505 = ORIENTED_EDGE ( 'NONE', *, *, #28212, .T. ) ;
#29506 = DIRECTION ( 'NONE',  ( 1.000000000000000000, -2.298508605669267507E-14, 1.734723475976805517E-15 ) ) ;
#29507 =( BOUNDED_SURFACE ( )  B_SPLINE_SURFACE ( 3, 3, ( 
 ( #12072, #22607, #25274, #4560, #17257, #4389, #32819, #14572 ),
 ( #22267, #32637, #24587, #14734, #20107, #29797, #6870, #25087 ),
 ( #24932, #1713, #32478, #30298, #14375, #32146, #9717, #1898 ),
 ( #7374, #29641, #9539, #7226, #19752, #19942, #11911, #17563 ) ),
 .UNSPECIFIED., .F., .F., .F. ) 
 B_SPLINE_SURFACE_WITH_KNOTS ( ( 4, 4 ),
 ( 4, 2, 2, 4 ),
 ( 0.000000000000000000, 1.000000000000000000 ),
 ( 0.000000000000000000, 0.5000000000000000000, 0.7500000000000000000, 1.000000000000000000 ),
 .UNSPECIFIED. ) 
 GEOMETRIC_REPRESENTATION_ITEM ( )  RATIONAL_B_SPLINE_SURFACE ( (
 ( 1.000000000000000000, 1.000000000000000000, 1.000000000000000000, 1.000000000000000000, 1.000000000000000000, 1.000000000000000000, 1.000000000000000000, 1.000000000000000000),
 ( 0.9743068154145673176, 0.9743068154145673176, 0.9743068154145673176, 0.9743068154145673176, 0.9743068154145673176, 0.9743068154145673176, 0.9743068154145673176, 0.9743068154145673176),
 ( 0.9743068154145673176, 0.9743068154145673176, 0.9743068154145673176, 0.9743068154145673176, 0.9743068154145673176, 0.9743068154145673176, 0.9743068154145673176, 0.9743068154145673176),
 ( 1.000000000000000000, 1.000000000000000000, 1.000000000000000000, 1.000000000000000000, 1.000000000000000000, 1.000000000000000000, 1.000000000000000000, 1.000000000000000000) ) ) 
 REPRESENTATION_ITEM ( '' )  SURFACE ( )  );
#29508 = CARTESIAN_POINT ( 'NONE',  ( 5.377543748152548986, 6.940565734314653845, -4.007137495034738706 ) ) ;
#29510 = ORIENTED_EDGE ( 'NONE', *, *, #6525, .F. ) ;
#29509 = CARTESIAN_POINT ( 'NONE',  ( 68.95644445486074403, -3.844730188641327651, -2.184957270837231569 ) ) ;
#29511 = DIRECTION ( 'NONE',  ( -0.1437473352845045071, 0.000000000000000000, 0.9896144216807898353 ) ) ;
#29512 = CARTESIAN_POINT ( 'NONE',  ( 2.592584712403274150, 2.232024585009849016, -10.08167743097170543 ) ) ;
#29513 = CIRCLE ( 'NONE', #11897, 4.000000000000001776 ) ;
#29514 = CIRCLE ( 'NONE', #10822, 0.4999999999999978351 ) ;
#29515 = CARTESIAN_POINT ( 'NONE',  ( 101.8731863870445267, -5.072399176882428584, 2.336383929218190492 ) ) ;
#29516 = DIRECTION ( 'NONE',  ( 0.000000000000000000, -0.7071067811865558994, 0.7071067811865392461 ) ) ;
#29517 = VECTOR ( 'NONE', #24890, 1000.000000000000000 ) ;
#29518 = B_SPLINE_CURVE_WITH_KNOTS ( 'NONE', 3,
 ( #102, #15141, #17823, #24993, #27521, #12625, #2457, #22328, #17473, #33033 ),
 .UNSPECIFIED., .F., .F.,
 ( 4, 2, 2, 2, 4 ),
 ( 2.493548413898819905E-07, 0.0005478513795029405983, 0.001095453404164491292, 0.001643055428826041987, 0.002190657453487592464 ),
 .UNSPECIFIED. ) ;
#29519 = CARTESIAN_POINT ( 'NONE',  ( 3.499999999999999556, 6.100541242131516384, 3.528937025535512362 ) ) ;
#29520 = LINE ( 'NONE', #21979, #19286 ) ;
#29521 = CARTESIAN_POINT ( 'NONE',  ( 7.577572045913206544, 15.00000000000002132, -4.612695725900421984 ) ) ;
#29522 = EDGE_CURVE ( 'NONE', #1159, #20638, #29458, .T. ) ;
#29523 = AXIS2_PLACEMENT_3D ( 'NONE', #24236, #11858, #17205 ) ;
#29524 = EDGE_CURVE ( 'NONE', #29226, #9973, #26272, .T. ) ;
#29525 = FACE_BOUND ( 'NONE', #27078, .T. ) ;
#29526 = VECTOR ( 'NONE', #5139, 1000.000000000000000 ) ;
#29527 = CARTESIAN_POINT ( 'NONE',  ( 0.000000000000000000, 0.000000000000000000, 0.000000000000000000 ) ) ;
#29528 = DIRECTION ( 'NONE',  ( -0.9993908270190957621, 0.03489949670250105246, 0.000000000000000000 ) ) ;
#29529 = CIRCLE ( 'NONE', #30624, 302.4235430809786749 ) ;
#29530 = VECTOR ( 'NONE', #5269, 1000.000000000000000 ) ;
#29531 = DIRECTION ( 'NONE',  ( -1.000000000000000000, 0.000000000000000000, 0.000000000000000000 ) ) ;
#29532 = CARTESIAN_POINT ( 'NONE',  ( -6.700050802731187360, 2.853674364686379583, 1.549418761218565921 ) ) ;
#29533 = ORIENTED_EDGE ( 'NONE', *, *, #25358, .F. ) ;
#29534 = VECTOR ( 'NONE', #14321, 1000.000000000000000 ) ;
#29535 = VECTOR ( 'NONE', #9193, 1000.000000000000000 ) ;
#29536 = CARTESIAN_POINT ( 'NONE',  ( -5.750050799999999462, 0.9222479816126443186, 3.113457007523260156 ) ) ;
#29537 = DIRECTION ( 'NONE',  ( 0.000000000000000000, 0.000000000000000000, 1.000000000000000000 ) ) ;
#29538 = FACE_OUTER_BOUND ( 'NONE', #29799, .T. ) ;
#29539 = CARTESIAN_POINT ( 'NONE',  ( 6.879500825888995585, -8.675028761530525045, 1.500000000000000000 ) ) ;
#29540 = CIRCLE ( 'NONE', #21002, 8.500000000000000000 ) ;
#29541 = EDGE_LOOP ( 'NONE', ( #16318, #2335, #11311, #5379, #10669, #29674, #476, #9657, #3938, #12663, #11865, #4769 ) ) ;
#29542 = CARTESIAN_POINT ( 'NONE',  ( 9.613697478362256632, -12.36077863760288231, -1.500000000000000444 ) ) ;
#29543 = ORIENTED_EDGE ( 'NONE', *, *, #1809, .T. ) ;
#29544 = CARTESIAN_POINT ( 'NONE',  ( 0.4214208491204014528, -4.489406624787253719, 1.766534570867400955 ) ) ;
#29545 = APPROVAL_ROLE ( '' ) ;
#29546 = CARTESIAN_POINT ( 'NONE',  ( -1.433134780067091442E-16, -9.620177616658022401, 5.227991826304056566 ) ) ;
#29547 = ORIENTED_EDGE ( 'NONE', *, *, #8813, .T. ) ;
#29548 = CARTESIAN_POINT ( 'NONE',  ( 11.59711033912294731, -20.31971356584124422, 1.499999999999999334 ) ) ;
#29549 = CARTESIAN_POINT ( 'NONE',  ( 3.499999999999999556, -7.009698679648292519, 0.7308381473896670144 ) ) ;
#29550 = CIRCLE ( 'NONE', #729, 2.999999999999999112 ) ;
#29551 = CARTESIAN_POINT ( 'NONE',  ( 9.220104123695119114, 0.1261569107277066837, -1.391360883757695399 ) ) ;
#29552 = AXIS2_PLACEMENT_3D ( 'NONE', #7185, #10160, #32776 ) ;
#29553 = FACE_OUTER_BOUND ( 'NONE', #3604, .T. ) ;
#29554 = CARTESIAN_POINT ( 'NONE',  ( 0.7632845268398871230, 0.000000000000000000, 0.000000000000000000 ) ) ;
#29555 = ORIENTED_EDGE ( 'NONE', *, *, #6127, .F. ) ;
#29556 = AXIS2_PLACEMENT_3D ( 'NONE', #21672, #32384, #31879 ) ;
#29557 = CARTESIAN_POINT ( 'NONE',  ( 8.886302293890576465, 0.01997115109545394632, 1.161565467022927622 ) ) ;
#29558 = CARTESIAN_POINT ( 'NONE',  ( 1.394036994807608625E-16, 1.625881193364697719, 4.467071865485476856 ) ) ;
#29559 = VECTOR ( 'NONE', #4696, 1000.000000000000000 ) ;
#29560 = DIRECTION ( 'NONE',  ( 1.000000000000000000, -0.000000000000000000, -0.000000000000000000 ) ) ;
#29561 = VECTOR ( 'NONE', #5564, 1000.000000000000000 ) ;
#29562 = EDGE_CURVE ( 'NONE', #28100, #21723, #19656, .T. ) ;
#29564 = ORIENTED_EDGE ( 'NONE', *, *, #32909, .T. ) ;
#29563 = CARTESIAN_POINT ( 'NONE',  ( 25.75181271650331993, 2.887405513829538251, 0.9065264845798409743 ) ) ;
#29565 = CARTESIAN_POINT ( 'NONE',  ( 108.1105523077318651, 18.79375879618914169, -4.458706230583343810 ) ) ;
#29566 = FACE_OUTER_BOUND ( 'NONE', #17223, .T. ) ;
#29567 = CARTESIAN_POINT ( 'NONE',  ( 5.612974384376776982, -3.934067627273155399, -7.213266193303299545 ) ) ;
#29568 = CARTESIAN_POINT ( 'NONE',  ( 25.75999999999999801, -2.208672634433321348E-15, 0.000000000000000000 ) ) ;
#29569 = CARTESIAN_POINT ( 'NONE',  ( 0.000000000000000000, 10.85582367538894211, 1.425064293572374963 ) ) ;
#29570 = LOCAL_TIME ( 16, 7, 10.00000000000000000, #21869 ) ;
#29571 = CARTESIAN_POINT ( 'NONE',  ( 107.9916885326170473, -18.73354948406877440, 4.428418223197585490 ) ) ;
#29572 = DIRECTION ( 'NONE',  ( 0.000000000000000000, 0.7071067811865465735, 0.7071067811865484609 ) ) ;
#29573 = FACE_OUTER_BOUND ( 'NONE', #32070, .T. ) ;
#29574 = ORIENTED_EDGE ( 'NONE', *, *, #13539, .F. ) ;
#29575 = CARTESIAN_POINT ( 'NONE',  ( -2.562942409646512321, -5.022711880624455567E-15, 2.999999999999999556 ) ) ;
#29576 = ORIENTED_EDGE ( 'NONE', *, *, #6084, .T. ) ;
#29577 = CARTESIAN_POINT ( 'NONE',  ( 17.32050807568873552, 10.00000000000002309, 0.000000000000000000 ) ) ;
#29578 = AXIS2_PLACEMENT_3D ( 'NONE', #22704, #5144, #9822 ) ;
#29579 = FACE_OUTER_BOUND ( 'NONE', #27941, .T. ) ;
#29580 = CIRCLE ( 'NONE', #10365, 6.000000000000001776 ) ;
#29581 = EDGE_CURVE ( 'NONE', #11409, #22634, #13567, .T. ) ;
#29582 = CARTESIAN_POINT ( 'NONE',  ( 23.68064580653238949, -7.171681651382474598, -4.522129901861164036 ) ) ;
#29583 = AXIS2_PLACEMENT_3D ( 'NONE', #22449, #25618, #32845 ) ;
#29584 = CYLINDRICAL_SURFACE ( 'NONE', #24718, 4.000000000000001776 ) ;
#29585 = CARTESIAN_POINT ( 'NONE',  ( 55.01406067017558144, -7.826279391975567101, 1.873789188489173307 ) ) ;
#29586 = ORIENTED_EDGE ( 'NONE', *, *, #969, .F. ) ;
#29587 = CARTESIAN_POINT ( 'NONE',  ( -40.16771308880407076, -10.96999999999998643, 5.500000000000000000 ) ) ;
#29588 = VERTEX_POINT ( 'NONE', #16250 ) ;
#29589 = COORDINATED_UNIVERSAL_TIME_OFFSET ( 0, 0, .AHEAD. ) ;
#29590 = EDGE_CURVE ( 'NONE', #7057, #27059, #29993, .T. ) ;
#29592 = CARTESIAN_POINT ( 'NONE',  ( 18.75835488814835728, -5.878330108280717781, 3.994702635762014342 ) ) ;
#29591 = APPROVAL_PERSON_ORGANIZATION ( #14997, #6347, #13012 ) ;
#29593 = DIRECTION ( 'NONE',  ( -1.000000000000000000, -0.000000000000000000, -0.000000000000000000 ) ) ;
#29594 = LINE ( 'NONE', #14510, #28445 ) ;
#29595 = EDGE_CURVE ( 'NONE', #11257, #19641, #6059, .T. ) ;
#29596 = ORIENTED_EDGE ( 'NONE', *, *, #11444, .F. ) ;
#29597 = ORIENTED_EDGE ( 'NONE', *, *, #3734, .F. ) ;
#29598 = CARTESIAN_POINT ( 'NONE',  ( 5.489321708267617339, 6.152096559282836274, 5.297846913781713241 ) ) ;
#29599 = CARTESIAN_POINT ( 'NONE',  ( 5.885541806331896275, -7.447669719165306290, -3.871259391815531359 ) ) ;
#29600 = CARTESIAN_POINT ( 'NONE',  ( 23.92249999999999943, 2.378061970571979433, -1.291182301015470824 ) ) ;
#29601 = CARTESIAN_POINT ( 'NONE',  ( 0.3474085791285200786, -7.723996299823893352, -1.499999999999981570 ) ) ;
#29603 = EDGE_LOOP ( 'NONE', ( #548, #27147, #22743, #12897 ) ) ;
#29602 = FACE_OUTER_BOUND ( 'NONE', #31033, .T. ) ;
#29604 = AXIS2_PLACEMENT_3D ( 'NONE', #30744, #27545, #128 ) ;
#29605 = CARTESIAN_POINT ( 'NONE',  ( -2.637550801365593500, -1.088641768524163389, -3.675193018007246071 ) ) ;
#29606 = CYLINDRICAL_SURFACE ( 'NONE', #27791, 3.000000000000000444 ) ;
#29608 = EDGE_CURVE ( 'NONE', #14457, #24661, #24096, .T. ) ;
#29607 = CARTESIAN_POINT ( 'NONE',  ( 107.5603894785018468, -18.96336710931913316, -4.563597971271542875 ) ) ;
#29609 = ORIENTED_EDGE ( 'NONE', *, *, #7944, .F. ) ;
#29611 = ORIENTED_EDGE ( 'NONE', *, *, #6497, .F. ) ;
#29610 = DIRECTION ( 'NONE',  ( -1.000000000000000000, 8.574039729943017111E-17, -0.000000000000000000 ) ) ;
#29612 = EDGE_CURVE ( 'NONE', #19939, #21907, #3225, .T. ) ;
#29613 = CARTESIAN_POINT ( 'NONE',  ( 16.02642041956679719, 11.88017725832204974, 1.500000000000000222 ) ) ;
#29614 = CARTESIAN_POINT ( 'NONE',  ( 5.489321486716459475, 7.976795196726687465, 1.512021494499613761 ) ) ;
#29615 = ORGANIZATION ( 'NAUO-ORG7', 'UNSPECIFIED', 'UNSPECIFIED' ) ;
#29616 = CARTESIAN_POINT ( 'NONE',  ( -16.41799616858202171, 12.22102706438217368, 1.500000000000000000 ) ) ;
#29617 = CARTESIAN_POINT ( 'NONE',  ( -24.41756317296288969, 18.46223496596762459, 1.773004750130063867 ) ) ;
#29618 = CARTESIAN_POINT ( 'NONE',  ( -3.135269660805079628, -0.5000000000000025535, -1.500000000000000000 ) ) ;
#29619 = CARTESIAN_POINT ( 'NONE',  ( 5.084999606894402593E-16, -5.227991826304019263, -9.620177616658041941 ) ) ;
#29620 = CARTESIAN_POINT ( 'NONE',  ( 47.88260332740732395, -3.822977517009182868, 0.4367665431859983349 ) ) ;
#29621 = DIRECTION ( 'NONE',  ( -1.000000000000000000, 0.000000000000000000, -0.000000000000000000 ) ) ;
#29622 = ORIENTED_EDGE ( 'NONE', *, *, #29484, .F. ) ;
#29623 = DIRECTION ( 'NONE',  ( 0.000000000000000000, 1.000000000000000000, 0.000000000000000000 ) ) ;
#29624 = EDGE_LOOP ( 'NONE', ( #20634, #17775, #23363 ) ) ;
#29625 = EDGE_CURVE ( 'NONE', #30338, #21513, #18749, .T. ) ;
#29626 = VECTOR ( 'NONE', #32161, 1000.000000000000000 ) ;
#29627 = CARTESIAN_POINT ( 'NONE',  ( 9.302055952181039089, 0.2457637073014079521, -1.050000000000000044 ) ) ;
#29628 = CARTESIAN_POINT ( 'NONE',  ( -8.000050800000018114, 1.979734913925816908, -2.936190332390367086 ) ) ;
#29630 = CARTESIAN_POINT ( 'NONE',  ( 18.86054332783516330, -4.736068442360130248, -3.993434336035624366 ) ) ;
#29629 = LINE ( 'NONE', #15340, #10770 ) ;
#29631 = ORIENTED_EDGE ( 'NONE', *, *, #29842, .F. ) ;
#29632 = DIRECTION ( 'NONE',  ( -1.000000000000000000, 0.000000000000000000, 0.000000000000000000 ) ) ;
#29633 = ORIENTED_EDGE ( 'NONE', *, *, #7732, .T. ) ;
#29634 = CARTESIAN_POINT ( 'NONE',  ( 2.274274201625327230, -10.90201369670499609, 1.464956435139503022 ) ) ;
#29636 = ORIENTED_EDGE ( 'NONE', *, *, #31925, .T. ) ;
#29635 = CARTESIAN_POINT ( 'NONE',  ( 84.96569962550037758, -4.060952333826338467, -3.996603857777809132 ) ) ;
#29637 = ORIENTED_EDGE ( 'NONE', *, *, #10065, .F. ) ;
#29638 = APPROVAL_PERSON_ORGANIZATION ( #19124, #10621, #1264 ) ;
#29639 = EDGE_CURVE ( 'NONE', #10525, #7224, #21120, .T. ) ;
#29640 = CARTESIAN_POINT ( 'NONE',  ( 5.887530252753766291, 5.676096663009888132, -6.185189124321764709 ) ) ;
#29641 = CARTESIAN_POINT ( 'NONE',  ( 85.08949032934707191, -1.315411135598756553, 0.07017451552782173751 ) ) ;
#29643 = EDGE_LOOP ( 'NONE', ( #20331, #25859, #18163, #20625 ) ) ;
#29642 = CARTESIAN_POINT ( 'NONE',  ( 2.281627749324420140, -0.2935656086769634077, -1.757435426329174710 ) ) ;
#29644 = CARTESIAN_POINT ( 'NONE',  ( 13.32584843873297409, 6.791410140412673435, -1.500000000000237366 ) ) ;
#29645 = DIRECTION ( 'NONE',  ( -1.000000000000000000, 8.574039729943022041E-17, -1.232595164407830946E-32 ) ) ;
#29646 = CARTESIAN_POINT ( 'NONE',  ( -1.348815490713419493E-16, -7.533794289458111137, 7.944914065997086716 ) ) ;
#29647 = EDGE_CURVE ( 'NONE', #18404, #21855, #1031, .T. ) ;
#29648 = CARTESIAN_POINT ( 'NONE',  ( 6.800570610007084404, -8.349954097220308569, -1.500000000000000000 ) ) ;
#29650 = VERTEX_POINT ( 'NONE', #28959 ) ;
#29649 = CARTESIAN_POINT ( 'NONE',  ( 107.4581045272831545, -17.47692235061807864, -4.756303059044163284 ) ) ;
#29651 = EDGE_CURVE ( 'NONE', #9004, #19632, #19319, .T. ) ;
#29652 = DIRECTION ( 'NONE',  ( 0.000000000000000000, 0.000000000000000000, 1.000000000000000000 ) ) ;
#29653 = CARTESIAN_POINT ( 'NONE',  ( 0.7632845268451400322, 6.772677083973724699, 5.538577986791671570 ) ) ;
#29654 = CARTESIAN_POINT ( 'NONE',  ( 9.350000000000001421, 0.000000000000000000, 1.000000000000000000 ) ) ;
#29655 = CARTESIAN_POINT ( 'NONE',  ( 24.46547057403054737, -17.44104734125400213, -1.464603527736665134 ) ) ;
#29656 = DIRECTION ( 'NONE',  ( -1.000000000000000000, 0.000000000000000000, 0.000000000000000000 ) ) ;
#29657 = VERTEX_POINT ( 'NONE', #8250 ) ;
#29658 = DIRECTION ( 'NONE',  ( 0.000000000000000000, 0.000000000000000000, -1.000000000000000000 ) ) ;
#29659 = CYLINDRICAL_SURFACE ( 'NONE', #30031, 5.010000000000000675 ) ;
#29660 = CARTESIAN_POINT ( 'NONE',  ( 2.857988133323936530, -6.150950518044163928, -7.318787950819745092 ) ) ;
#29661 = EDGE_LOOP ( 'NONE', ( #7183, #5210, #12220, #4722 ) ) ;
#29662 = EDGE_CURVE ( 'NONE', #3311, #15684, #14060, .T. ) ;
#29663 = APPROVAL ( #21344, 'UNSPECIFIED' ) ;
#29664 = FACE_OUTER_BOUND ( 'NONE', #5408, .T. ) ;
#29665 = DIRECTION ( 'NONE',  ( 2.473959037481232675E-13, 1.000000000000000000, 0.000000000000000000 ) ) ;
#29666 = ORIENTED_EDGE ( 'NONE', *, *, #9363, .T. ) ;
#29667 = CARTESIAN_POINT ( 'NONE',  ( 0.000000000000000000, 4.561279057474472154, -4.271385531633124621 ) ) ;
#29668 = VERTEX_POINT ( 'NONE', #5731 ) ;
#29669 = EDGE_LOOP ( 'NONE', ( #16498, #24047, #18392, #6994 ) ) ;
#29670 = CARTESIAN_POINT ( 'NONE',  ( 10.00000000000000178, -8.574039729943018837E-16, 0.000000000000000000 ) ) ;
#29671 = DATE_AND_TIME ( #13761, #10373 ) ;
#29673 = ORIENTED_EDGE ( 'NONE', *, *, #33085, .T. ) ;
#29672 = DIRECTION ( 'NONE',  ( -1.000000000000000000, -0.000000000000000000, 0.000000000000000000 ) ) ;
#29674 = ORIENTED_EDGE ( 'NONE', *, *, #7811, .F. ) ;
#29675 = CARTESIAN_POINT ( 'NONE',  ( 23.73500000136559507, 1.570731468192929858, 2.892927487894329630 ) ) ;
#29676 = ADVANCED_FACE ( 'NONE', ( #29125 ), #6211, .T. ) ;
#29677 = EDGE_LOOP ( 'NONE', ( #21488, #32856, #8291, #16556 ) ) ;
#29678 = DIRECTION ( 'NONE',  ( 1.000000000000000000, -3.540392581751473016E-15, 0.000000000000000000 ) ) ;
#29679 = CARTESIAN_POINT ( 'NONE',  ( 1.787149210215136508, -1.031811077599730231, 1.500000000000000000 ) ) ;
#29681 = VERTEX_POINT ( 'NONE', #3709 ) ;
#29680 = DIRECTION ( 'NONE',  ( 0.000000000000000000, 1.000000000000000000, 0.000000000000000000 ) ) ;
#29682 = CARTESIAN_POINT ( 'NONE',  ( 1.750000000000000222, -5.848742439617879540, -6.167836887841045446 ) ) ;
#29683 = CARTESIAN_POINT ( 'NONE',  ( -56.36516744639037313, 0.007311977099128529056, -1.006610376653334971 ) ) ;
#29684 = CARTESIAN_POINT ( 'NONE',  ( 5.489321486716458587, 1.307389195612976618, 8.012877392144801547 ) ) ;
#29685 = CARTESIAN_POINT ( 'NONE',  ( 24.92250000136559507, -1.913930629741527500, 2.363507492473149618 ) ) ;
#29686 = CARTESIAN_POINT ( 'NONE',  ( 2.440333830126093950, 5.258796312403019257, -9.290196408095376057 ) ) ;
#29687 = CARTESIAN_POINT ( 'NONE',  ( 15.28872660057386845, 20.76088595412476678, -4.612695725900421984 ) ) ;
#29688 = CARTESIAN_POINT ( 'NONE',  ( 102.5437075123492292, -5.726773290143885475, -0.07017451552783424140 ) ) ;
#29689 = PLANE ( 'NONE',  #6115 ) ;
#29690 = DIRECTION ( 'NONE',  ( 8.574039729943018344E-17, 1.000000000000000000, 0.000000000000000000 ) ) ;
#29691 = CARTESIAN_POINT ( 'NONE',  ( -5.240875073191923583, 0.000000000000000000, -3.405250132838343102 ) ) ;
#29692 = CARTESIAN_POINT ( 'NONE',  ( 2.274274201625327230, 0.000000000000000000, 0.000000000000000000 ) ) ;
#29693 = FACE_OUTER_BOUND ( 'NONE', #19411, .T. ) ;
#29694 = ADVANCED_FACE ( 'NONE', ( #1210 ), #13385, .T. ) ;
#29695 = CARTESIAN_POINT ( 'NONE',  ( -5.000050802731188959, 0.9222479816126443186, 3.113457007523260156 ) ) ;
#29696 = ORIENTED_EDGE ( 'NONE', *, *, #23763, .T. ) ;
#29697 = CARTESIAN_POINT ( 'NONE',  ( -7.487550801365594033, -2.228590825266444586, -2.752080473201636401 ) ) ;
#29698 = DIRECTION ( 'NONE',  ( 1.000000000000000000, -0.000000000000000000, -0.000000000000000000 ) ) ;
#29699 = DIRECTION ( 'NONE',  ( 0.000000000000000000, -1.598721155460225418E-14, 1.000000000000000000 ) ) ;
#29700 = CARTESIAN_POINT ( 'NONE',  ( 0.7632845268398876781, -8.734705317681624948, 0.4999240074894106822 ) ) ;
#29701 = ORIENTED_EDGE ( 'NONE', *, *, #15698, .F. ) ;
#29702 = CARTESIAN_POINT ( 'NONE',  ( 34.30400690026458932, 19.51744974835125035, -2.412380016372522196 ) ) ;
#29703 = CARTESIAN_POINT ( 'NONE',  ( 1.750000000000000222, 7.003298780661491918, -4.817032923780496745 ) ) ;
#29704 =( BOUNDED_SURFACE ( )  B_SPLINE_SURFACE ( 3, 2, ( 
 ( #20858, #31071, #10996 ),
 ( #21196, #8470, #5659 ),
 ( #28215, #23220, #10498 ),
 ( #5318, #15495, #636 ),
 ( #10827, #21042, #31249 ),
 ( #8323, #18519, #5968 ),
 ( #28712, #19512, #29544 ),
 ( #29706, #21678, #21343 ),
 ( #31886, #29353, #9296 ),
 ( #4125, #16164, #29200 ),
 ( #6288, #1609, #21829 ),
 ( #1119, #11797, #6631 ),
 ( #26536, #8636, #16823 ),
 ( #3791, #13962, #14145 ),
 ( #11315, #16473, #21525 ),
 ( #31735, #23999, #24344 ),
 ( #8810, #19017, #26680 ),
 ( #23853, #24181, #22006 ),
 ( #26395, #11142, #16328 ),
 ( #1308, #19341, #3493 ),
 ( #11484, #8952, #27023 ),
 ( #1456, #19160, #6441 ),
 ( #16648, #26858, #3975 ),
 ( #11634, #31548, #32040 ),
 ( #9109, #32230, #962 ),
 ( #13649, #18854, #29056 ),
 ( #3639, #14291, #24489 ),
 ( #6146, #13794, #14953 ),
 ( #4778, #30366, #6942 ),
 ( #32719, #25166, #17634 ),
 ( #2288, #4280, #2107 ),
 ( #9449, #7134, #27839 ),
 ( #6787, #17476, #1962 ),
 ( #24668, #27523, #19830 ),
 ( #16975, #22500, #27173 ),
 ( #10107, #14453, #1796 ),
 ( #17329, #27675, #19667 ),
 ( #22686, #9798, #27354 ) ),
 .UNSPECIFIED., .F., .F., .F. ) 
 B_SPLINE_SURFACE_WITH_KNOTS ( ( 4, 2, 2, 2, 2, 2, 2, 2, 2, 2, 2, 2, 2, 2, 2, 2, 2, 2, 4 ),
 ( 3, 3 ),
 ( 0.000000000000000000, 0.001917845367245767704, 0.003835690734491535407, 0.004794613418114419476, 0.005753536101737302677, 0.006712458785360186746, 0.007191920127171628346, 0.007671381468983070814, 0.008630304152605954016, 0.009589226836228838952, 0.01150707220347460535, 0.01246599488709749029, 0.01342491757072037349, 0.01534276293796614163, 0.01726060830521190803, 0.01917845367245767790, 0.02301414440694921071, 0.02684983514144074698, 0.03068552587593228326 ),
 ( 0.000000000000000000, 1.000000000000000000 ),
 .UNSPECIFIED. ) 
 GEOMETRIC_REPRESENTATION_ITEM ( )  RATIONAL_B_SPLINE_SURFACE ( (
 ( 1.000000000000000000, 0.8449619147701442623, 1.000000000000000000),
 ( 1.000000000000000000, 0.8445678281941895182, 1.000000000000000000),
 ( 1.000000000000000000, 0.8440735482790849842, 1.000000000000000000),
 ( 1.000000000000000000, 0.8426717852686910204, 1.000000000000000000),
 ( 1.000000000000000000, 0.8417782867635215105, 1.000000000000000000),
 ( 1.000000000000000000, 0.8396989866086126408, 1.000000000000000000),
 ( 1.000000000000000000, 0.8389583138861036460, 1.000000000000000000),
 ( 1.000000000000000000, 0.8374420476517394629, 1.000000000000000000),
 ( 1.000000000000000000, 0.8366705097161594162, 1.000000000000000000),
 ( 1.000000000000000000, 0.8350115697338978960, 1.000000000000000000),
 ( 1.000000000000000000, 0.8340765399395944080, 1.000000000000000000),
 ( 1.000000000000000000, 0.8336680578661073149, 1.000000000000000000),
 ( 1.000000000000000000, 0.8336622264597983722, 1.000000000000000000),
 ( 1.000000000000000000, 0.8338830948382838226, 1.000000000000000000),
 ( 1.000000000000000000, 0.8341112768085173768, 1.000000000000000000),
 ( 1.000000000000000000, 0.8349632181683559473, 1.000000000000000000),
 ( 1.000000000000000000, 0.8357222399959970405, 1.000000000000000000),
 ( 1.000000000000000000, 0.8375330892283537887, 1.000000000000000000),
 ( 1.000000000000000000, 0.8383871522769865692, 1.000000000000000000),
 ( 1.000000000000000000, 0.8406677340059340864, 1.000000000000000000),
 ( 1.000000000000000000, 0.8419340173013039053, 1.000000000000000000),
 ( 1.000000000000000000, 0.8434078201704927613, 1.000000000000000000),
 ( 1.000000000000000000, 0.8438011345265380436, 1.000000000000000000),
 ( 1.000000000000000000, 0.8444525021093555184, 1.000000000000000000),
 ( 1.000000000000000000, 0.8447123061114764075, 1.000000000000000000),
 ( 1.000000000000000000, 0.8453648520239724906, 1.000000000000000000),
 ( 1.000000000000000000, 0.8456340021638725224, 1.000000000000000000),
 ( 1.000000000000000000, 0.8460540157046728682, 1.000000000000000000),
 ( 1.000000000000000000, 0.8462024902987614894, 1.000000000000000000),
 ( 1.000000000000000000, 0.8464941297768426853, 1.000000000000000000),
 ( 1.000000000000000000, 0.8466725100393527326, 1.000000000000000000),
 ( 1.000000000000000000, 0.8470349430677968083, 1.000000000000000000),
 ( 1.000000000000000000, 0.8471950786340051165, 1.000000000000000000),
 ( 1.000000000000000000, 0.8474407600832977172, 1.000000000000000000),
 ( 1.000000000000000000, 0.8475244351830560907, 1.000000000000000000),
 ( 1.000000000000000000, 0.8476586567771616787, 1.000000000000000000),
 ( 1.000000000000000000, 0.8477086664503143965, 1.000000000000000000),
 ( 1.000000000000000000, 0.8477574071929551147, 1.000000000000000000) ) ) 
 REPRESENTATION_ITEM ( '' )  SURFACE ( )  );
#29705 = ORIENTED_EDGE ( 'NONE', *, *, #32513, .T. ) ;
#29706 = CARTESIAN_POINT ( 'NONE',  ( 0.6729935896713523658, -5.225233662718014038, 1.500000000000000000 ) ) ;
#29707 = COORDINATED_UNIVERSAL_TIME_OFFSET ( 0, 0, .AHEAD. ) ;
#29708 = DIRECTION ( 'NONE',  ( 0.000000000000000000, 0.5877852522924689183, 0.8090169943749503378 ) ) ;
#29709 = VERTEX_POINT ( 'NONE', #725 ) ;
#29710 = CARTESIAN_POINT ( 'NONE',  ( 9.337065666035902822, -0.007760238742139066379, -1.098363920870219168 ) ) ;
#29711 = ADVANCED_FACE ( 'NONE', ( #31806 ), #8877, .F. ) ;
#29712 = ADVANCED_FACE ( 'NONE', ( #3885 ), #24266, .T. ) ;
#29713 = CARTESIAN_POINT ( 'NONE',  ( 14.89840567085375866, 9.424658325534814196, -1.050000000000000044 ) ) ;
#29714 = CARTESIAN_POINT ( 'NONE',  ( 85.02810471335169495, -5.078937868683484957, -4.155404232713865831 ) ) ;
#29715 = FACE_OUTER_BOUND ( 'NONE', #9263, .T. ) ;
#29716 = FACE_OUTER_BOUND ( 'NONE', #30907, .T. ) ;
#29717 = B_SPLINE_CURVE_WITH_KNOTS ( 'NONE', 3,
 ( #9311, #8966, #26693, #4297, #31748, #29723, #11997, #11496, #24356, #32057, #16989, #1627, #27036, #14476, #3810, #24686, #29563, #32249 ),
 .UNSPECIFIED., .F., .F.,
 ( 4, 2, 2, 2, 2, 2, 2, 2, 4 ),
 ( 0.008622242838676193177, 0.009334878258772234122, 0.01004751367886827507, 0.01076014909896431601, 0.01147278451906035696, 0.01218541993915639790, 0.01289805535925243885, 0.01361069077934847805, 0.01432332619944451900 ),
 .UNSPECIFIED. ) ;
#29718 = EDGE_CURVE ( 'NONE', #29588, #27801, #15188, .T. ) ;
#29719 = ORIENTED_EDGE ( 'NONE', *, *, #17517, .T. ) ;
#29720 = DIRECTION ( 'NONE',  ( 0.000000000000000000, 0.000000000000000000, 1.000000000000000000 ) ) ;
#29721 = LINE ( 'NONE', #19174, #11293 ) ;
#29722 = CARTESIAN_POINT ( 'NONE',  ( 109.4744264295851082, 15.07339897850246224, -2.806473568333505586 ) ) ;
#29724 = ORIENTED_EDGE ( 'NONE', *, *, #16435, .T. ) ;
#29723 = CARTESIAN_POINT ( 'NONE',  ( 25.62190975187500896, 1.596356670451427817, -2.417129575599294533 ) ) ;
#29725 = CARTESIAN_POINT ( 'NONE',  ( -57.12917293608614955, -2.964366234459024696, 5.871858320049880398 ) ) ;
#29726 = DIRECTION ( 'NONE',  ( -0.000000000000000000, 0.000000000000000000, 1.000000000000000000 ) ) ;
#29727 = CARTESIAN_POINT ( 'NONE',  ( -4.556376981307135310, 0.1572233378491222633, -3.000000000000000000 ) ) ;
#29728 = CARTESIAN_POINT ( 'NONE',  ( 25.59657441296793934, 19.00570861426560043, 1.395765800962750713 ) ) ;
#29729 = DIRECTION ( 'NONE',  ( 0.000000000000000000, 0.000000000000000000, -1.000000000000000000 ) ) ;
#29730 = CARTESIAN_POINT ( 'NONE',  ( 6.356381935169121533, -0.9265622495396348413, 8.556754636093206301 ) ) ;
#29731 = CARTESIAN_POINT ( 'NONE',  ( 7.249760686538667009, -1.391664247347174754, -7.892520144992448472 ) ) ;
#29732 = DIRECTION ( 'NONE',  ( -1.000000000000000000, 2.498001805406600196E-13, 0.000000000000000000 ) ) ;
#29733 = DIRECTION ( 'NONE',  ( 0.000000000000000000, 1.000000000000000000, 0.000000000000000000 ) ) ;
#29734 = VERTEX_POINT ( 'NONE', #22723 ) ;
#29735 = DIRECTION ( 'NONE',  ( 0.000000000000000000, -1.000000000000000000, 0.000000000000000000 ) ) ;
#29736 = EDGE_LOOP ( 'NONE', ( #26544, #31081, #4214, #29090 ) ) ;
#29737 = CARTESIAN_POINT ( 'NONE',  ( -7.104531657079157014, -2.975847129947406522, -0.3127741368606805072 ) ) ;
#29738 = CARTESIAN_POINT ( 'NONE',  ( 25.86000000136559862, 1.570731468192929858, 2.892927487894329186 ) ) ;
#29739 = CARTESIAN_POINT ( 'NONE',  ( -6.162942409646512409, 7.727249047114547632E-16, -2.999999999999999556 ) ) ;
#29740 = CARTESIAN_POINT ( 'NONE',  ( 109.4831014662948974, 20.77917954950586577, -0.4463807625373443777 ) ) ;
#29741 = DIRECTION ( 'NONE',  ( 0.000000000000000000, -0.9659258262890643154, -0.2588190451025359495 ) ) ;
#29742 = ORIENTED_EDGE ( 'NONE', *, *, #4956, .F. ) ;
#29743 = CARTESIAN_POINT ( 'NONE',  ( 107.8323272165538640, 17.24449170613245030, -2.317971953726807754 ) ) ;
#29744 = EDGE_CURVE ( 'NONE', #4178, #11832, #25390, .T. ) ;
#29745 = ORIENTED_EDGE ( 'NONE', *, *, #235, .F. ) ;
#29746 = MECHANICAL_CONTEXT ( 'NONE', #31920, 'mechanical' ) ;
#29747 = CARTESIAN_POINT ( 'NONE',  ( 28.66426575328085846, -6.758862791617487709, 4.003574682356660475 ) ) ;
#29748 = EDGE_CURVE ( 'NONE', #18185, #8026, #29629, .T. ) ;
#29749 = CARTESIAN_POINT ( 'NONE',  ( -4.716257286563783957, 20.00000000000000000, -4.924645716438867282 ) ) ;
#29750 = CYLINDRICAL_SURFACE ( 'NONE', #18298, 0.5000000000000004441 ) ;
#29751 = ORIENTED_EDGE ( 'NONE', *, *, #10619, .T. ) ;
#29752 = VERTEX_POINT ( 'NONE', #17515 ) ;
#29753 = FACE_OUTER_BOUND ( 'NONE', #12315, .T. ) ;
#29754 = CARTESIAN_POINT ( 'NONE',  ( -2.144454921107342038, 1.816023192640135786, 3.086171154715485088 ) ) ;
#29755 = CARTESIAN_POINT ( 'NONE',  ( 24.04749999999999943, 2.594547506269380133, 0.7685399846772031918 ) ) ;
#29756 = CARTESIAN_POINT ( 'NONE',  ( 9.015861660202212136, -14.64815961618594109, -1.754831069275766042 ) ) ;
#29758 = ORIENTED_EDGE ( 'NONE', *, *, #18537, .T. ) ;
#29757 = DIRECTION ( 'NONE',  ( 0.000000000000000000, 0.000000000000000000, 1.000000000000000000 ) ) ;
#29759 = CARTESIAN_POINT ( 'NONE',  ( -2.787550801365593411, -3.521866450007987037, -0.3701630799359323931 ) ) ;
#29760 = DIRECTION ( 'NONE',  ( 0.000000000000000000, -0.7071067811865483499, -0.7071067811865466846 ) ) ;
#29761 = DIRECTION ( 'NONE',  ( 1.000000000000000000, -0.000000000000000000, -0.000000000000000000 ) ) ;
#29762 = CARTESIAN_POINT ( 'NONE',  ( 10.00000000000000000, -4.467071865485484850, 1.625881193364682620 ) ) ;
#29763 = ORIENTED_EDGE ( 'NONE', *, *, #9947, .F. ) ;
#29765 = ORIENTED_EDGE ( 'NONE', *, *, #18500, .T. ) ;
#29764 = CARTESIAN_POINT ( 'NONE',  ( 3.519702661476644678, 3.984442983884231162E-15, 1.098333652976365871 ) ) ;
#29766 = DIRECTION ( 'NONE',  ( -1.000000000000000000, 0.000000000000000000, -0.000000000000000000 ) ) ;
#29767 = DIRECTION ( 'NONE',  ( -1.000000000000000000, -0.000000000000000000, 0.000000000000000000 ) ) ;
#29768 = APPLICATION_CONTEXT ( 'configuration controlled 3d designs of mechanical parts and assemblies' ) ;
#29769 = CARTESIAN_POINT ( 'NONE',  ( 26.50087866478441256, 17.58784721092444769, -0.4463807625373593657 ) ) ;
#29770 = CARTESIAN_POINT ( 'NONE',  ( -26.89442091290521830, 17.54567542505808575, 1.795026885182104071 ) ) ;
#29771 = CARTESIAN_POINT ( 'NONE',  ( -3.789183816811442007, -9.307783592219267987, -1.743674011537540203 ) ) ;
#29772 = CYLINDRICAL_SURFACE ( 'NONE', #27407, 4.000000000000001776 ) ;
#29773 = ADVANCED_FACE ( 'NONE', ( #11709 ), #19435, .F. ) ;
#29774 = PRODUCT_DEFINITION_SHAPE ( 'NONE', 'NONE',  #32113 ) ;
#29775 = CARTESIAN_POINT ( 'NONE',  ( 102.2517087015678925, -1.537876043683767735, 1.873789182642447537 ) ) ;
#29776 = CARTESIAN_POINT ( 'NONE',  ( -2.537550801365592967, 1.828967928396027176, -3.368539882008727115 ) ) ;
#29777 = VERTEX_POINT ( 'NONE', #22870 ) ;
#29778 = CARTESIAN_POINT ( 'NONE',  ( 18.51491971917342028, -8.599446730134173933, -0.07017451552783579571 ) ) ;
#29779 = EDGE_LOOP ( 'NONE', ( #23487, #12593, #9497 ) ) ;
#29780 = EDGE_CURVE ( 'NONE', #31964, #20990, #4310, .T. ) ;
#29781 = DIRECTION ( 'NONE',  ( 0.000000000000000000, 0.000000000000000000, 1.000000000000000000 ) ) ;
#29782 = SHAPE_REPRESENTATION_RELATIONSHIP ( 'NONE' , 'NONE' ,  #3460, #31139 ) ;
#29783 = EDGE_CURVE ( 'NONE', #11951, #23972, #12892, .T. ) ;
#29784 = LINE ( 'NONE', #6860, #6914 ) ;
#29785 = CARTESIAN_POINT ( 'NONE',  ( -34.55406472725060496, 0.5174497483512505713, 3.046515352619032946 ) ) ;
#29786 = EDGE_LOOP ( 'NONE', ( #11111, #16160 ) ) ;
#29787 = B_SPLINE_CURVE_WITH_KNOTS ( 'NONE', 3,
 ( #25206, #4995, #7469, #18169, #30246, #27703 ),
 .UNSPECIFIED., .F., .F.,
 ( 4, 2, 4 ),
 ( 2.872315617951276927E-05, 0.0004097954672334697037, 0.0007908677782874266957 ),
 .UNSPECIFIED. ) ;
#29788 = CARTESIAN_POINT ( 'NONE',  ( -53.72801162551947840, 5.497307881342318403, 1.430198536305348656 ) ) ;
#29789 = ORIENTED_EDGE ( 'NONE', *, *, #29999, .F. ) ;
#29790 = CARTESIAN_POINT ( 'NONE',  ( 0.6708088701982984903, 0.000000000000000000, -4.612695725900422872 ) ) ;
#29792 = VERTEX_POINT ( 'NONE', #7326 ) ;
#29791 = CARTESIAN_POINT ( 'NONE',  ( 102.3442017738903047, -2.858083093383076090, -3.998506272710563803 ) ) ;
#29793 = EDGE_CURVE ( 'NONE', #1782, #1418, #7670, .T. ) ;
#29794 = EDGE_LOOP ( 'NONE', ( #16990, #19116, #26070, #23736 ) ) ;
#29795 = EDGE_CURVE ( 'NONE', #12441, #6329, #24865, .T. ) ;
#29796 = FACE_OUTER_BOUND ( 'NONE', #25285, .T. ) ;
#29797 = CARTESIAN_POINT ( 'NONE',  ( 29.40513214801762842, -2.959508727822389940, 1.915219082070892531 ) ) ;
#29799 = EDGE_LOOP ( 'NONE', ( #20078, #20238, #16647 ) ) ;
#29798 = CARTESIAN_POINT ( 'NONE',  ( 25.75999999999999801, 2.788229309062804084, 1.188575764268269053 ) ) ;
#29800 = CARTESIAN_POINT ( 'NONE',  ( 25.75999999999999801, 5.999999999999997335, 0.000000000000000000 ) ) ;
#29801 = CARTESIAN_POINT ( 'NONE',  ( 22.42250000000000298, -2.378061970571983430, 1.291182301015471490 ) ) ;
#29802 = CARTESIAN_POINT ( 'NONE',  ( -4.059984658974702398, -5.088068716088551824, 1.745854725342557812 ) ) ;
#29803 = DIRECTION ( 'NONE',  ( 8.574039729943018344E-17, 1.000000000000000000, 0.000000000000000000 ) ) ;
#29805 = ORIENTED_EDGE ( 'NONE', *, *, #10190, .T. ) ;
#29804 = CARTESIAN_POINT ( 'NONE',  ( 107.4762276881066043, -17.74013139905899905, -5.017020369388183632 ) ) ;
#29806 = CARTESIAN_POINT ( 'NONE',  ( 4.749760686538667009, -7.892520144992426268, -1.391664247347309535 ) ) ;
#29807 = EDGE_CURVE ( 'NONE', #26246, #13763, #27215, .T. ) ;
#29808 = LINE ( 'NONE', #4217, #9682 ) ;
#29809 = CARTESIAN_POINT ( 'NONE',  ( 23.29750000136559862, -0.3178988483021076838, -3.024605502323848949 ) ) ;
#29810 = CARTESIAN_POINT ( 'NONE',  ( 107.3477133433398620, -15.88627905081428260, -1.500000000000000000 ) ) ;
#29811 = FACE_OUTER_BOUND ( 'NONE', #6182, .T. ) ;
#29812 = DIRECTION ( 'NONE',  ( 0.000000000000000000, 0.000000000000000000, 1.000000000000000000 ) ) ;
#29813 = ORIENTED_EDGE ( 'NONE', *, *, #29854, .T. ) ;
#29814 = LINE ( 'NONE', #25107, #10292 ) ;
#29815 = DIRECTION ( 'NONE',  ( 0.000000000000000000, -1.000000000000000000, 0.000000000000000000 ) ) ;
#29816 = LINE ( 'NONE', #6241, #28490 ) ;
#29817 = ORIENTED_EDGE ( 'NONE', *, *, #16834, .T. ) ;
#29818 = CARTESIAN_POINT ( 'NONE',  ( 8.917086725895012833, 0.3004441037763295186, -1.469409787067161410 ) ) ;
#29819 = ADVANCED_FACE ( 'NONE', ( #27891 ), #13163, .T. ) ;
#29820 = CARTESIAN_POINT ( 'NONE',  ( 3.086618293031875293, -0.003885106576443817308, -0.6225218429476583326 ) ) ;
#29821 = ORIENTED_EDGE ( 'NONE', *, *, #5859, .F. ) ;
#29822 = CARTESIAN_POINT ( 'NONE',  ( 7.167277592125206986, -6.432846314878395866, 1.000000000000000666 ) ) ;
#29823 = EDGE_CURVE ( 'NONE', #9887, #19305, #32673, .T. ) ;
#29824 = ORIENTED_EDGE ( 'NONE', *, *, #17433, .F. ) ;
#29825 = B_SPLINE_CURVE_WITH_KNOTS ( 'NONE', 3,
 ( #18330, #600, #28538, #31222, #18492, #3050, #214, #17561 ),
 .UNSPECIFIED., .F., .F.,
 ( 4, 2, 2, 4 ),
 ( 5.099451029798974806E-07, 0.001229190215600040655, 0.001843530350848571675, 0.002457870486097102694 ),
 .UNSPECIFIED. ) ;
#29826 = ORIENTED_EDGE ( 'NONE', *, *, #18528, .F. ) ;
#29827 = CYLINDRICAL_SURFACE ( 'NONE', #22548, 4.000000000000001776 ) ;
#29829 = VERTEX_POINT ( 'NONE', #12816 ) ;
#29828 = CARTESIAN_POINT ( 'NONE',  ( 0.9801757370192293317, 19.50000000000000000, -6.747923662139670320 ) ) ;
#29830 = ORIENTED_EDGE ( 'NONE', *, *, #1872, .T. ) ;
#29831 = CARTESIAN_POINT ( 'NONE',  ( 22.36000000136559507, 0.9349337715887185984, -3.156283516753368268 ) ) ;
#29832 = EDGE_CURVE ( 'NONE', #14230, #16163, #2648, .T. ) ;
#29833 = ORIENTED_EDGE ( 'NONE', *, *, #7417, .T. ) ;
#29834 = LINE ( 'NONE', #27315, #21437 ) ;
#29835 = DIRECTION ( 'NONE',  ( 1.000000000000000000, -0.000000000000000000, -0.000000000000000000 ) ) ;
#29837 = EDGE_LOOP ( 'NONE', ( #11348, #30874, #22209, #20749, #18714 ) ) ;
#29836 = CARTESIAN_POINT ( 'NONE',  ( 47.89262141173624343, -4.427686077581835633, -2.184956528778913221 ) ) ;
#29838 = DIRECTION ( 'NONE',  ( -1.000000000000000000, -0.000000000000000000, -0.000000000000000000 ) ) ;
#29839 = DIRECTION ( 'NONE',  ( 0.000000000000000000, 0.000000000000000000, -1.000000000000000000 ) ) ;
#29840 = CARTESIAN_POINT ( 'NONE',  ( 24.17250000136559507, -2.363507492473152283, -1.913930629741525280 ) ) ;
#29841 = CARTESIAN_POINT ( 'NONE',  ( 107.6300027436162310, -19.96576125925734502, 2.508990583257467044 ) ) ;
#29842 = EDGE_CURVE ( 'NONE', #12277, #32002, #14081, .T. ) ;
#29843 = CYLINDRICAL_SURFACE ( 'NONE', #17122, 4.000000000000001776 ) ;
#29844 = DIRECTION ( 'NONE',  ( 0.000000000000000000, 0.000000000000000000, 1.000000000000000000 ) ) ;
#29845 = CARTESIAN_POINT ( 'NONE',  ( 25.52557118915443723, -17.56218954043521308, 1.000000000000000888 ) ) ;
#29846 = DIRECTION ( 'NONE',  ( -0.9896144216807905014, -0.000000000000000000, -0.1437473352845003161 ) ) ;
#29847 = DIRECTION ( 'NONE',  ( 0.000000000000000000, 0.000000000000000000, -1.000000000000000000 ) ) ;
#29848 = DIRECTION ( 'NONE',  ( 0.000000000000000000, -0.2588190451025066396, -0.9659258262890719759 ) ) ;
#29849 = LINE ( 'NONE', #2449, #31628 ) ;
#29850 = CARTESIAN_POINT ( 'NONE',  ( -5.900050802731187538, 2.853674364686379583, 1.549418761218565921 ) ) ;
#29851 = VERTEX_POINT ( 'NONE', #18667 ) ;
#29852 = CARTESIAN_POINT ( 'NONE',  ( -3.050050800000000617, -2.853674364686378695, -1.549418761218566809 ) ) ;
#29853 = CARTESIAN_POINT ( 'NONE',  ( 21.64915922382874314, -21.84574418159160203, -1.293067337327047372 ) ) ;
#29854 = EDGE_CURVE ( 'NONE', #21409, #533, #31394, .T. ) ;
#29855 = CARTESIAN_POINT ( 'NONE',  ( -3.807304909706596519, -1.062355717592093463, -3.000000000000000888 ) ) ;
#29856 = VERTEX_POINT ( 'NONE', #20711 ) ;
#29857 = DIRECTION ( 'NONE',  ( -0.1736481776669307198, -2.126576849575776229E-17, -0.9848077530122080203 ) ) ;
#29858 = CARTESIAN_POINT ( 'NONE',  ( 16.05919002109104099, -15.28992581341303136, -1.499999999999999778 ) ) ;
#29859 = ORIENTED_EDGE ( 'NONE', *, *, #26877, .T. ) ;
#29860 = CARTESIAN_POINT ( 'NONE',  ( 17.32050807568873552, 10.00000000000002309, -1.500000000000000000 ) ) ;
#29861 = APPROVAL_DATE_TIME ( #6632, #30093 ) ;
#29862 = CARTESIAN_POINT ( 'NONE',  ( -2.650050800000000262, 2.853674364686379583, 1.549418761218565921 ) ) ;
#29863 = VERTEX_POINT ( 'NONE', #23702 ) ;
#29864 = CARTESIAN_POINT ( 'NONE',  ( 17.33093461831347781, -21.43932300456618378, 1.500000000000000000 ) ) ;
#29865 = AXIS2_PLACEMENT_3D ( 'NONE', #27499, #12445, #24972 ) ;
#29866 = CARTESIAN_POINT ( 'NONE',  ( 3.249999999999999556, 9.241976615262133876, 1.699438267350532161 ) ) ;
#29867 = CARTESIAN_POINT ( 'NONE',  ( 40.88222826850149261, -6.571667082171160246, -4.275175681037933550 ) ) ;
#29868 = CARTESIAN_POINT ( 'NONE',  ( 24.40342144122098134, -17.37878489514604041, -1.350270808451339510 ) ) ;
#29869 = DIRECTION ( 'NONE',  ( -1.000000000000000000, -0.000000000000000000, -0.000000000000000000 ) ) ;
#29870 = B_SPLINE_CURVE_WITH_KNOTS ( 'NONE', 3,
 ( #30935, #8011, #192, #25923 ),
 .UNSPECIFIED., .F., .F.,
 ( 4, 4 ),
 ( 0.002129256371650449509, 0.002522096907598464846 ),
 .UNSPECIFIED. ) ;
#29871 = ORIENTED_EDGE ( 'NONE', *, *, #8279, .F. ) ;
#29872 = LINE ( 'NONE', #3989, #5560 ) ;
#29873 = CARTESIAN_POINT ( 'NONE',  ( 107.3084207622235482, 16.37966385977266270, 1.508007899815985153 ) ) ;
#29874 = DIRECTION ( 'NONE',  ( -0.000000000000000000, -0.000000000000000000, -1.000000000000000000 ) ) ;
#29875 = EDGE_CURVE ( 'NONE', #21989, #24800, #25712, .T. ) ;
#29877 = ORIENTED_EDGE ( 'NONE', *, *, #4293, .T. ) ;
#29876 = DIRECTION ( 'NONE',  ( -1.000000000000000000, 0.000000000000000000, 0.000000000000000000 ) ) ;
#29878 = CARTESIAN_POINT ( 'NONE',  ( 6.530491241813344061, -8.637950316517745364, -0.6236753264480845438 ) ) ;
#29879 = DIRECTION ( 'NONE',  ( -0.000000000000000000, -0.000000000000000000, -1.000000000000000000 ) ) ;
#29880 = CARTESIAN_POINT ( 'NONE',  ( 5.377543748152548986, -4.007137495034764463, -6.940565734314639634 ) ) ;
#29881 = LINE ( 'NONE', #9133, #29426 ) ;
#29882 = CARTESIAN_POINT ( 'NONE',  ( 2.970200448039778784, -8.521880193013323890, 3.362738345035466647 ) ) ;
#29883 = CIRCLE ( 'NONE', #3213, 302.6457063863960002 ) ;
#29884 = CARTESIAN_POINT ( 'NONE',  ( -23.35000000000000142, -10.96966150227469505, -11.50000000000000000 ) ) ;
#29885 = CARTESIAN_POINT ( 'NONE',  ( 25.41905588447623643, -17.54124894465117279, -1.046314264356064117 ) ) ;
#29886 = DIRECTION ( 'NONE',  ( 0.000000000000000000, 0.000000000000000000, 1.000000000000000000 ) ) ;
#29887 = CARTESIAN_POINT ( 'NONE',  ( 17.33093461831353466, -21.43932300456619089, 1.949999999999999512 ) ) ;
#29888 = VECTOR ( 'NONE', #24138, 1000.000000000000114 ) ;
#29889 = VERTEX_POINT ( 'NONE', #30910 ) ;
#29890 = DIRECTION ( 'NONE',  ( -0.000000000000000000, 0.000000000000000000, 1.000000000000000000 ) ) ;
#29891 = VERTEX_POINT ( 'NONE', #28866 ) ;
#29892 = EDGE_CURVE ( 'NONE', #30559, #1994, #3726, .T. ) ;
#29893 = CARTESIAN_POINT ( 'NONE',  ( -5.804531657079157192, 1.883076972206379374, 2.325406398514293205 ) ) ;
#29894 = VECTOR ( 'NONE', #12979, 1000.000000000000000 ) ;
#29895 =( BOUNDED_CURVE ( )  B_SPLINE_CURVE ( 2, ( #26976, #11932, #4079, #19466, #18964, #14395, #6579, #9241, #16423, #29151, #18785 ),
 .UNSPECIFIED., .F., .F. ) 
 B_SPLINE_CURVE_WITH_KNOTS ( ( 3, 2, 2, 2, 2, 3 ),
 ( 0.3103822619934377136, 0.3125000000000000000, 0.3281250000000000000, 0.3437500000000000000, 0.3593750000000000000, 0.3728822619934377136 ),
 .UNSPECIFIED. ) 
 CURVE ( )  GEOMETRIC_REPRESENTATION_ITEM ( )  RATIONAL_B_SPLINE_CURVE ( ( 0.9821626249036857770, 0.9896829947469991673, 1.000000000000000000, 0.9238795325112867385, 1.000000000000000000, 0.9238795325112867385, 1.000000000000000000, 0.9238795325112867385, 1.000000000000000000, 0.9341965377642874602, 0.9821626249036857770 ) ) 
 REPRESENTATION_ITEM ( '' )  );
#29896 = LINE ( 'NONE', #32269, #11946 ) ;
#29897 = EDGE_CURVE ( 'NONE', #22155, #12070, #14474, .T. ) ;
#29898 = CARTESIAN_POINT ( 'NONE',  ( 85.20563808598666355, -3.194259795296103821, -4.522129901861162260 ) ) ;
#29899 = DIRECTION ( 'NONE',  ( 1.000000000000000000, -0.000000000000000000, -0.000000000000000000 ) ) ;
#29900 = CYLINDRICAL_SURFACE ( 'NONE', #16730, 4.000000000000000888 ) ;
#29901 = EDGE_LOOP ( 'NONE', ( #26495, #26469, #5175 ) ) ;
#29902 = DIRECTION ( 'NONE',  ( -1.000000000000000000, -0.000000000000000000, -0.000000000000000000 ) ) ;
#29903 = B_SPLINE_CURVE_WITH_KNOTS ( 'NONE', 3,
 ( #13494, #23226, #28393, #18523, #26214, #15696, #25902, #20560, #10657, #31080 ),
 .UNSPECIFIED., .F., .F.,
 ( 4, 2, 2, 2, 4 ),
 ( 2.493548413898819905E-07, 0.0005478513795029395141, 0.001095453404164489124, 0.001643055428826038734, 0.002190657453487588127 ),
 .UNSPECIFIED. ) ;
#29904 = ORIENTED_EDGE ( 'NONE', *, *, #19564, .T. ) ;
#29905 = PERSON_AND_ORGANIZATION ( #6766, #25292 ) ;
#29906 = CARTESIAN_POINT ( 'NONE',  ( 102.4228461758059581, -3.993355098355509281, 4.003574673590898136 ) ) ;
#29907 = VECTOR ( 'NONE', #28227, 1000.000000000000000 ) ;
#29908 = DIRECTION ( 'NONE',  ( 0.000000000000000000, 0.5735764363510558184, -0.8191520442889850262 ) ) ;
#29910 = LINE ( 'NONE', #6993, #20407 ) ;
#29909 = CARTESIAN_POINT ( 'NONE',  ( 5.489344087273877015, 6.152099123112526158, -5.297876218488255518 ) ) ;
#29911 = ORIENTED_EDGE ( 'NONE', *, *, #17541, .T. ) ;
#29912 = FACE_OUTER_BOUND ( 'NONE', #22253, .T. ) ;
#29913 = CYLINDRICAL_SURFACE ( 'NONE', #14994, 2.499999999999997780 ) ;
#29914 = CARTESIAN_POINT ( 'NONE',  ( 24.23499999999999943, 0.2613211581691317065, 2.486304738420681559 ) ) ;
#29915 = CARTESIAN_POINT ( 'NONE',  ( 0.8637286840862898885, -8.447112080008446711, -1.500000000000000444 ) ) ;
#29916 = AXIS2_PLACEMENT_3D ( 'NONE', #13407, #13252, #905 ) ;
#29918 = VERTEX_POINT ( 'NONE', #23519 ) ;
#29917 = CARTESIAN_POINT ( 'NONE',  ( 3.499999999999999556, -5.233522515400120589, 4.720195129223259123 ) ) ;
#29919 = CARTESIAN_POINT ( 'NONE',  ( -4.537550801365592967, -1.828967928396026510, 3.368539882008728004 ) ) ;
#29920 = CARTESIAN_POINT ( 'NONE',  ( 18.65791233782715963, -7.001076235476726417, 2.184956778830005497 ) ) ;
#29921 = CARTESIAN_POINT ( 'NONE',  ( 23.95058674323829706, -2.449331254355760823, 0.07017451552782173751 ) ) ;
#29922 = CARTESIAN_POINT ( 'NONE',  ( -2.619932554246537343E-16, -3.055657119358776264, -3.641590349731960163 ) ) ;
#29923 = VERTEX_POINT ( 'NONE', #2838 ) ;
#29924 = ORIENTED_EDGE ( 'NONE', *, *, #2889, .F. ) ;
#29925 = CARTESIAN_POINT ( 'NONE',  ( 11.68225172329192496, 4.861379696014986429, 1.500000000000000222 ) ) ;
#29926 = CARTESIAN_POINT ( 'NONE',  ( -50.81000000000000227, -10.96999999999998643, 1.500000000000000000 ) ) ;
#29927 = AXIS2_PLACEMENT_3D ( 'NONE', #19348, #1313, #24003 ) ;
#29928 = ADVANCED_FACE ( 'NONE', ( #324 ), #29704, .F. ) ;
#29929 = CARTESIAN_POINT ( 'NONE',  ( 24.36000000136559507, -1.570731468192933633, -2.892927487894330962 ) ) ;
#29930 = EDGE_CURVE ( 'NONE', #10433, #19561, #27305, .T. ) ;
#29931 = CIRCLE ( 'NONE', #19786, 2.999999999999999556 ) ;
#29932 = CARTESIAN_POINT ( 'NONE',  ( -50.81000000000000227, -10.96999999999998643, 5.500000000000000000 ) ) ;
#29933 = CARTESIAN_POINT ( 'NONE',  ( 11.75204077933772417, -19.94170559719522728, -1.750535629482800282 ) ) ;
#29934 = DIRECTION ( 'NONE',  ( 0.000000000000000000, 1.000000000000000000, 0.000000000000000000 ) ) ;
#29935 = AXIS2_PLACEMENT_3D ( 'NONE', #5209, #12878, #17920 ) ;
#29936 = CARTESIAN_POINT ( 'NONE',  ( 0.000000000000000000, 0.000000000000000000, 0.000000000000000000 ) ) ;
#29937 = CARTESIAN_POINT ( 'NONE',  ( 0.1606233661178074201, 7.854816391752183158, 7.161985370896712055 ) ) ;
#29938 = VERTEX_POINT ( 'NONE', #20019 ) ;
#29939 = AXIS2_PLACEMENT_3D ( 'NONE', #22512, #30054, #22696 ) ;
#29940 = DIRECTION ( 'NONE',  ( -0.000000000000000000, -0.000000000000000000, -1.000000000000000000 ) ) ;
#29941 = ORIENTED_EDGE ( 'NONE', *, *, #4425, .T. ) ;
#29942 = CIRCLE ( 'NONE', #5898, 8.750000000000000000 ) ;
#29943 = DIRECTION ( 'NONE',  ( -0.000000000000000000, -0.000000000000000000, -1.000000000000000000 ) ) ;
#29944 = CARTESIAN_POINT ( 'NONE',  ( 2.976845970491568405, 5.822399416825399854, -7.079702685456805256 ) ) ;
#29945 = ORIENTED_EDGE ( 'NONE', *, *, #29987, .T. ) ;
#29946 = CARTESIAN_POINT ( 'NONE',  ( 7.249760686538667009, 0.000000000000000000, 0.000000000000000000 ) ) ;
#29947 = ORIENTED_EDGE ( 'NONE', *, *, #26933, .T. ) ;
#29948 = CARTESIAN_POINT ( 'NONE',  ( -29.35000000000000853, -10.96966150227469505, -1.500000000000000000 ) ) ;
#29950 = ORIENTED_EDGE ( 'NONE', *, *, #8631, .T. ) ;
#29949 = CARTESIAN_POINT ( 'NONE',  ( 28.69270465004975890, -5.650360225335952613, -4.043900693839809435 ) ) ;
#29951 = B_SPLINE_CURVE_WITH_KNOTS ( 'NONE', 3,
 ( #18547, #26566, #31275, #8350, #28737, #16011, #30088, #26901 ),
 .UNSPECIFIED., .F., .F.,
 ( 4, 2, 2, 4 ),
 ( 5.099451029790481183E-07, 0.001229189590448580760, 0.001843529413121383674, 0.002457869235794186806 ),
 .UNSPECIFIED. ) ;
#29952 = VERTEX_POINT ( 'NONE', #7436 ) ;
#29953 = VECTOR ( 'NONE', #18144, 1000.000000000000000 ) ;
#29954 = EDGE_CURVE ( 'NONE', #2157, #8276, #18246, .T. ) ;
#29955 = CARTESIAN_POINT ( 'NONE',  ( 3.063284526839887167, -7.360373001730951437, 4.729683950898845524 ) ) ;
#29956 = TOROIDAL_SURFACE ( 'NONE', #15530, 300.0401151713995773, 0.8000000000000170308 ) ;
#29957 = AXIS2_PLACEMENT_3D ( 'NONE', #25188, #9976, #22351 ) ;
#29958 = FACE_OUTER_BOUND ( 'NONE', #26535, .T. ) ;
#29960 = EDGE_LOOP ( 'NONE', ( #8580, #4380, #23074, #18174 ) ) ;
#29959 = CARTESIAN_POINT ( 'NONE',  ( 7.382000898082563545, -19.12189044733477417, -1.499999999999998224 ) ) ;
#29961 = CARTESIAN_POINT ( 'NONE',  ( 24.29583315745070848, 18.19363606234995245, -1.499999999999882316 ) ) ;
#29962 = VECTOR ( 'NONE', #28397, 1000.000000000000000 ) ;
#29963 = DIRECTION ( 'NONE',  ( 4.917867153433014437E-17, 0.5735764363510474917, -0.8191520442889907994 ) ) ;
#29964 = CARTESIAN_POINT ( 'NONE',  ( -10.00000000000000000, 0.000000000000000000, 0.000000000000000000 ) ) ;
#29966 = ORIENTED_EDGE ( 'NONE', *, *, #4569, .F. ) ;
#29965 = CARTESIAN_POINT ( 'NONE',  ( 108.0278902883042633, -18.47097532996942348, -4.374628062554474006 ) ) ;
#29967 = CARTESIAN_POINT ( 'NONE',  ( 0.7632845268398871230, 0.000000000000000000, 0.000000000000000000 ) ) ;
#29968 = VECTOR ( 'NONE', #27260, 1000.000000000000000 ) ;
#29969 = EDGE_CURVE ( 'NONE', #30917, #14918, #29241, .T. ) ;
#29970 = CARTESIAN_POINT ( 'NONE',  ( 7.064632918400240769, -2.318425219014176974, -8.437262856154180923 ) ) ;
#29971 = LINE ( 'NONE', #24790, #25350 ) ;
#29972 = EDGE_CURVE ( 'NONE', #8056, #27353, #18512, .T. ) ;
#29973 = DIRECTION ( 'NONE',  ( -1.000000000000000000, 0.000000000000000000, -3.469446951953611033E-15 ) ) ;
#29974 = DIRECTION ( 'NONE',  ( 0.000000000000000000, 0.000000000000000000, 1.000000000000000000 ) ) ;
#29975 = DIRECTION ( 'NONE',  ( -1.000000000000000000, 0.000000000000000000, 0.000000000000000000 ) ) ;
#29976 = ORIENTED_EDGE ( 'NONE', *, *, #4387, .F. ) ;
#29977 = CARTESIAN_POINT ( 'NONE',  ( 10.52034268205830614, -3.641590349731950393, 3.055657119358789142 ) ) ;
#29978 = AXIS2_PLACEMENT_3D ( 'NONE', #2958, #30348, #7419 ) ;
#29979 = EDGE_CURVE ( 'NONE', #21128, #3186, #12364, .T. ) ;
#29980 = CARTESIAN_POINT ( 'NONE',  ( 25.75999999999999801, -2.208672634433321348E-15, 0.000000000000000000 ) ) ;
#29981 = CARTESIAN_POINT ( 'NONE',  ( -6.187550801365593323, -0.3701630799359326152, 3.521866450007987037 ) ) ;
#29982 = ORIENTED_EDGE ( 'NONE', *, *, #8164, .T. ) ;
#29983 = CIRCLE ( 'NONE', #6447, 5.000000000000003553 ) ;
#29984 = AXIS2_PLACEMENT_3D ( 'NONE', #19959, #12082, #4725 ) ;
#29985 = VECTOR ( 'NONE', #5747, 1000.000000000000114 ) ;
#29986 = PLANE ( 'NONE',  #22641 ) ;
#29987 = EDGE_CURVE ( 'NONE', #32838, #29709, #25352, .T. ) ;
#29988 = CARTESIAN_POINT ( 'NONE',  ( 3.527557386959558894, -11.88551672347146848, -0.9788672205888330202 ) ) ;
#29989 = ORIENTED_EDGE ( 'NONE', *, *, #5515, .F. ) ;
#29991 = CARTESIAN_POINT ( 'NONE',  ( 107.9638161812118256, 20.82655351785575348, 1.489452138568093664 ) ) ;
#29990 = AXIS2_PLACEMENT_3D ( 'NONE', #3238, #744, #25474 ) ;
#29992 = ORIENTED_EDGE ( 'NONE', *, *, #8279, .T. ) ;
#29993 = CIRCLE ( 'NONE', #28389, 3.750000000000000444 ) ;
#29994 = AXIS2_PLACEMENT_3D ( 'NONE', #3842, #4015, #32088 ) ;
#29995 = VERTEX_POINT ( 'NONE', #12627 ) ;
#29996 = CARTESIAN_POINT ( 'NONE',  ( 0.000000000000000000, 0.5174497483512452423, 7.981930256614262476 ) ) ;
#29998 = ORIENTED_EDGE ( 'NONE', *, *, #7097, .T. ) ;
#29997 = CARTESIAN_POINT ( 'NONE',  ( 56.97280603064898941, -277.2763395528616002, -1.491740999229418829 ) ) ;
#29999 = EDGE_CURVE ( 'NONE', #11786, #16905, #8641, .T. ) ;
#30000 = EDGE_LOOP ( 'NONE', ( #1920, #26341, #10380, #5527 ) ) ;
#30001 = CARTESIAN_POINT ( 'NONE',  ( 23.67250000136559507, 2.363507492473148286, 1.913930629741525058 ) ) ;
#30002 = EDGE_LOOP ( 'NONE', ( #15797, #9200, #4953, #30942, #20207, #15894 ) ) ;
#30003 = CARTESIAN_POINT ( 'NONE',  ( 0.08034252392848015289, -2.072171912280144301, 10.58792409793185207 ) ) ;
#30005 = ORIENTED_EDGE ( 'NONE', *, *, #24976, .F. ) ;
#30004 = CARTESIAN_POINT ( 'NONE',  ( 10.56870887191539587, 4.467071865485493731, -1.625881193364653088 ) ) ;
#30006 = DIRECTION ( 'NONE',  ( 7.472768010111444442E-18, 0.08715574274766196838, -0.9961946980917452121 ) ) ;
#30007 = B_SPLINE_CURVE_WITH_KNOTS ( 'NONE', 3,
 ( #31190, #5900, #13113, #25994, #7927, #20492, #28157, #79, #3101, #13412, #23632, #23313, #20653, #8418, #2760, #755, #16090, #15620, #12758, #5425, #20973, #28314, #13257, #25833, #31339, #26144, #8272, #10442, #5261, #15931, #10938, #5753, #18611, #15433, #2593, #23458, #416, #18464 ),
 .UNSPECIFIED., .F., .F.,
 ( 4, 2, 2, 2, 2, 2, 2, 2, 2, 2, 2, 2, 2, 2, 2, 2, 2, 2, 4 ),
 ( 1.067815302520814551E-18, 0.001916204205297452126, 0.003832408410594902951, 0.004790510513243628581, 0.005748612615892353776, 0.006706714718541078972, 0.007185765769865441570, 0.007664816821189803300, 0.008622918923838523292, 0.009581021026487241549, 0.01149722523178467806, 0.01245532733443339458, 0.01341342943708211284, 0.01532963364237954589, 0.01724583784767698066, 0.01916204205297441718, 0.02299445046356927980, 0.02682685887416414242, 0.03065926728475900503 ),
 .UNSPECIFIED. ) ;
#30008 = EDGE_CURVE ( 'NONE', #15630, #2062, #30536, .T. ) ;
#30009 = AXIS2_PLACEMENT_3D ( 'NONE', #29932, #24754, #27435 ) ;
#30010 = DIRECTION ( 'NONE',  ( 0.9993908270190957621, -0.03489949670250111491, 0.000000000000000000 ) ) ;
#30011 = CARTESIAN_POINT ( 'NONE',  ( 23.86000000136559507, -0.9349337715887248157, 3.156283516753367824 ) ) ;
#30012 = DIRECTION ( 'NONE',  ( 0.000000000000000000, 0.000000000000000000, 1.000000000000000000 ) ) ;
#30013 = AXIS2_PLACEMENT_3D ( 'NONE', #23984, #6129, #21506 ) ;
#30014 = CIRCLE ( 'NONE', #19870, 5.010000000000000675 ) ;
#30015 = AXIS2_PLACEMENT_3D ( 'NONE', #31444, #28929, #6034 ) ;
#30016 = CARTESIAN_POINT ( 'NONE',  ( 110.2779561444948939, -18.44184597392421665, -5.485967528433938867 ) ) ;
#30017 = CARTESIAN_POINT ( 'NONE',  ( 107.9116956367119116, -16.79780125263170376, -2.301619431082305489 ) ) ;
#30018 = PLANE ( 'NONE',  #18409 ) ;
#30019 = EDGE_CURVE ( 'NONE', #32242, #28214, #10779, .T. ) ;
#30020 = AXIS2_PLACEMENT_3D ( 'NONE', #25437, #2547, #7727 ) ;
#30021 = EDGE_CURVE ( 'NONE', #29668, #12740, #28527, .T. ) ;
#30022 = AXIS2_PLACEMENT_3D ( 'NONE', #160, #24191, #29063 ) ;
#30023 = FACE_OUTER_BOUND ( 'NONE', #25674, .T. ) ;
#30024 = CARTESIAN_POINT ( 'NONE',  ( 6.448894291898077391, -17.04229596238074862, 4.522129901861159595 ) ) ;
#30025 = LINE ( 'NONE', #4453, #30543 ) ;
#30026 = CARTESIAN_POINT ( 'NONE',  ( 41.19430503359171070, -3.886431767412232396, 0.07017451550800558879 ) ) ;
#30027 = CARTESIAN_POINT ( 'NONE',  ( 56.97280603064898941, -277.2763395528616002, 0.4463807625373157340 ) ) ;
#30028 = CARTESIAN_POINT ( 'NONE',  ( -2.050050802731187449, 2.331437884370912705, -1.887961173149511618 ) ) ;
#30029 = ORIENTED_EDGE ( 'NONE', *, *, #16828, .F. ) ;
#30030 = CARTESIAN_POINT ( 'NONE',  ( -4.700050800000001416, -2.983565686104819648, -0.3135853898029605791 ) ) ;
#30031 = AXIS2_PLACEMENT_3D ( 'NONE', #29980, #24443, #17280 ) ;
#30032 = DIRECTION ( 'NONE',  ( 0.000000000000000000, 0.2588190451025135785, 0.9659258262890703106 ) ) ;
#30033 = CARTESIAN_POINT ( 'NONE',  ( -4.162942409646514186, -5.022711880624455567E-15, 2.999999999999999556 ) ) ;
#30035 = VERTEX_POINT ( 'NONE', #590 ) ;
#30034 = VECTOR ( 'NONE', #2919, 1000.000000000000000 ) ;
#30036 = CARTESIAN_POINT ( 'NONE',  ( -1.762942409646513164, -5.022711880624455567E-15, 2.999999999999999556 ) ) ;
#30037 = FACE_OUTER_BOUND ( 'NONE', #26803, .T. ) ;
#30038 = AXIS2_PLACEMENT_3D ( 'NONE', #12454, #17619, #27661 ) ;
#30040 = EDGE_CURVE ( 'NONE', #10723, #979, #27888, .T. ) ;
#30039 = VECTOR ( 'NONE', #4412, 1000.000000000000000 ) ;
#30041 = AXIS2_PLACEMENT_3D ( 'NONE', #18873, #655, #1141 ) ;
#30042 = EDGE_LOOP ( 'NONE', ( #16360, #14099, #22419, #12015 ) ) ;
#30043 = CARTESIAN_POINT ( 'NONE',  ( 0.000000000000000000, 0.000000000000000000, 0.000000000000000000 ) ) ;
#30044 = APPROVAL_DATE_TIME ( #15301, #6550 ) ;
#30045 = AXIS2_PLACEMENT_3D ( 'NONE', #16264, #16411, #24280 ) ;
#30046 = CARTESIAN_POINT ( 'NONE',  ( 3.499999999999999556, -7.009698679648292519, 0.7308381473896670144 ) ) ;
#30047 = ORIENTED_EDGE ( 'NONE', *, *, #28410, .T. ) ;
#30048 = DIRECTION ( 'NONE',  ( 1.000000000000000000, -0.000000000000000000, -0.000000000000000000 ) ) ;
#30049 = AXIS2_PLACEMENT_3D ( 'NONE', #33070, #2145, #9840 ) ;
#30050 = ORIENTED_EDGE ( 'NONE', *, *, #3497, .F. ) ;
#30051 = LINE ( 'NONE', #27530, #18177 ) ;
#30052 = CARTESIAN_POINT ( 'NONE',  ( -6.512942406915326110, 3.284080845023683730E-15, 3.000000000000000000 ) ) ;
#30053 = FACE_OUTER_BOUND ( 'NONE', #10852, .T. ) ;
#30054 = DIRECTION ( 'NONE',  ( -1.000000000000000000, -0.000000000000000000, -0.000000000000000000 ) ) ;
#30055 = VERTEX_POINT ( 'NONE', #13274 ) ;
#30056 = EDGE_CURVE ( 'NONE', #20812, #5699, #18270, .T. ) ;
#30057 = DIRECTION ( 'NONE',  ( -3.469446951953478110E-15, 0.000000000000000000, 1.000000000000000000 ) ) ;
#30058 = CARTESIAN_POINT ( 'NONE',  ( -55.91000000000000369, -10.96999999999998643, 5.700000000000000178 ) ) ;
#30059 = AXIS2_PLACEMENT_3D ( 'NONE', #4021, #6681, #12032 ) ;
#30061 = EDGE_LOOP ( 'NONE', ( #20679, #13764, #9256, #6537 ) ) ;
#30060 = CARTESIAN_POINT ( 'NONE',  ( -3.350050802731187272, -0.3135853898029607456, 2.983565686104819648 ) ) ;
#30062 = AXIS2_PLACEMENT_3D ( 'NONE', #19306, #18988, #26825 ) ;
#30063 = CARTESIAN_POINT ( 'NONE',  ( 5.887529311434773760, -8.386653846779019261, -0.3723788567093603841 ) ) ;
#30064 = PRODUCT_DEFINITION_SHAPE ( 'NONE', 'NONE',  #33100 ) ;
#30065 = AXIS2_PLACEMENT_3D ( 'NONE', #27785, #5078, #12732 ) ;
#30066 = CARTESIAN_POINT ( 'NONE',  ( -3.529825581556942343E-16, -4.116875700062099241, 2.376879293651050329 ) ) ;
#30067 = DIRECTION ( 'NONE',  ( 1.000000000000000000, 0.000000000000000000, 0.000000000000000000 ) ) ;
#30068 = CARTESIAN_POINT ( 'NONE',  ( 0.5032039692148381205, 0.7352278974742033624, -9.704418393831362621 ) ) ;
#30069 = CARTESIAN_POINT ( 'NONE',  ( 101.6637436982523752, -2.056476561060098796, -2.639289249382372304 ) ) ;
#30070 = EDGE_CURVE ( 'NONE', #22634, #20949, #22013, .T. ) ;
#30071 = AXIS2_PLACEMENT_3D ( 'NONE', #29227, #6166, #29081 ) ;
#30072 = ADVANCED_FACE ( 'NONE', ( #5124 ), #23180, .T. ) ;
#30073 = AXIS2_PLACEMENT_3D ( 'NONE', #25609, #27473, #7745 ) ;
#30074 = VECTOR ( 'NONE', #28591, 999.9999999999998863 ) ;
#30075 = CARTESIAN_POINT ( 'NONE',  ( 1.394036994807660394E-16, 1.625881193364758337, -4.467071865485455540 ) ) ;
#30076 = DIRECTION ( 'NONE',  ( 0.000000000000000000, 0.000000000000000000, -1.000000000000000000 ) ) ;
#30077 = CARTESIAN_POINT ( 'NONE',  ( -56.32443066862174419, 0.3152581172270095267, -1.465964887886411550 ) ) ;
#30078 = LINE ( 'NONE', #15325, #29478 ) ;
#30079 = ORIENTED_EDGE ( 'NONE', *, *, #7324, .F. ) ;
#30080 = AXIS2_PLACEMENT_3D ( 'NONE', #1140, #19178, #29216 ) ;
#30081 = CIRCLE ( 'NONE', #32225, 6.250000000000000000 ) ;
#30082 = CARTESIAN_POINT ( 'NONE',  ( 6.038145077921538650, 2.472816103755249184, 8.106170535363455443 ) ) ;
#30083 = EDGE_LOOP ( 'NONE', ( #26949, #21542, #13690, #12372 ) ) ;
#30084 = AXIS2_PLACEMENT_3D ( 'NONE', #1935, #4438, #4245 ) ;
#30085 = CARTESIAN_POINT ( 'NONE',  ( -5.204531657079157547, 2.325406398514293205, -1.883076972206379374 ) ) ;
#30086 = CARTESIAN_POINT ( 'NONE',  ( -29.01811942205308270, 5.485000000000015419, 1.500000000000000000 ) ) ;
#30087 = FACE_OUTER_BOUND ( 'NONE', #29018, .T. ) ;
#30088 = CARTESIAN_POINT ( 'NONE',  ( 0.7212197595511946613, -8.936767016217507020, -0.5238431420100763125 ) ) ;
#30089 = PLANE ( 'NONE',  #712 ) ;
#30090 = ORIENTED_EDGE ( 'NONE', *, *, #20313, .T. ) ;
#30091 = CARTESIAN_POINT ( 'NONE',  ( 10.00000000000000178, 5.003758587302149508, 0.2500000000000014988 ) ) ;
#30092 = ADVANCED_FACE ( 'NONE', ( #15300 ), #25503, .T. ) ;
#30093 = APPROVAL ( #19342, 'UNSPECIFIED' ) ;
#30094 = CIRCLE ( 'NONE', #6561, 0.9999999999999991118 ) ;
#30095 = VERTEX_POINT ( 'NONE', #20818 ) ;
#30097 = CIRCLE ( 'NONE', #15661, 5.500000000000000000 ) ;
#30096 = APPLICATION_PROTOCOL_DEFINITION ( 'international standard', 'config_control_design', 1994, #15890 ) ;
#30098 = CARTESIAN_POINT ( 'NONE',  ( 28.66443557441545664, -6.752188475680952706, 4.013697994492946286 ) ) ;
#30099 = AXIS2_PLACEMENT_3D ( 'NONE', #2329, #10490, #23214 ) ;
#30100 = VECTOR ( 'NONE', #25028, 1000.000000000000000 ) ;
#30101 = CIRCLE ( 'NONE', #7123, 0.4499999999999990119 ) ;
#30102 = B_SPLINE_CURVE_WITH_KNOTS ( 'NONE', 3,
 ( #6607, #29515, #19137, #11611, #11288, #6763, #1585, #27150, #29327, #6264 ),
 .UNSPECIFIED., .F., .F.,
 ( 4, 3, 3, 4 ),
 ( 0.000000000000000000, 0.0005351973326734097130, 0.001070394665346821161, 0.002130599829429023241 ),
 .UNSPECIFIED. ) ;
#30103 = CYLINDRICAL_SURFACE ( 'NONE', #27242, 0.5000000000000004441 ) ;
#30105 = LINE ( 'NONE', #12340, #27861 ) ;
#30104 = CARTESIAN_POINT ( 'NONE',  ( 6.037141869538508843, 7.552970526864689838, 3.843044125430091107 ) ) ;
#30106 = EDGE_LOOP ( 'NONE', ( #31290, #3535, #24303 ) ) ;
#30107 = CC_DESIGN_SECURITY_CLASSIFICATION ( #7128, ( #12467 ) ) ;
#30108 = DIRECTION ( 'NONE',  ( 1.000000000000000000, -8.574039729943018344E-17, -0.000000000000000000 ) ) ;
#30109 = PLANE ( 'NONE',  #14439 ) ;
#30110 = EDGE_CURVE ( 'NONE', #6161, #14600, #23657, .T. ) ;
#30111 = CARTESIAN_POINT ( 'NONE',  ( 25.54750000136559507, 1.913930629741522838, -2.363507492473150062 ) ) ;
#30112 = CARTESIAN_POINT ( 'NONE',  ( 0.5496208378618945289, -7.013485574150957191, -1.500000000000000444 ) ) ;
#30114 = ORIENTED_EDGE ( 'NONE', *, *, #17940, .F. ) ;
#30113 = CARTESIAN_POINT ( 'NONE',  ( 0.3277201397524639459, -5.271209332775584677, 1.500000000000000444 ) ) ;
#30115 = CARTESIAN_POINT ( 'NONE',  ( -3.437550801365593767, -1.088641768524163389, -3.675193018007246071 ) ) ;
#30116 = CARTESIAN_POINT ( 'NONE',  ( 107.9617355966649654, 17.96508862869939094, -3.860795742263698482 ) ) ;
#30117 = DIRECTION ( 'NONE',  ( -7.770718973609008239E-17, -0.9063077870366540445, 0.4226182617406906705 ) ) ;
#30118 = CARTESIAN_POINT ( 'NONE',  ( 41.35220755422948713, -6.766095577561610952, -3.993434768848478367 ) ) ;
#30119 = ORIENTED_EDGE ( 'NONE', *, *, #17121, .F. ) ;
#30121 = ORIENTED_EDGE ( 'NONE', *, *, #6327, .T. ) ;
#30120 = CARTESIAN_POINT ( 'NONE',  ( 22.19921710918638880, -17.00655848932612102, 1.494769569001483500 ) ) ;
#30122 =( BOUNDED_CURVE ( )  B_SPLINE_CURVE ( 2, ( #30033, #22325, #27834, #9605, #9444, #17324, #17135, #12282, #27344, #29855, #27669 ),
 .UNSPECIFIED., .F., .F. ) 
 B_SPLINE_CURVE_WITH_KNOTS ( ( 3, 2, 2, 2, 2, 3 ),
 ( 0.5603822619934377691, 0.5625000000000000000, 0.5781250000000000000, 0.5937500000000000000, 0.6093750000000000000, 0.6228822619934377691 ),
 .UNSPECIFIED. ) 
 CURVE ( )  GEOMETRIC_REPRESENTATION_ITEM ( )  RATIONAL_B_SPLINE_CURVE ( ( 0.9821626249036861100, 0.9896829947469995004, 1.000000000000000000, 0.9238795325112867385, 1.000000000000000000, 0.9238795325112867385, 1.000000000000000000, 0.9238795325112867385, 1.000000000000000000, 0.9341965377642872381, 0.9821626249036861100 ) ) 
 REPRESENTATION_ITEM ( '' )  );
#30123 = AXIS2_PLACEMENT_3D ( 'NONE', #5896, #6083, #11426 ) ;
#30124 = CARTESIAN_POINT ( 'NONE',  ( 0.000000000000000000, -1.471047635026914380, 6.892461014225956362 ) ) ;
#30125 = DIRECTION ( 'NONE',  ( -1.000000000000000000, 0.000000000000000000, -0.000000000000000000 ) ) ;
#30126 = AXIS2_PLACEMENT_3D ( 'NONE', #28817, #8284, #18794 ) ;
#30127 = CARTESIAN_POINT ( 'NONE',  ( -16.85110191150524273, 12.14507408406953637, 1.499999999999892975 ) ) ;
#30128 = CARTESIAN_POINT ( 'NONE',  ( -25.41317123495344177, 18.70748839123610452, 1.500000000000000000 ) ) ;
#30129 = CARTESIAN_POINT ( 'NONE',  ( 15.95505886943986518, -20.93460726762247504, -1.499999999986860511 ) ) ;
#30130 = LINE ( 'NONE', #24756, #31154 ) ;
#30131 = APPROVAL_PERSON_ORGANIZATION ( #2501, #25149, #20209 ) ;
#30132 = CARTESIAN_POINT ( 'NONE',  ( 47.89262141172610399, -4.427686077581428847, 2.184956528777964202 ) ) ;
#30133 = LINE ( 'NONE', #25574, #29559 ) ;
#30134 = ORIENTED_EDGE ( 'NONE', *, *, #32934, .T. ) ;
#30135 = CARTESIAN_POINT ( 'NONE',  ( 101.7221769401408551, -2.897900707893039662, 3.993434276071444078 ) ) ;
#30136 = ORIENTED_EDGE ( 'NONE', *, *, #18186, .T. ) ;
#30137 = DIRECTION ( 'NONE',  ( -0.1027947991993878180, 0.9947025833170221043, 0.000000000000000000 ) ) ;
#30138 = DIRECTION ( 'NONE',  ( 0.000000000000000000, 0.000000000000000000, 1.000000000000000000 ) ) ;
#30139 = CARTESIAN_POINT ( 'NONE',  ( 3.499999999999999556, 2.429606751577119805, -5.757344182232886354 ) ) ;
#30140 = ORIENTED_EDGE ( 'NONE', *, *, #32311, .T. ) ;
#30141 = AXIS2_PLACEMENT_3D ( 'NONE', #30384, #32564, #7455 ) ;
#30142 = CARTESIAN_POINT ( 'NONE',  ( 108.0843732272301736, 18.64798334617831799, -4.598824503537998432 ) ) ;
#30143 = ORIENTED_EDGE ( 'NONE', *, *, #31997, .T. ) ;
#30144 = DIRECTION ( 'NONE',  ( -0.000000000000000000, 0.000000000000000000, 1.000000000000000000 ) ) ;
#30146 = VERTEX_POINT ( 'NONE', #7797 ) ;
#30145 = CARTESIAN_POINT ( 'NONE',  ( 18.85875575654547021, -4.756049901768979460, -4.023790192995878812 ) ) ;
#30147 = EDGE_LOOP ( 'NONE', ( #20048, #589 ) ) ;
#30148 = EDGE_CURVE ( 'NONE', #16254, #17299, #668, .T. ) ;
#30149 = DIRECTION ( 'NONE',  ( -1.000000000000000000, 0.000000000000000000, 0.000000000000000000 ) ) ;
#30150 = ADVANCED_FACE ( 'NONE', ( #22986 ), #16896, .T. ) ;
#30151 = DIRECTION ( 'NONE',  ( -0.7822388118548815328, 0.4516257885949861439, -0.4291113938172932962 ) ) ;
#30153 = ORIENTED_EDGE ( 'NONE', *, *, #2829, .F. ) ;
#30152 = CARTESIAN_POINT ( 'NONE',  ( 107.3615104199937775, -16.08547161712497697, 1.908459023709874636 ) ) ;
#30154 = CARTESIAN_POINT ( 'NONE',  ( 6.880159396099833735, 4.949130873693378341, 7.192972099401642616 ) ) ;
#30155 = CARTESIAN_POINT ( 'NONE',  ( 8.870145747188287189, 0.000000000000000000, -1.000000000000002220 ) ) ;
#30156 = ADVANCED_FACE ( 'NONE', ( #8435 ), #13671, .F. ) ;
#30157 = CARTESIAN_POINT ( 'NONE',  ( 7.249760686538667009, -3.647351267791625773, 7.953573330858203505 ) ) ;
#30158 = APPROVAL_PERSON_ORGANIZATION ( #17098, #28809, #24309 ) ;
#30159 = CARTESIAN_POINT ( 'NONE',  ( 2.357329994281668117, 10.64078702437731749, -2.053141773251354163 ) ) ;
#30161 = ORIENTED_EDGE ( 'NONE', *, *, #3348, .F. ) ;
#30160 = CARTESIAN_POINT ( 'NONE',  ( 107.9987586186765327, -18.05148653437722217, -4.627286608547184876 ) ) ;
#30162 = DIRECTION ( 'NONE',  ( -8.541412920197222280E-17, -0.9961946980917462113, 0.08715574274765119922 ) ) ;
#30163 = LINE ( 'NONE', #14895, #17180 ) ;
#30164 = CARTESIAN_POINT ( 'NONE',  ( 23.48500000136559862, 2.892927487894327410, -1.570731468192931635 ) ) ;
#30165 = CARTESIAN_POINT ( 'NONE',  ( 108.4602224094683010, 20.74085989589152845, -1.474553323550922723 ) ) ;
#30166 = DIRECTION ( 'NONE',  ( 0.000000000000000000, 1.000000000000000000, 0.000000000000000000 ) ) ;
#30167 = DIRECTION ( 'NONE',  ( -1.000000000000000000, 0.000000000000000000, 0.000000000000000000 ) ) ;
#30168 = CIRCLE ( 'NONE', #15728, 2.999999999999999112 ) ;
#30169 = ORIENTED_EDGE ( 'NONE', *, *, #14855, .F. ) ;
#30170 = CARTESIAN_POINT ( 'NONE',  ( 5.489321676144490958, -4.149060317827554023, 6.978593840069431842 ) ) ;
#30171 = CARTESIAN_POINT ( 'NONE',  ( 3.499999999999999556, -7.009698679648281860, -0.7308381473897611613 ) ) ;
#30172 = CARTESIAN_POINT ( 'NONE',  ( -7.487550801365594033, -2.228590825266444586, -2.752080473201636401 ) ) ;
#30173 = ORIENTED_EDGE ( 'NONE', *, *, #11171, .T. ) ;
#30174 = DIRECTION ( 'NONE',  ( -1.000000000000000000, 0.000000000000000000, 0.000000000000000000 ) ) ;
#30175 = CARTESIAN_POINT ( 'NONE',  ( 3.048228882235557879, 0.5389963249801591472, -1.289664751349871574 ) ) ;
#30176 = EDGE_LOOP ( 'NONE', ( #18105, #8093, #27201 ) ) ;
#30177 = CARTESIAN_POINT ( 'NONE',  ( 2.632061376486628301, -0.5000000000000000000, -1.500000000000000000 ) ) ;
#30178 = ORIENTED_EDGE ( 'NONE', *, *, #12098, .F. ) ;
#30179 = EDGE_CURVE ( 'NONE', #30672, #7133, #23816, .T. ) ;
#30180 = ORIENTED_EDGE ( 'NONE', *, *, #29484, .T. ) ;
#30181 = DIRECTION ( 'NONE',  ( -1.000000000000000000, 8.574039729943022041E-17, -1.232595164407830946E-32 ) ) ;
#30183 = ORIENTED_EDGE ( 'NONE', *, *, #31283, .T. ) ;
#30182 = CARTESIAN_POINT ( 'NONE',  ( 3.499999999999999556, 5.904264776415128146, -2.046865518294647579 ) ) ;
#30184 = ORIENTED_EDGE ( 'NONE', *, *, #26707, .T. ) ;
#30185 = CARTESIAN_POINT ( 'NONE',  ( 20.98500000136559862, -2.892927487894331406, 1.570731468192932523 ) ) ;
#30186 = EDGE_LOOP ( 'NONE', ( #3040, #1795, #31202, #28085 ) ) ;
#30187 = CARTESIAN_POINT ( 'NONE',  ( 0.08034253207385326501, 9.783802610460172744, -4.547003328335167183 ) ) ;
#30188 = AXIS2_PLACEMENT_3D ( 'NONE', #8570, #16272, #20268 ) ;
#30190 = ORIENTED_EDGE ( 'NONE', *, *, #10994, .T. ) ;
#30189 = PLANE ( 'NONE',  #10683 ) ;
#30191 = DIRECTION ( 'NONE',  ( 0.000000000000000000, 0.000000000000000000, 1.000000000000000000 ) ) ;
#30192 = CARTESIAN_POINT ( 'NONE',  ( 48.09670199522223299, -9.430894477028838097, 0.07017451552781736601 ) ) ;
#30193 = FACE_OUTER_BOUND ( 'NONE', #11326, .T. ) ;
#30194 = CARTESIAN_POINT ( 'NONE',  ( 10.00000000000000000, 1.946309384392590491, 4.616489984850538519 ) ) ;
#30195 = DIRECTION ( 'NONE',  ( 1.000000000000000000, 0.000000000000000000, 0.000000000000000000 ) ) ;
#30196 = CARTESIAN_POINT ( 'NONE',  ( 25.52557090713405685, -17.56218951387322491, 1.057622280107608725 ) ) ;
#30197 = LINE ( 'NONE', #22315, #13930 ) ;
#30198 = CARTESIAN_POINT ( 'NONE',  ( 41.20585001718148277, -8.497180311781159290, 0.02339150517593243869 ) ) ;
#30199 = CARTESIAN_POINT ( 'NONE',  ( 3.499999999999999556, 1.459547570502368385, 6.894905428400277536 ) ) ;
#30200 = CARTESIAN_POINT ( 'NONE',  ( 41.19430503359171780, -3.886431767412232841, -0.07017451552781628354 ) ) ;
#30201 = CARTESIAN_POINT ( 'NONE',  ( 34.48223484310472031, 0.5000000000000000000, -2.999999999999997335 ) ) ;
#30202 = EDGE_CURVE ( 'NONE', #31589, #11659, #13760, .T. ) ;
#30203 = CARTESIAN_POINT ( 'NONE',  ( -2.150050802731187538, 0.3135853898029611342, -2.983565686104819648 ) ) ;
#30204 = VERTEX_POINT ( 'NONE', #9072 ) ;
#30205 = CARTESIAN_POINT ( 'NONE',  ( -2.500050800000000351, -0.3135853898029607456, 2.983565686104819648 ) ) ;
#30206 = EDGE_CURVE ( 'NONE', #24760, #25632, #12496, .T. ) ;
#30207 = CARTESIAN_POINT ( 'NONE',  ( 0.6791198108364597807, 3.345077512921651675, 8.522429291907608118 ) ) ;
#30208 = CARTESIAN_POINT ( 'NONE',  ( -4.200050800000000528, 1.887961173149511618, 2.331437884370912705 ) ) ;
#30209 = ORIENTED_EDGE ( 'NONE', *, *, #6930, .T. ) ;
#30210 = DIRECTION ( 'NONE',  ( 7.770718973608956470E-17, 0.9063077870366479383, 0.4226182617407038267 ) ) ;
#30211 = VERTEX_POINT ( 'NONE', #14257 ) ;
#30212 = CARTESIAN_POINT ( 'NONE',  ( 101.7264006491823949, -2.958721067365122082, -4.091315454812116670 ) ) ;
#30213 = COORDINATED_UNIVERSAL_TIME_OFFSET ( 0, 0, .AHEAD. ) ;
#30214 = CARTESIAN_POINT ( 'NONE',  ( -2.386718424894566315, -9.330009425477193474, -4.522129901861166701 ) ) ;
#30216 = EDGE_CURVE ( 'NONE', #25185, #13681, #8771, .T. ) ;
#30215 = VERTEX_POINT ( 'NONE', #31357 ) ;
#30217 = CARTESIAN_POINT ( 'NONE',  ( 40.87773210426689019, -5.748708618950156612, 3.993433839950368824 ) ) ;
#30218 = ADVANCED_FACE ( 'NONE', ( #13610 ), #32355, .F. ) ;
#30219 = VERTEX_POINT ( 'NONE', #29996 ) ;
#30220 = DIRECTION ( 'NONE',  ( -0.000000000000000000, -0.9961946980917449901, -0.08715574274766567375 ) ) ;
#30221 = FACE_OUTER_BOUND ( 'NONE', #14925, .T. ) ;
#30222 = DIRECTION ( 'NONE',  ( 1.000000000000000000, -0.000000000000000000, 0.000000000000000000 ) ) ;
#30223 = FACE_OUTER_BOUND ( 'NONE', #18948, .T. ) ;
#30224 = VERTEX_POINT ( 'NONE', #17293 ) ;
#30225 = APPLICATION_CONTEXT ( 'configuration controlled 3d designs of mechanical parts and assemblies' ) ;
#30226 = DIRECTION ( 'NONE',  ( 1.000000000000000000, 0.000000000000000000, 0.000000000000000000 ) ) ;
#30227 = ADVANCED_FACE ( 'NONE', ( #24963 ), #29827, .T. ) ;
#30228 = CARTESIAN_POINT ( 'NONE',  ( 0.000000000000000000, 4.438567988583181467, -7.249076783337631724 ) ) ;
#30230 = ORIENTED_EDGE ( 'NONE', *, *, #16946, .T. ) ;
#30229 = CARTESIAN_POINT ( 'NONE',  ( 7.249760686538667009, 0.000000000000000000, 0.000000000000000000 ) ) ;
#30231 = DIRECTION ( 'NONE',  ( -1.000000000000000000, 0.000000000000000000, -0.000000000000000000 ) ) ;
#30232 = CARTESIAN_POINT ( 'NONE',  ( -31.91713028529358098, -0.0003384977252905707612, 2.028141679950118625 ) ) ;
#30233 = CARTESIAN_POINT ( 'NONE',  ( 47.62814091865205768, 23.65599663307499512, -4.612695725900423760 ) ) ;
#30234 = CARTESIAN_POINT ( 'NONE',  ( 101.6441386174529384, -1.774168274679073454, -2.184956718804114573 ) ) ;
#30235 = EDGE_CURVE ( 'NONE', #12555, #13277, #19880, .T. ) ;
#30236 = DIRECTION ( 'NONE',  ( 0.000000000000000000, 0.000000000000000000, -1.000000000000000000 ) ) ;
#30237 = LINE ( 'NONE', #6658, #20910 ) ;
#30238 = CARTESIAN_POINT ( 'NONE',  ( -56.28386703554979675, 2.926702260634249026E-12, -1.039475297285789024 ) ) ;
#30240 = CARTESIAN_POINT ( 'NONE',  ( 23.09498300328107590, -21.93193249238093756, 1.086362660086114929 ) ) ;
#30239 = UNCERTAINTY_MEASURE_WITH_UNIT (LENGTH_MEASURE( 1.000000000000000082E-05 ), #7794, 'distance_accuracy_value', 'NONE');
#30241 = VERTEX_POINT ( 'NONE', #32852 ) ;
#30242 = CARTESIAN_POINT ( 'NONE',  ( -7.212550801365592790, 1.828967928396027176, -3.368539882008727115 ) ) ;
#30243 = ORIENTED_EDGE ( 'NONE', *, *, #20393, .F. ) ;
#30244 = CARTESIAN_POINT ( 'NONE',  ( -7.754531657079159146, -0.9198621039125872700, -3.105402419394638791 ) ) ;
#30245 = CARTESIAN_POINT ( 'NONE',  ( 4.749760686538667009, 5.151476664237558900, -6.139290821770204687 ) ) ;
#30246 = CARTESIAN_POINT ( 'NONE',  ( 107.7918428252582146, -20.44935860102534875, 1.500028854543402845 ) ) ;
#30247 = CARTESIAN_POINT ( 'NONE',  ( 0.2603629172483717391, -5.188755369436605314, 1.768970845646744561 ) ) ;
#30248 = DIRECTION ( 'NONE',  ( 0.000000000000000000, 0.000000000000000000, 1.000000000000000000 ) ) ;
#30249 = ORIENTED_EDGE ( 'NONE', *, *, #10067, .T. ) ;
#30250 = DIRECTION ( 'NONE',  ( -1.000000000000000000, 8.574039729943022041E-17, -1.232595164407830946E-32 ) ) ;
#30251 = ORIENTED_EDGE ( 'NONE', *, *, #23507, .F. ) ;
#30252 = CARTESIAN_POINT ( 'NONE',  ( 6.524595623740805372, -5.074779492939337722, 7.015943501182377418 ) ) ;
#30253 = COORDINATED_UNIVERSAL_TIME_OFFSET ( 0, 0, .AHEAD. ) ;
#30254 = EDGE_CURVE ( 'NONE', #15147, #14743, #11321, .T. ) ;
#30255 = CARTESIAN_POINT ( 'NONE',  ( 40.88397857810694092, -6.894206476317448207, 3.997238040198453302 ) ) ;
#30256 = ADVANCED_FACE ( 'NONE', ( #17597 ), #1928, .F. ) ;
#30257 = CARTESIAN_POINT ( 'NONE',  ( 10.57125986779756843, -1.115095498423276155, -4.884328206559847452 ) ) ;
#30259 = DIRECTION ( 'NONE',  ( 0.000000000000000000, 0.000000000000000000, -1.000000000000000000 ) ) ;
#30258 = CARTESIAN_POINT ( 'NONE',  ( 0.1606233164486133569, 9.238724727304104434, -5.257199111574238692 ) ) ;
#30260 = EDGE_LOOP ( 'NONE', ( #10916, #5757, #8476, #2941 ) ) ;
#30261 = EDGE_CURVE ( 'NONE', #4026, #292, #22297, .T. ) ;
#30262 = DIRECTION ( 'NONE',  ( 1.000000000000000000, -8.574039729943018344E-17, -0.000000000000000000 ) ) ;
#30263 = DIRECTION ( 'NONE',  ( -1.000000000000000000, 0.000000000000000000, 0.000000000000000000 ) ) ;
#30264 = CARTESIAN_POINT ( 'NONE',  ( 25.48500000136559862, 0.9349337715887185984, -3.156283516753368268 ) ) ;
#30265 = CARTESIAN_POINT ( 'NONE',  ( 0.5636839040845996740, -7.175910112258415019, -1.499999999999999556 ) ) ;
#30267 = ORIENTED_EDGE ( 'NONE', *, *, #21218, .F. ) ;
#30266 = CARTESIAN_POINT ( 'NONE',  ( 5.612974044843318744, 8.123783100924566014, -1.229732182294818621 ) ) ;
#30268 = CARTESIAN_POINT ( 'NONE',  ( -3.837550801365593234, 1.088641768524161613, 3.675193018007247403 ) ) ;
#30269 = CARTESIAN_POINT ( 'NONE',  ( 107.9166481000539193, 17.71402365689241520, -3.323306282662723543 ) ) ;
#30270 = DIRECTION ( 'NONE',  ( 1.000000000000000000, -0.000000000000000000, -0.000000000000000000 ) ) ;
#30271 = CARTESIAN_POINT ( 'NONE',  ( 22.24290772321994325, 0.1310194482076003919, 2.499999999999998668 ) ) ;
#30272 = EDGE_LOOP ( 'NONE', ( #14737, #26172, #19045, #5469 ) ) ;
#30274 = ORIENTED_EDGE ( 'NONE', *, *, #30465, .F. ) ;
#30273 = CARTESIAN_POINT ( 'NONE',  ( 22.17497728449718863, -17.32537947343248064, 1.743178009048999444 ) ) ;
#30275 = EDGE_CURVE ( 'NONE', #5926, #6901, #14915, .T. ) ;
#30276 = CARTESIAN_POINT ( 'NONE',  ( 9.513773624275961183, 1.351470648933397412, 1.500000000000000222 ) ) ;
#30277 = DIRECTION ( 'NONE',  ( 0.000000000000000000, -9.769962616701377556E-15, 1.000000000000000000 ) ) ;
#30278 = CARTESIAN_POINT ( 'NONE',  ( 24.11000000136559507, -2.892927487894331406, 1.570731468192932523 ) ) ;
#30279 = CARTESIAN_POINT ( 'NONE',  ( 102.2915521900159206, -2.105775436102748532, 2.787782622540901478 ) ) ;
#30280 = CARTESIAN_POINT ( 'NONE',  ( -3.111251654333415217, -11.33182932643446605, -1.500000000000000222 ) ) ;
#30281 = CARTESIAN_POINT ( 'NONE',  ( 5.489321676144490958, 6.978593840069445164, 4.149060317827530042 ) ) ;
#30282 = CARTESIAN_POINT ( 'NONE',  ( -1.750050802731187405, -0.3135853898029607456, 2.983565686104819648 ) ) ;
#30283 = CARTESIAN_POINT ( 'NONE',  ( 0.6728002192067888965, 7.058361986476102246, 5.823680980834201826 ) ) ;
#30284 = VERTEX_POINT ( 'NONE', #25124 ) ;
#30285 = DIRECTION ( 'NONE',  ( 0.000000000000000000, 0.000000000000000000, 1.000000000000000000 ) ) ;
#30286 = EDGE_CURVE ( 'NONE', #32504, #28422, #24620, .T. ) ;
#30287 = PERSON_AND_ORGANIZATION ( #6766, #25292 ) ;
#30288 = CARTESIAN_POINT ( 'NONE',  ( 19.01480233880980819, -3.011762293215293429, -0.07017451552781921176 ) ) ;
#30289 = EDGE_LOOP ( 'NONE', ( #8807, #15654, #2030, #16225 ) ) ;
#30290 = CARTESIAN_POINT ( 'NONE',  ( 10.00000000000000178, 3.672404558090038851, 3.407865132560194521 ) ) ;
#30291 = ORIENTED_EDGE ( 'NONE', *, *, #9757, .T. ) ;
#30292 = CARTESIAN_POINT ( 'NONE',  ( -4.599999999999996092, 0.000000000000000000, 0.000000000000000000 ) ) ;
#30294 = ORIENTED_EDGE ( 'NONE', *, *, #22432, .T. ) ;
#30293 = CARTESIAN_POINT ( 'NONE',  ( 54.94574350846487221, -5.369113455210825947, -4.008637379614919283 ) ) ;
#30295 = ORIENTED_EDGE ( 'NONE', *, *, #18703, .F. ) ;
#30296 = DIRECTION ( 'NONE',  ( 0.000000000000000000, -0.4226182617406961661, -0.9063077870366516020 ) ) ;
#30297 = LINE ( 'NONE', #22767, #12399 ) ;
#30298 = CARTESIAN_POINT ( 'NONE',  ( 47.98568197278773795, -2.821418575600919354, 1.010822989962091301 ) ) ;
#30300 = ORIENTED_EDGE ( 'NONE', *, *, #1635, .T. ) ;
#30299 = CARTESIAN_POINT ( 'NONE',  ( 3.529825581556927552E-16, 4.116875700062083254, 2.376879293651078751 ) ) ;
#30301 = DIRECTION ( 'NONE',  ( 0.000000000000000000, 0.000000000000000000, -1.000000000000000000 ) ) ;
#30302 = CARTESIAN_POINT ( 'NONE',  ( -50.81000000000000227, -10.96999999999998643, 1.499999999999999556 ) ) ;
#30303 = B_SPLINE_CURVE_WITH_KNOTS ( 'NONE', 3,
 ( #6352, #1197, #11394, #11549, #24072, #31626, #3700, #18929 ),
 .UNSPECIFIED., .F., .F.,
 ( 4, 2, 2, 4 ),
 ( 2.737843117464296545E-07, 0.001228034957219389283, 0.001841915543673210576, 0.002455796130127032087 ),
 .UNSPECIFIED. ) ;
#30304 = B_SPLINE_CURVE_WITH_KNOTS ( 'NONE', 3,
 ( #724, #16249, #6210, #11064, #31317, #8393, #18589, #28778 ),
 .UNSPECIFIED., .F., .F.,
 ( 4, 2, 2, 4 ),
 ( 0.009524646911531632620, 0.5047623234557656602, 0.7523811617278828301, 1.000000000000000000 ),
 .UNSPECIFIED. ) ;
#30305 = CARTESIAN_POINT ( 'NONE',  ( 6.883866557622099869, -3.625395379390139894, 7.943335131954991191 ) ) ;
#30306 = CARTESIAN_POINT ( 'NONE',  ( 5.865515302491369987, 15.00000000000000178, 1.508259000770582059 ) ) ;
#30308 = VERTEX_POINT ( 'NONE', #9753 ) ;
#30307 = CARTESIAN_POINT ( 'NONE',  ( 107.5620888422228205, -18.98815586165099845, -4.509679481931270217 ) ) ;
#30309 = CARTESIAN_POINT ( 'NONE',  ( 107.8806307222008627, -16.35047421165092985, 1.384330804614037236 ) ) ;
#30310 = LINE ( 'NONE', #20117, #23059 ) ;
#30311 = CARTESIAN_POINT ( 'NONE',  ( 23.73500000136559152, 1.570731468192929858, 2.892927487894329186 ) ) ;
#30312 = CARTESIAN_POINT ( 'NONE',  ( 107.3476950949991959, -15.88628029827230570, -1.500000000000000000 ) ) ;
#30313 = DIRECTION ( 'NONE',  ( 0.000000000000000000, 0.000000000000000000, -1.000000000000000000 ) ) ;
#30314 = CARTESIAN_POINT ( 'NONE',  ( 26.13024263984378592, 21.17433810686643980, 4.621439243524390506 ) ) ;
#30315 = ORIENTED_EDGE ( 'NONE', *, *, #26427, .F. ) ;
#30316 = CYLINDRICAL_SURFACE ( 'NONE', #21514, 12.49867430706168570 ) ;
#30317 = B_SPLINE_CURVE_WITH_KNOTS ( 'NONE', 3,
 ( #25867, #18493, #30737, #12978, #23493, #31223, #23192, #10473, #25515, #15656, #2984, #10626, #15158 ),
 .UNSPECIFIED., .F., .F.,
 ( 4, 3, 3, 3, 4 ),
 ( 8.673617379884035472E-19, 0.0002877298135619251536, 0.001654640778973444316, 0.002565914753109074971, 0.003274339315400769980 ),
 .UNSPECIFIED. ) ;
#30318 = CARTESIAN_POINT ( 'NONE',  ( 10.52034268205830259, 3.055657119358849094, -3.641590349731898879 ) ) ;
#30319 = CARTESIAN_POINT ( 'NONE',  ( -7.687550801365593323, -2.752080473201636845, 2.228590825266444586 ) ) ;
#30320 = ORIENTED_EDGE ( 'NONE', *, *, #31875, .F. ) ;
#30321 = EDGE_CURVE ( 'NONE', #13159, #3186, #32508, .T. ) ;
#30322 =( BOUNDED_SURFACE ( )  B_SPLINE_SURFACE ( 3, 2, ( 
 ( #29845, #27656, #10090 ),
 ( #30196, #17458, #25486 ),
 ( #17616, #15119, #12119 ),
 ( #25142, #32525, #15282 ),
 ( #25332, #12268, #33018 ),
 ( #27819, #32376, #4936 ),
 ( #28009, #2442, #2265 ),
 ( #12450, #12612, #7269 ),
 ( #32695, #22666, #4761 ),
 ( #22813, #20306, #9775 ) ),
 .UNSPECIFIED., .F., .F., .F. ) 
 B_SPLINE_SURFACE_WITH_KNOTS ( ( 4, 2, 2, 2, 4 ),
 ( 3, 3 ),
 ( 0.01348603581695214694, 0.01365687529133369216, 0.01382771476571523911, 0.01416939371447832954, 0.01485275161200451215 ),
 ( 0.000000000000000000, 1.000000000000000000 ),
 .UNSPECIFIED. ) 
 GEOMETRIC_REPRESENTATION_ITEM ( )  RATIONAL_B_SPLINE_SURFACE ( (
 ( 1.000000000000000000, 0.9948736491435667961, 1.000000000000000000),
 ( 1.000000000000000000, 0.9948794564610410340, 1.000000000000000000),
 ( 1.000000000000000000, 0.9935082075948730163, 1.000000000000000000),
 ( 1.000000000000000000, 0.9898246045859987463, 1.000000000000000000),
 ( 1.000000000000000000, 0.9875779995959915736, 1.000000000000000000),
 ( 1.000000000000000000, 0.9804235948789852273, 1.000000000000000000),
 ( 1.000000000000000000, 0.9752522326727456337, 1.000000000000000000),
 ( 1.000000000000000000, 0.9593679678194060312, 1.000000000000000000),
 ( 1.000000000000000000, 0.9482314950094890005, 1.000000000000000000),
 ( 1.000000000000000000, 0.9372872368324467462, 1.000000000000000000) ) ) 
 REPRESENTATION_ITEM ( '' )  SURFACE ( )  );
#30323 = CARTESIAN_POINT ( 'NONE',  ( -5.756376981307136376, -0.1572233378491221800, 3.000000000000000000 ) ) ;
#30324 = EDGE_CURVE ( 'NONE', #901, #4009, #4590, .T. ) ;
#30325 = DIRECTION ( 'NONE',  ( -0.9816271834476639757, 0.000000000000000000, 0.1908089953765452762 ) ) ;
#30326 = CARTESIAN_POINT ( 'NONE',  ( 3.750263394063806821, -2.684783475528570995E-05, -0.9948185799301207943 ) ) ;
#30327 = ORIENTED_EDGE ( 'NONE', *, *, #15383, .T. ) ;
#30328 = CARTESIAN_POINT ( 'NONE',  ( 18.51491971917340607, -8.599446730134173933, -0.07017451552783579571 ) ) ;
#30329 = ORIENTED_EDGE ( 'NONE', *, *, #9978, .F. ) ;
#30330 = LINE ( 'NONE', #17595, #24018 ) ;
#30331 = ORIENTED_EDGE ( 'NONE', *, *, #10190, .F. ) ;
#30332 = CARTESIAN_POINT ( 'NONE',  ( -2.983877251335061320, -0.2474135948681125963, 1.436677650513773274 ) ) ;
#30333 = PRODUCT ( 'Part7_handle1Sleeve', 'Part7_handle1Sleeve', '', ( #5805 ) ) ;
#30335 = ORIENTED_EDGE ( 'NONE', *, *, #14129, .F. ) ;
#30334 = CARTESIAN_POINT ( 'NONE',  ( 10.56870887191539587, -4.616489984850518979, -1.946309384392639119 ) ) ;
#30336 = ORIENTED_EDGE ( 'NONE', *, *, #2119, .T. ) ;
#30337 = DIRECTION ( 'NONE',  ( 0.000000000000000000, -0.9271838545667856479, -0.3746065934159164001 ) ) ;
#30338 = VERTEX_POINT ( 'NONE', #14765 ) ;
#30339 = DIRECTION ( 'NONE',  ( 1.000000000000000000, 0.000000000000000000, -0.000000000000000000 ) ) ;
#30341 = ORIENTED_EDGE ( 'NONE', *, *, #7758, .T. ) ;
#30340 = CARTESIAN_POINT ( 'NONE',  ( 17.32050807568873552, 10.00000000000002309, 4.629213727441584325 ) ) ;
#30342 = CARTESIAN_POINT ( 'NONE',  ( -5.450050799999999640, -2.853674364686378695, -1.549418761218566809 ) ) ;
#30343 = DIRECTION ( 'NONE',  ( 0.04710975479914572550, 0.5265925107009689077, 0.8488115212910427587 ) ) ;
#30344 = CARTESIAN_POINT ( 'NONE',  ( 108.0945118936045191, -19.43030987200927839, 3.536500079626898163 ) ) ;
#30345 = DIRECTION ( 'NONE',  ( -1.000000000000000000, 0.000000000000000000, -0.000000000000000000 ) ) ;
#30346 = DIRECTION ( 'NONE',  ( -0.000000000000000000, -0.000000000000000000, 1.000000000000000000 ) ) ;
#30347 = FACE_OUTER_BOUND ( 'NONE', #12055, .T. ) ;
#30348 = DIRECTION ( 'NONE',  ( 1.000000000000000000, -8.574039729943018344E-17, -0.000000000000000000 ) ) ;
#30349 = CARTESIAN_POINT ( 'NONE',  ( 18.60402535543785518, -7.603424548862136589, -0.02339150517595086839 ) ) ;
#30350 = CARTESIAN_POINT ( 'NONE',  ( 5.489343806296448136, 8.012901424861411215, 1.307372367723665940 ) ) ;
#30351 = CARTESIAN_POINT ( 'NONE',  ( 19.01480233880806381, -3.011762293215138886, 0.02339150516273075936 ) ) ;
#30352 = ADVANCED_FACE ( 'NONE', ( #4428 ), #9923, .T. ) ;
#30353 = CYLINDRICAL_SURFACE ( 'NONE', #19890, 3.000000000000000444 ) ;
#30354 = EDGE_CURVE ( 'NONE', #22866, #12952, #4916, .T. ) ;
#30355 = CARTESIAN_POINT ( 'NONE',  ( -2.500050802731187627, -1.549418761218565477, 2.853674364686380471 ) ) ;
#30356 = ORIENTED_EDGE ( 'NONE', *, *, #1191, .F. ) ;
#30357 = ADVANCED_FACE ( 'NONE', ( #17444 ), #5390, .F. ) ;
#30358 = CARTESIAN_POINT ( 'NONE',  ( -3.100050800000000439, -2.983565686104819648, -0.3135853898029605791 ) ) ;
#30359 = CARTESIAN_POINT ( 'NONE',  ( 33.81874022276149816, 19.50000000000000000, 1.818740222761736192 ) ) ;
#30360 = CARTESIAN_POINT ( 'NONE',  ( 7.249760686538667009, -8.711672189281420842, -0.8180878109962766986 ) ) ;
#30361 = VERTEX_POINT ( 'NONE', #10251 ) ;
#30362 = CARTESIAN_POINT ( 'NONE',  ( 56.97280603064898941, -277.2763395528616002, -1.491740999229418829 ) ) ;
#30363 = CARTESIAN_POINT ( 'NONE',  ( 2.661997627134203626, 7.629706518865846832, 6.664939678585187544 ) ) ;
#30364 = CARTESIAN_POINT ( 'NONE',  ( 107.4539122023615221, -17.41608652575267158, 4.650537122213327379 ) ) ;
#30365 = ORIENTED_EDGE ( 'NONE', *, *, #18827, .F. ) ;
#30366 = CARTESIAN_POINT ( 'NONE',  ( 7.214127126792253542, -13.85184692375858617, 1.500000000000140332 ) ) ;
#30367 = CALENDAR_DATE ( 2026, 6, 10 ) ;
#30368 = FACE_OUTER_BOUND ( 'NONE', #31593, .T. ) ;
#30369 = VERTEX_POINT ( 'NONE', #20950 ) ;
#30370 = CARTESIAN_POINT ( 'NONE',  ( -3.790520337094915870, -3.338398410437402042, 1.747101600989292791 ) ) ;
#30371 = EDGE_LOOP ( 'NONE', ( #94, #32627, #17414, #30586 ) ) ;
#30372 = CARTESIAN_POINT ( 'NONE',  ( 101.8797206818349821, -5.166491396337139719, -2.184956718990371805 ) ) ;
#30374 = EDGE_LOOP ( 'NONE', ( #23621, #4200, #29111 ) ) ;
#30373 = CARTESIAN_POINT ( 'NONE',  ( 0.7632845268398871230, -8.152713396088739017, -3.174628368996162298 ) ) ;
#30375 = DIRECTION ( 'NONE',  ( 1.000000000000000000, -0.000000000000000000, -0.000000000000000000 ) ) ;
#30376 = DIRECTION ( 'NONE',  ( 0.000000000000000000, 1.000000000000000000, 0.000000000000000000 ) ) ;
#30377 = FACE_OUTER_BOUND ( 'NONE', #24548, .T. ) ;
#30378 = DIRECTION ( 'NONE',  ( -8.541412920197213652E-17, -0.9961946980917453232, -0.08715574274766135776 ) ) ;
#30379 = VERTEX_POINT ( 'NONE', #20472 ) ;
#30380 = EDGE_CURVE ( 'NONE', #30476, #11874, #176, .T. ) ;
#30381 = FACE_BOUND ( 'NONE', #29097, .T. ) ;
#30382 = CARTESIAN_POINT ( 'NONE',  ( 10.56870887191539587, -1.625881193364728805, 4.467071865485467086 ) ) ;
#30383 = CARTESIAN_POINT ( 'NONE',  ( 0.5640491561247281682, 0.6680154998105966024, -9.516580665849634357 ) ) ;
#30384 = CARTESIAN_POINT ( 'NONE',  ( 12.44989959798868817, 20.00000000000000000, 13.00000000000004441 ) ) ;
#30385 = EDGE_CURVE ( 'NONE', #15360, #19057, #3701, .T. ) ;
#30386 = CARTESIAN_POINT ( 'NONE',  ( 6.524595126109738352, -0.8869162863045095824, 8.613374939462822510 ) ) ;
#30387 = DIRECTION ( 'NONE',  ( 4.917867153433085927E-17, 0.5735764363510558184, -0.8191520442889850262 ) ) ;
#30388 = CARTESIAN_POINT ( 'NONE',  ( -56.29416256380356032, 0.02368334168385285987, -1.154763663137946761 ) ) ;
#30389 = CARTESIAN_POINT ( 'NONE',  ( 23.14329945973256031, -21.92788238883854390, 1.164089052066326069 ) ) ;
#30390 = ORIENTED_EDGE ( 'NONE', *, *, #15583, .T. ) ;
#30391 = CARTESIAN_POINT ( 'NONE',  ( -8.012550801365593500, 1.828967928396027176, -3.368539882008727115 ) ) ;
#30392 = ORIENTED_EDGE ( 'NONE', *, *, #23394, .F. ) ;
#30393 = CARTESIAN_POINT ( 'NONE',  ( -5.554531657079158080, -3.105402419394638791, 0.9198621039125867149 ) ) ;
#30394 = CARTESIAN_POINT ( 'NONE',  ( 21.67250000136559507, 3.024605502323846729, -0.3178988483021056854 ) ) ;
#30395 = EDGE_CURVE ( 'NONE', #28862, #4581, #20876, .T. ) ;
#30396 = DIRECTION ( 'NONE',  ( -0.9842544651762054064, 0.1767573132311699990, 0.000000000000000000 ) ) ;
#30397 = CARTESIAN_POINT ( 'NONE',  ( 3.744708216408842549, 0.000000000000000000, -1.000000000000000000 ) ) ;
#30398 = CARTESIAN_POINT ( 'NONE',  ( 108.3696618535068126, 20.23658298680886958, 1.395260099363828665 ) ) ;
#30399 = VERTEX_POINT ( 'NONE', #2578 ) ;
#30400 = CYLINDRICAL_SURFACE ( 'NONE', #30049, 2.999999999999999112 ) ;
#30401 = DIRECTION ( 'NONE',  ( 0.000000000000000000, 0.000000000000000000, 1.000000000000000000 ) ) ;
#30402 = ORIENTED_EDGE ( 'NONE', *, *, #9562, .F. ) ;
#30403 = CARTESIAN_POINT ( 'NONE',  ( 5.489344087273876127, -5.138668362895322694, 6.285690376021081605 ) ) ;
#30404 = APPROVAL_DATE_TIME ( #9996, #25149 ) ;
#30405 = EDGE_CURVE ( 'NONE', #26914, #23785, #546, .T. ) ;
#30406 = CARTESIAN_POINT ( 'NONE',  ( 102.4223857194505882, -3.986708129022342728, 4.013697985697794124 ) ) ;
#30407 = DIRECTION ( 'NONE',  ( -1.000000000000000000, 8.574039729943019576E-17, 0.000000000000000000 ) ) ;
#30409 = CARTESIAN_POINT ( 'NONE',  ( 5.885541416630536204, -0.3712256868991837266, -8.385500676968934641 ) ) ;
#30408 = CARTESIAN_POINT ( 'NONE',  ( 109.1350892577483620, 18.84131025325909548, -5.127064439618892244 ) ) ;
#30410 = VERTEX_POINT ( 'NONE', #18100 ) ;
#30411 = CARTESIAN_POINT ( 'NONE',  ( 0.000000000000000000, 1.975651141462391402, -10.82112760146734054 ) ) ;
#30412 = DIRECTION ( 'NONE',  ( -2.219124775575025560E-17, -0.2588190451025318972, 0.9659258262890653146 ) ) ;
#30413 = CARTESIAN_POINT ( 'NONE',  ( 22.54750000136559507, 1.913930629741522838, -2.363507492473150062 ) ) ;
#30414 = CARTESIAN_POINT ( 'NONE',  ( -50.60000000000000142, -10.96966150227468972, 7.500000000000000000 ) ) ;
#30416 = VERTEX_POINT ( 'NONE', #23296 ) ;
#30415 = CARTESIAN_POINT ( 'NONE',  ( 1.278428506419904798, -2.392608122357158251, 1.500000000000000444 ) ) ;
#30417 = CARTESIAN_POINT ( 'NONE',  ( -4.562550801365594211, 2.228590825266444142, 2.752080473201636845 ) ) ;
#30418 = DIRECTION ( 'NONE',  ( 1.000000000000000000, -8.574039729943018344E-17, -0.000000000000000000 ) ) ;
#30419 = CIRCLE ( 'NONE', #535, 0.5000000000000003331 ) ;
#30420 = EDGE_CURVE ( 'NONE', #26576, #29348, #9716, .T. ) ;
#30421 = LINE ( 'NONE', #5026, #6513 ) ;
#30422 = FACE_BOUND ( 'NONE', #27689, .T. ) ;
#30423 = VERTEX_POINT ( 'NONE', #18273 ) ;
#30425 = ORIENTED_EDGE ( 'NONE', *, *, #12206, .T. ) ;
#30424 = CARTESIAN_POINT ( 'NONE',  ( 3.499999999999999556, -5.848742439617962141, 6.167836887840967286 ) ) ;
#30426 = VECTOR ( 'NONE', #13452, 1000.000000000000000 ) ;
#30427 = CYLINDRICAL_SURFACE ( 'NONE', #23547, 0.5000000000000000000 ) ;
#30428 = CARTESIAN_POINT ( 'NONE',  ( 26.50087866478441256, 17.58784721092444769, 0.4463807625373157340 ) ) ;
#30429 = ADVANCED_FACE ( 'NONE', ( #28484 ), #28642, .T. ) ;
#30430 = EDGE_CURVE ( 'NONE', #15369, #29650, #15914, .T. ) ;
#30431 = CARTESIAN_POINT ( 'NONE',  ( 23.42250000136559862, -0.3178988483021076838, -3.024605502323848949 ) ) ;
#30432 = CARTESIAN_POINT ( 'NONE',  ( 54.92448458018063917, -4.608697703007766933, 2.787782628545061314 ) ) ;
#30433 = CARTESIAN_POINT ( 'NONE',  ( -2.938251396093196632, -11.64407820748950861, -1.500000000000079714 ) ) ;
#30434 = CARTESIAN_POINT ( 'NONE',  ( 25.17249999999999233, 1.291182301015473710, 2.378061970571975436 ) ) ;
#30435 = DIRECTION ( 'NONE',  ( -3.623545766764170865E-17, -0.4226182617406944453, -0.9063077870366522681 ) ) ;
#30436 = CARTESIAN_POINT ( 'NONE',  ( 107.4514419172558064, -17.38041855283238135, 4.563595182964964359 ) ) ;
#30437 = ORIENTED_EDGE ( 'NONE', *, *, #1883, .T. ) ;
#30438 = EDGE_CURVE ( 'NONE', #3978, #27203, #8401, .T. ) ;
#30439 = CARTESIAN_POINT ( 'NONE',  ( 0.2582728410551998199, -8.984109560031233954, 5.239665997526856245 ) ) ;
#30440 = AXIS2_PLACEMENT_3D ( 'NONE', #25414, #22895, #14589 ) ;
#30441 = AXIS2_PLACEMENT_3D ( 'NONE', #14916, #10076, #20288 ) ;
#30442 = DATE_AND_TIME ( #23251, #13530 ) ;
#30443 = LINE ( 'NONE', #9527, #7521 ) ;
#30444 = ORIENTED_EDGE ( 'NONE', *, *, #30216, .F. ) ;
#30445 = ADVANCED_FACE ( 'NONE', ( #31965 ), #10920, .F. ) ;
#30446 = TOROIDAL_SURFACE ( 'NONE', #1607, 3.895301350492843540, 15.00000000000000178 ) ;
#30447 = CARTESIAN_POINT ( 'NONE',  ( 107.4480564796146780, 17.91338030753361465, -4.728172914300420970 ) ) ;
#30448 = ORIENTED_EDGE ( 'NONE', *, *, #22165, .F. ) ;
#30449 = CARTESIAN_POINT ( 'NONE',  ( 0.000000000000000000, 0.000000000000000000, 0.000000000000000000 ) ) ;
#30451 = ORIENTED_EDGE ( 'NONE', *, *, #21248, .T. ) ;
#30450 = CARTESIAN_POINT ( 'NONE',  ( 84.96817173929643729, -4.101265922145543641, -4.053846905880101659 ) ) ;
#30452 = ORIENTED_EDGE ( 'NONE', *, *, #6966, .F. ) ;
#30453 = CARTESIAN_POINT ( 'NONE',  ( 18.53175858344379634, -21.44524224917989130, -1.500000000000000000 ) ) ;
#30454 = DIRECTION ( 'NONE',  ( -0.000000000000000000, -0.000000000000000000, -1.000000000000000000 ) ) ;
#30455 = DIRECTION ( 'NONE',  ( 0.000000000000000000, 0.000000000000000000, 1.000000000000000000 ) ) ;
#30456 = CARTESIAN_POINT ( 'NONE',  ( 107.5820849072354832, -19.27577136381270151, -3.923241656623378315 ) ) ;
#30458 = ORIENTED_EDGE ( 'NONE', *, *, #2458, .F. ) ;
#30457 = DIRECTION ( 'NONE',  ( -1.000000000000000000, 8.574039729943019576E-17, -0.000000000000000000 ) ) ;
#30459 = CARTESIAN_POINT ( 'NONE',  ( 7.249760686538667009, -6.147671362329260702, 6.226446564517894799 ) ) ;
#30460 = DIRECTION ( 'NONE',  ( 0.000000000000000000, 0.000000000000000000, -1.000000000000000000 ) ) ;
#30461 = CARTESIAN_POINT ( 'NONE',  ( -1.397981246020602697, -14.12199645988578212, 1.500000000000000444 ) ) ;
#30462 = CARTESIAN_POINT ( 'NONE',  ( 2.976845726615124921, 8.871766062375177953, -2.305279507610514145 ) ) ;
#30465 = EDGE_CURVE ( 'NONE', #14398, #27971, #26288, .T. ) ;
#30464 = ORIENTED_EDGE ( 'NONE', *, *, #11602, .F. ) ;
#30463 = CARTESIAN_POINT ( 'NONE',  ( 108.0618756673665501, -18.96035633396743592, -4.492382516429220374 ) ) ;
#30466 = CARTESIAN_POINT ( 'NONE',  ( 7.249760686538667009, -5.151476664237518044, 6.139290821770238438 ) ) ;
#30467 = AXIS2_PLACEMENT_3D ( 'NONE', #24200, #1322, #21692 ) ;
#30468 = VECTOR ( 'NONE', #9894, 999.9999999999998863 ) ;
#30469 = CARTESIAN_POINT ( 'NONE',  ( 10.56870887191539587, -4.467071865485462645, -1.625881193364742572 ) ) ;
#30470 = CARTESIAN_POINT ( 'NONE',  ( 25.61000000136559507, 3.156283516753366047, 0.9349337715887203748 ) ) ;
#30471 = ADVANCED_FACE ( 'NONE', ( #21431 ), #13879, .T. ) ;
#30472 = DIRECTION ( 'NONE',  ( -0.8528685319524442754, 0.4924038765061022893, 0.1736481776669307198 ) ) ;
#30473 = CARTESIAN_POINT ( 'NONE',  ( -14.62340757463330654, -21.93932300455827900, -1.000000000000000000 ) ) ;
#30474 = CARTESIAN_POINT ( 'NONE',  ( 0.000000000000000000, -9.620177616657944242, -5.227991826304196010 ) ) ;
#30475 = VECTOR ( 'NONE', #23294, 1000.000000000000000 ) ;
#30476 = VERTEX_POINT ( 'NONE', #24089 ) ;
#30477 = CARTESIAN_POINT ( 'NONE',  ( 7.249760686538667009, -4.973063321323927255, 7.199384779417104419 ) ) ;
#30478 = DIRECTION ( 'NONE',  ( -1.000000000000000000, 0.000000000000000000, 0.000000000000000000 ) ) ;
#30479 = CARTESIAN_POINT ( 'NONE',  ( -6.937550801365595099, -1.828967928396026732, 3.368539882008728004 ) ) ;
#30480 = VERTEX_POINT ( 'NONE', #3410 ) ;
#30481 = B_SPLINE_CURVE_WITH_KNOTS ( 'NONE', 3,
 ( #8366, #28755, #1007, #31438, #18418, #13540, #11190, #20911, #10697, #21397, #6189, #13063, #21092, #3539, #28444, #5844, #3374, #13358, #31293, #26092, #28921, #28609, #8693, #26440, #5554, #18562, #11040, #21240, #6026, #25770, #23569, #23264 ),
 .UNSPECIFIED., .F., .F.,
 ( 4, 2, 2, 2, 2, 2, 2, 2, 2, 2, 2, 2, 2, 2, 2, 4 ),
 ( 0.001762511593127062031, 0.004900820851275785282, 0.008039130109424507883, 0.01117743936757322962, 0.01274659399664759482, 0.01353117131118477742, 0.01431574862572196176, 0.01588490325479632870, 0.01666948056933351824, 0.01745405788387070084, 0.01823863519840788344, 0.01902321251294506951, 0.02059236714201943125, 0.02216152177109378951, 0.02373067640016815125, 0.02686898565831688165 ),
 .UNSPECIFIED. ) ;
#30482 = ADVANCED_FACE ( 'NONE', ( #18595 ), #23611, .T. ) ;
#30483 = CARTESIAN_POINT ( 'NONE',  ( 25.42231079161887308, 2.505942517978533957, 1.022343137445100636 ) ) ;
#30484 = AXIS2_PLACEMENT_3D ( 'NONE', #11868, #32102, #16877 ) ;
#30485 = DIRECTION ( 'NONE',  ( -1.000000000000000000, -0.000000000000000000, -0.000000000000000000 ) ) ;
#30486 = CARTESIAN_POINT ( 'NONE',  ( 5.885541416630534428, -8.385500676968931089, 0.3712256868992730441 ) ) ;
#30487 = ORIENTED_EDGE ( 'NONE', *, *, #19096, .T. ) ;
#30488 = CARTESIAN_POINT ( 'NONE',  ( 85.49734435724840864, -7.913007294147472059, -0.07017451552783579571 ) ) ;
#30489 = ORIENTED_EDGE ( 'NONE', *, *, #25545, .T. ) ;
#30491 = EDGE_CURVE ( 'NONE', #13510, #18680, #7311, .T. ) ;
#30490 = AXIS2_PLACEMENT_3D ( 'NONE', #4884, #15065, #2910 ) ;
#30492 = CC_DESIGN_PERSON_AND_ORGANIZATION_ASSIGNMENT ( #26247, #5690, ( #23132 ) ) ;
#30493 = CARTESIAN_POINT ( 'NONE',  ( -40.96572980946567100, -13.73075632567362980, 5.760101628985244915 ) ) ;
#30494 = AXIS2_PLACEMENT_3D ( 'NONE', #12140, #9967, #17644 ) ;
#30495 = ORIENTED_EDGE ( 'NONE', *, *, #9566, .T. ) ;
#30496 = CARTESIAN_POINT ( 'NONE',  ( 107.4616526958865705, -17.52838469296580826, 4.846942987312949924 ) ) ;
#30498 = ORIENTED_EDGE ( 'NONE', *, *, #10837, .F. ) ;
#30497 = FACE_OUTER_BOUND ( 'NONE', #4437, .T. ) ;
#30499 = ORIENTED_EDGE ( 'NONE', *, *, #19635, .F. ) ;
#30500 = CARTESIAN_POINT ( 'NONE',  ( 4.749760686538667009, 8.014274990069656823, -8.669741416787380218E-17 ) ) ;
#30501 = VERTEX_POINT ( 'NONE', #29280 ) ;
#30503 = AXIS2_PLACEMENT_3D ( 'NONE', #29946, #24770, #7036 ) ;
#30502 = CARTESIAN_POINT ( 'NONE',  ( 0.5704036742842228946, 8.851103337321323039, -3.563415854978401853 ) ) ;
#30504 = B_SPLINE_CURVE_WITH_KNOTS ( 'NONE', 3,
 ( #32201, #8786, #31707, #16449, #6419, #19309, #32014, #18990, #24635, #29177, #9270, #16804 ),
 .UNSPECIFIED., .F., .F.,
 ( 4, 2, 2, 2, 2, 4 ),
 ( 2.983873419563917522E-05, 0.0001332968301352377373, 0.0002367549260748362994, 0.0004436711179540329085, 0.0006505873098332294905, 0.0008575035017124260726 ),
 .UNSPECIFIED. ) ;
#30506 = ORIENTED_EDGE ( 'NONE', *, *, #27126, .T. ) ;
#30505 = CARTESIAN_POINT ( 'NONE',  ( 18.86894852475868589, -4.642115209765685258, 3.841991646160189955 ) ) ;
#30507 = CARTESIAN_POINT ( 'NONE',  ( -56.33578448492038859, 0.003046479527603615251, -1.001959257668779690 ) ) ;
#30508 = CARTESIAN_POINT ( 'NONE',  ( 22.90158751868999332, -21.92087667321502309, -1.135468510342512394 ) ) ;
#30509 = CYLINDRICAL_SURFACE ( 'NONE', #6940, 4.000000000000001776 ) ;
#30510 = LINE ( 'NONE', #12263, #9805 ) ;
#30511 = ADVANCED_FACE ( 'NONE', ( #28784 ), #16136, .T. ) ;
#30512 = ADVANCED_FACE ( 'NONE', ( #16559, #26467 ), #21125, .F. ) ;
#30513 = AXIS2_PLACEMENT_3D ( 'NONE', #15968, #3958, #8938 ) ;
#30514 = DIRECTION ( 'NONE',  ( -1.000000000000000000, 0.000000000000000000, 6.938893903907221278E-15 ) ) ;
#30515 = DIRECTION ( 'NONE',  ( -0.1437473352844943209, 0.000000000000000000, 0.9896144216807913896 ) ) ;
#30516 = FACE_OUTER_BOUND ( 'NONE', #7999, .T. ) ;
#30517 = CIRCLE ( 'NONE', #27821, 2.999999999999999112 ) ;
#30518 = AXIS2_PLACEMENT_3D ( 'NONE', #3655, #13811, #24017 ) ;
#30519 = CARTESIAN_POINT ( 'NONE',  ( -3.659776827757759587, -1.633636780108321807, 0.9788672205877712029 ) ) ;
#30520 = DIRECTION ( 'NONE',  ( -1.000000000000000000, 8.574039729943018344E-17, -0.000000000000000000 ) ) ;
#30521 = FACE_OUTER_BOUND ( 'NONE', #8884, .T. ) ;
#30522 = CARTESIAN_POINT ( 'NONE',  ( 109.4831014662949258, 20.77917954950597235, 0.7764623220122568448 ) ) ;
#30523 = VECTOR ( 'NONE', #31401, 1000.000000000000000 ) ;
#30524 =( BOUNDED_SURFACE ( )  B_SPLINE_SURFACE ( 3, 2, ( 
 ( #9365, #19917, #1522 ),
 ( #29617, #29433, #27245 ),
 ( #16887, #19574, #30128 ),
 ( #29770, #6849, #14047 ),
 ( #17036, #6527, #14540 ),
 ( #12050, #22246, #16542 ),
 ( #24254, #19730, #1370 ),
 ( #4539, #11547, #21743 ),
 ( #11698, #31951, #19235 ),
 ( #27923, #7702, #4691 ),
 ( #17714, #20405, #17396 ),
 ( #32799, #2178, #5188 ),
 ( #23069, #7352, #30785 ),
 ( #15972, #27740, #17543 ),
 ( #20086, #17897, #10984 ),
 ( #5036, #26194, #23689 ),
 ( #15215, #4847, #28091 ),
 ( #2679, #7203, #27590 ) ),
 .UNSPECIFIED., .F., .F., .F. ) 
 B_SPLINE_SURFACE_WITH_KNOTS ( ( 4, 2, 2, 2, 2, 2, 2, 2, 4 ),
 ( 3, 3 ),
 ( 0.000000000000000000, 0.3926990816987241395, 0.7853981633974482790, 1.178097245096172418, 1.570796326794896558, 1.963495408493620697, 2.356194490192344837, 2.748893571891068976, 3.141592653589793116 ),
 ( 0.000000000000000000, 1.000000000000000000 ),
 .UNSPECIFIED. ) 
 GEOMETRIC_REPRESENTATION_ITEM ( )  RATIONAL_B_SPLINE_SURFACE ( (
 ( 1.000000000000000000, 0.8526401643540935105, 1.000000000000000000),
 ( 1.000000000000000000, 0.8526458704374199060, 1.000000000000000000),
 ( 1.000000000000000000, 0.8500048284159407164, 1.000000000000000000),
 ( 1.000000000000000000, 0.8396427561410217955, 1.000000000000000000),
 ( 1.000000000000000000, 0.8319131657169130944, 1.000000000000000000),
 ( 1.000000000000000000, 0.8119378018741435499, 1.000000000000000000),
 ( 1.000000000000000000, 0.7996867613998320801, 1.000000000000000000),
 ( 1.000000000000000000, 0.7717639430037522841, 1.000000000000000000),
 ( 1.000000000000000000, 0.7560862040295790454, 1.000000000000000000),
 ( 1.000000000000000000, 0.7231030986475501798, 1.000000000000000000),
 ( 1.000000000000000000, 0.7057963334870693828, 1.000000000000000000),
 ( 1.000000000000000000, 0.6721825289763700972, 1.000000000000000000),
 ( 1.000000000000000000, 0.6558905360689835096, 1.000000000000000000),
 ( 1.000000000000000000, 0.6276164863454245513, 1.000000000000000000),
 ( 1.000000000000000000, 0.6156781713470711459, 1.000000000000000000),
 ( 1.000000000000000000, 0.5992555908992014402, 1.000000000000000000),
 ( 1.000000000000000000, 0.5947841457457127001, 1.000000000000000000),
 ( 1.000000000000000000, 0.5948227867513392608, 1.000000000000000000) ) ) 
 REPRESENTATION_ITEM ( '' )  SURFACE ( )  );
#30525 = LINE ( 'NONE', #17812, #137 ) ;
#30526 = CARTESIAN_POINT ( 'NONE',  ( -2.250050802731187183, -1.887961173149512062, -2.331437884370912261 ) ) ;
#30527 = ORIENTED_EDGE ( 'NONE', *, *, #8102, .T. ) ;
#30528 = CARTESIAN_POINT ( 'NONE',  ( -4.287550801365592967, -2.228590825266444586, -2.752080473201636401 ) ) ;
#30529 = AXIS2_PLACEMENT_3D ( 'NONE', #25817, #5094, #15104 ) ;
#30530 = DIRECTION ( 'NONE',  ( 1.000000000000000000, 0.000000000000000000, 0.000000000000000000 ) ) ;
#30531 = CARTESIAN_POINT ( 'NONE',  ( 20.53274989849676757, -21.72776571847661842, -1.408906953170802723 ) ) ;
#30532 = ORIENTED_EDGE ( 'NONE', *, *, #15698, .T. ) ;
#30533 = CARTESIAN_POINT ( 'NONE',  ( 5.377543748152548986, -5.151476664237435443, -6.139290821770307716 ) ) ;
#30534 = CARTESIAN_POINT ( 'NONE',  ( 5.377543748152548098, 7.530955069117513112, 2.741043480754951744 ) ) ;
#30535 = ORIENTED_EDGE ( 'NONE', *, *, #10569, .T. ) ;
#30536 = LINE ( 'NONE', #2611, #27333 ) ;
#30537 = CALENDAR_DATE ( 2026, 6, 10 ) ;
#30538 = VECTOR ( 'NONE', #14861, 1000.000000000000000 ) ;
#30540 = ORIENTED_EDGE ( 'NONE', *, *, #29897, .T. ) ;
#30539 = DIRECTION ( 'NONE',  ( 1.000000000000000000, 0.000000000000000000, 0.000000000000000000 ) ) ;
#30541 = ORIENTED_EDGE ( 'NONE', *, *, #647, .F. ) ;
#30542 = FACE_OUTER_BOUND ( 'NONE', #12347, .T. ) ;
#30543 = VECTOR ( 'NONE', #11970, 1000.000000000000000 ) ;
#30544 = AXIS2_PLACEMENT_3D ( 'NONE', #11576, #1238, #32160 ) ;
#30545 = ORIENTED_EDGE ( 'NONE', *, *, #12479, .T. ) ;
#30546 = CARTESIAN_POINT ( 'NONE',  ( -14.62340757463330654, -27.93932300454937590, -1.000000000000000000 ) ) ;
#30548 = ORIENTED_EDGE ( 'NONE', *, *, #32827, .T. ) ;
#30547 = DIRECTION ( 'NONE',  ( 0.000000000000000000, 0.9063077870366468280, 0.4226182617407062136 ) ) ;
#30549 = AXIS2_PLACEMENT_3D ( 'NONE', #9544, #17421, #12394 ) ;
#30550 = CARTESIAN_POINT ( 'NONE',  ( 41.45135008765517881, -9.497951668093163491, 0.07017451552781803215 ) ) ;
#30551 = DIRECTION ( 'NONE',  ( 1.000000000000000000, -0.000000000000000000, -0.000000000000000000 ) ) ;
#30552 = AXIS2_PLACEMENT_3D ( 'NONE', #864, #5845, #26736 ) ;
#30553 = EDGE_CURVE ( 'NONE', #22104, #17772, #6002, .T. ) ;
#30554 = LINE ( 'NONE', #17841, #5031 ) ;
#30555 = CARTESIAN_POINT ( 'NONE',  ( 101.7915493539012033, -3.896846208356848695, 4.171867813802681901 ) ) ;
#30556 = EDGE_CURVE ( 'NONE', #21890, #17869, #10274, .T. ) ;
#30557 = VECTOR ( 'NONE', #8725, 1000.000000000000000 ) ;
#30558 = AXIS2_PLACEMENT_3D ( 'NONE', #5740, #28969, #16259 ) ;
#30559 = VERTEX_POINT ( 'NONE', #3891 ) ;
#30560 = CARTESIAN_POINT ( 'NONE',  ( 21.49290772595112387, 0.1310194482076003919, 2.499999999999998668 ) ) ;
#30561 = LINE ( 'NONE', #10478, #25761 ) ;
#30562 = CARTESIAN_POINT ( 'NONE',  ( -50.60000000000000142, -21.43932300454937945, -1.500000000000000000 ) ) ;
#30563 = CARTESIAN_POINT ( 'NONE',  ( 3.122314033877864698E-16, 3.641590349731929965, 3.055657119358814011 ) ) ;
#30564 = CARTESIAN_POINT ( 'NONE',  ( 24.41148010920957034, -17.42203112336814996, 1.436991846559697361 ) ) ;
#30565 = AXIS2_PLACEMENT_3D ( 'NONE', #9289, #19506, #7395 ) ;
#30566 = DIRECTION ( 'NONE',  ( 7.472768010110837389E-18, 0.08715574274765461316, 0.9961946980917457672 ) ) ;
#30567 = CARTESIAN_POINT ( 'NONE',  ( -56.71489992210280207, 0.2545037525615557183, -1.043529352691957124 ) ) ;
#30568 = FACE_OUTER_BOUND ( 'NONE', #8145, .T. ) ;
#30569 = ORIENTED_EDGE ( 'NONE', *, *, #5077, .F. ) ;
#30570 = AXIS2_PLACEMENT_3D ( 'NONE', #27338, #6775, #22674 ) ;
#30571 = CIRCLE ( 'NONE', #27964, 8.750000000000000000 ) ;
#30572 = CARTESIAN_POINT ( 'NONE',  ( -7.712550801365593678, 1.088641768524161613, 3.675193018007247403 ) ) ;
#30573 = EDGE_LOOP ( 'NONE', ( #22044, #22806, #9985, #11998 ) ) ;
#30574 = CIRCLE ( 'NONE', #25758, 6.250000000000000000 ) ;
#30575 = AXIS2_PLACEMENT_3D ( 'NONE', #29040, #23351, #6131 ) ;
#30576 = CARTESIAN_POINT ( 'NONE',  ( -4.954531657079158435, 0.9198621039125853827, 3.105402419394639235 ) ) ;
#30577 = B_SPLINE_CURVE_WITH_KNOTS ( 'NONE', 3,
 ( #7699, #25055, #20230, #23241, #10176, #186, #30931 ),
 .UNSPECIFIED., .F., .F.,
 ( 4, 3, 4 ),
 ( 2.602085213965210256E-18, 0.002564119400760675634, 0.003456443488766134785 ),
 .UNSPECIFIED. ) ;
#30578 = CARTESIAN_POINT ( 'NONE',  ( 23.29750000136559862, -2.363507492473152283, -1.913930629741525280 ) ) ;
#30579 = DIRECTION ( 'NONE',  ( 0.000000000000000000, 0.000000000000000000, 1.000000000000000000 ) ) ;
#30580 = CARTESIAN_POINT ( 'NONE',  ( 0.4979849626702088639, -4.221418788689684121, 1.765595572481148512 ) ) ;
#30581 = CARTESIAN_POINT ( 'NONE',  ( 56.97280603064898941, -277.2763395528616002, 5.471072653610979941 ) ) ;
#30582 = VECTOR ( 'NONE', #24713, 1000.000000000000000 ) ;
#30583 = ORIENTED_EDGE ( 'NONE', *, *, #12657, .F. ) ;
#30584 = CARTESIAN_POINT ( 'NONE',  ( 10.52034268205830614, 3.993798362933350887, -3.024842911000649615 ) ) ;
#30585 = CARTESIAN_POINT ( 'NONE',  ( 3.249999999999999556, -0.4999240074893822605, -8.734705317681632053 ) ) ;
#30586 = ORIENTED_EDGE ( 'NONE', *, *, #22518, .T. ) ;
#30587 = CARTESIAN_POINT ( 'NONE',  ( 7.249760686538667009, 2.210816291636212405, 8.466096581343489191 ) ) ;
#30588 = CALENDAR_DATE ( 2026, 6, 10 ) ;
#30589 = CARTESIAN_POINT ( 'NONE',  ( 40.88388279378574452, -6.876528161884418289, 4.023789691746774366 ) ) ;
#30590 = ADVANCED_FACE ( 'NONE', ( #1386 ), #17190, .T. ) ;
#30591 = DIRECTION ( 'NONE',  ( 0.9842544651762055175, -0.1767573132311700268, 0.000000000000000000 ) ) ;
#30592 = VECTOR ( 'NONE', #2546, 1000.000000000000000 ) ;
#30594 = CARTESIAN_POINT ( 'NONE',  ( 5.489321606599604664, 7.664118171219035602, -2.678948506461252599 ) ) ;
#30593 = CARTESIAN_POINT ( 'NONE',  ( 0.3045634635876931506, -10.03290811084029954, -2.226307684702790723 ) ) ;
#30595 = VECTOR ( 'NONE', #20409, 1000.000000000000000 ) ;
#30596 = ORIENTED_EDGE ( 'NONE', *, *, #25623, .F. ) ;
#30597 = VECTOR ( 'NONE', #32069, 1000.000000000000114 ) ;
#30598 = CYLINDRICAL_SURFACE ( 'NONE', #29552, 0.4500000000000025646 ) ;
#30599 = DIRECTION ( 'NONE',  ( -1.000000000000000000, 0.000000000000000000, 0.000000000000000000 ) ) ;
#30600 = AXIS2_PLACEMENT_3D ( 'NONE', #11209, #9366, #4188 ) ;
#30601 = CARTESIAN_POINT ( 'NONE',  ( 25.36000000136559862, -1.570731468192933633, -2.892927487894330074 ) ) ;
#30602 = VECTOR ( 'NONE', #20123, 999.9999999999998863 ) ;
#30603 = CARTESIAN_POINT ( 'NONE',  ( 12.13203477089214388, -15.56659747185076448, -1.754034475440599872 ) ) ;
#30605 = ORIENTED_EDGE ( 'NONE', *, *, #5248, .T. ) ;
#30604 = CARTESIAN_POINT ( 'NONE',  ( 71.67787245194618606, -18.34520463695562498, 1.500000000000000444 ) ) ;
#30606 = CARTESIAN_POINT ( 'NONE',  ( -6.462550801365593678, 0.3701630799359330593, -3.521866450007987037 ) ) ;
#30607 = DIRECTION ( 'NONE',  ( 0.000000000000000000, 0.000000000000000000, 1.000000000000000000 ) ) ;
#30608 = CARTESIAN_POINT ( 'NONE',  ( -23.54713438637982748, 3.520075575296777171, 1.500000000000000000 ) ) ;
#30609 = LINE ( 'NONE', #10360, #10208 ) ;
#30610 =( GEOMETRIC_REPRESENTATION_CONTEXT ( 3 ) GLOBAL_UNCERTAINTY_ASSIGNED_CONTEXT ( ( #30239 ) ) GLOBAL_UNIT_ASSIGNED_CONTEXT ( ( #7794, #17986, #23812 ) ) REPRESENTATION_CONTEXT ( 'NONE', 'WORKASPACE' ) );
#30611 = ORIENTED_EDGE ( 'NONE', *, *, #5908, .F. ) ;
#30613 = EDGE_LOOP ( 'NONE', ( #25170, #5080, #13441 ) ) ;
#30612 = CARTESIAN_POINT ( 'NONE',  ( 24.40342144122392298, -17.37878489514629265, 1.350270808450722670 ) ) ;
#30614 = AXIS2_PLACEMENT_3D ( 'NONE', #17250, #9885, #26952 ) ;
#30615 = CARTESIAN_POINT ( 'NONE',  ( 21.62838417909332733, -16.89547707397426279, -1.499999999999863665 ) ) ;
#30616 = CARTESIAN_POINT ( 'NONE',  ( 2.274274201625327230, -10.82112760146734765, -1.975651141462354543 ) ) ;
#30617 = EDGE_CURVE ( 'NONE', #17653, #12775, #4388, .T. ) ;
#30618 = CARTESIAN_POINT ( 'NONE',  ( 21.36000000136559507, -1.570731468192933633, -2.892927487894330962 ) ) ;
#30619 = CARTESIAN_POINT ( 'NONE',  ( 84.96516786084541195, -4.058994088352219087, 3.993433528812682098 ) ) ;
#30620 = CARTESIAN_POINT ( 'NONE',  ( 7.541748857011418394, -18.86390992599486438, -1.499999999999761746 ) ) ;
#30621 = CIRCLE ( 'NONE', #12983, 8.749000000000002331 ) ;
#30622 = CARTESIAN_POINT ( 'NONE',  ( 3.063284526839887167, 4.729683950898978750, -7.360373001730866171 ) ) ;
#30623 = PRODUCT_DEFINITION_SHAPE ( 'NONE', 'NONE',  #33103 ) ;
#30624 = AXIS2_PLACEMENT_3D ( 'NONE', #15863, #11173, #8197 ) ;
#30625 = EDGE_CURVE ( 'NONE', #3908, #16153, #7045, .T. ) ;
#30626 = AXIS2_PLACEMENT_3D ( 'NONE', #28320, #8098, #10604 ) ;
#30627 = LINE ( 'NONE', #20738, #11362 ) ;
#30628 = CARTESIAN_POINT ( 'NONE',  ( 107.8771114573266630, -16.29979767294548409, 1.280413873165804128 ) ) ;
#30629 = VERTEX_POINT ( 'NONE', #1039 ) ;
#30630 = DIRECTION ( 'NONE',  ( -0.1436597682917712671, 0.03489949670250103858, 0.9890115753135888532 ) ) ;
#30631 = VECTOR ( 'NONE', #8840, 1000.000000000000227 ) ;
#30632 = AXIS2_PLACEMENT_3D ( 'NONE', #6529, #8716, #16544 ) ;
#30633 = EDGE_CURVE ( 'NONE', #3483, #31221, #31645, .T. ) ;
#30634 = PERSON_AND_ORGANIZATION_ROLE ( 'design_supplier' ) ;
#30636 = CARTESIAN_POINT ( 'NONE',  ( 25.75999999999999801, -2.208672634433321348E-15, 0.000000000000000000 ) ) ;
#30635 = APPROVAL_PERSON_ORGANIZATION ( #23221, #9842, #10500 ) ;
#30637 = ORIENTED_EDGE ( 'NONE', *, *, #1411, .T. ) ;
#30638 = CARTESIAN_POINT ( 'NONE',  ( -23.54713438637982748, 8.763231220430828472, 1.786631099142472534 ) ) ;
#30639 = ORIENTED_EDGE ( 'NONE', *, *, #31970, .F. ) ;
#30640 = CARTESIAN_POINT ( 'NONE',  ( -18.90002009650197934, 6.067137108840462645, 2.089261350533889061 ) ) ;
#30642 = ORIENTED_EDGE ( 'NONE', *, *, #8833, .F. ) ;
#30641 = CARTESIAN_POINT ( 'NONE',  ( 40.87777647240479695, -5.756792757569010988, -4.006106576936585562 ) ) ;
#30643 = ORIENTED_EDGE ( 'NONE', *, *, #5299, .T. ) ;
#30644 = ADVANCED_FACE ( 'NONE', ( #11716 ), #19937, .F. ) ;
#30645 = EDGE_CURVE ( 'NONE', #7325, #20999, #23249, .T. ) ;
#30646 = FACE_OUTER_BOUND ( 'NONE', #4815, .T. ) ;
#30647 = PLANE ( 'NONE',  #31048 ) ;
#30648 = CARTESIAN_POINT ( 'NONE',  ( 6.883866557622099869, -8.415306967752693268, 2.328663417917411049 ) ) ;
#30649 = PLANE ( 'NONE',  #26268 ) ;
#30651 = EDGE_LOOP ( 'NONE', ( #17325, #11481, #24293, #9028 ) ) ;
#30650 = CARTESIAN_POINT ( 'NONE',  ( 1.624999999999999778, 1.975651141462390070, -10.82112760146734232 ) ) ;
#30652 = VECTOR ( 'NONE', #12081, 1000.000000000000000 ) ;
#30653 = CARTESIAN_POINT ( 'NONE',  ( 107.5756344652065621, -19.18288839493439468, 4.113624156228013362 ) ) ;
#30654 = CARTESIAN_POINT ( 'NONE',  ( -1.033057378353323452, -8.048844657540879410, 4.522129901861156931 ) ) ;
#30655 = VECTOR ( 'NONE', #15587, 999.9999999999998863 ) ;
#30656 = CARTESIAN_POINT ( 'NONE',  ( -2.938323964970641633, -11.64395169159722521, 1.499999999999919620 ) ) ;
#30657 = CARTESIAN_POINT ( 'NONE',  ( 23.23500000136559862, -1.570731468192933633, -2.892927487894330074 ) ) ;
#30658 = VECTOR ( 'NONE', #4081, 1000.000000000000114 ) ;
#30659 = DIRECTION ( 'NONE',  ( 0.000000000000000000, 0.5735764363510510444, -0.8191520442889883569 ) ) ;
#30660 = EDGE_CURVE ( 'NONE', #6030, #11692, #24926, .T. ) ;
#30662 = ORIENTED_EDGE ( 'NONE', *, *, #25289, .F. ) ;
#30661 = CARTESIAN_POINT ( 'NONE',  ( 18.62687130938129343, -7.348052634901513613, -1.527295581757700749 ) ) ;
#30663 = CARTESIAN_POINT ( 'NONE',  ( -8.049676575031998738, 0.000000000000000000, -6.923700951379997193 ) ) ;
#30664 = CIRCLE ( 'NONE', #3957, 0.4499999999999990119 ) ;
#30665 = VECTOR ( 'NONE', #26558, 1000.000000000000000 ) ;
#30666 = CARTESIAN_POINT ( 'NONE',  ( -24.00476095649313635, 18.44930403746426961, 1.773314187735097747 ) ) ;
#30667 = CARTESIAN_POINT ( 'NONE',  ( 23.73500000273118715, -2.486304738420683780, 0.2613211581691335383 ) ) ;
#30668 = CC_DESIGN_APPROVAL ( #11877, ( #32113 ) ) ;
#30669 = EDGE_CURVE ( 'NONE', #29851, #14011, #20100, .T. ) ;
#30670 = CARTESIAN_POINT ( 'NONE',  ( 34.48223484310466347, 0.000000000000000000, 13.00000000000012079 ) ) ;
#30671 = CARTESIAN_POINT ( 'NONE',  ( 56.97280603064898941, -277.2763395528616002, -0.4463807625373593657 ) ) ;
#30672 = VERTEX_POINT ( 'NONE', #1706 ) ;
#30673 = DIRECTION ( 'NONE',  ( 8.281886410780543074E-17, 0.9659258262890716429, -0.2588190451025081940 ) ) ;
#30674 = PLANE ( 'NONE',  #24657 ) ;
#30675 = CARTESIAN_POINT ( 'NONE',  ( -5.537550801365593856, 3.368539882008727115, 1.828967928396027176 ) ) ;
#30676 = VERTEX_POINT ( 'NONE', #22602 ) ;
#30677 = CIRCLE ( 'NONE', #22635, 5.000000000000000888 ) ;
#30678 = VECTOR ( 'NONE', #5465, 1000.000000000000000 ) ;
#30679 = CARTESIAN_POINT ( 'NONE',  ( 25.28110583668922473, 2.565906573285401393, 0.05495561580884226333 ) ) ;
#30680 = LINE ( 'NONE', #9915, #3438 ) ;
#30681 = CARTESIAN_POINT ( 'NONE',  ( 41.92799935455844462, -21.01937708447562159, -4.522129901861164925 ) ) ;
#30682 = FACE_OUTER_BOUND ( 'NONE', #14359, .T. ) ;
#30683 = ADVANCED_FACE ( 'NONE', ( #14728 ), #4709, .T. ) ;
#30684 = ORIENTED_EDGE ( 'NONE', *, *, #995, .F. ) ;
#30685 = CARTESIAN_POINT ( 'NONE',  ( 0.1574692293613783600, -4.391622967207749362, -9.672096048330562468 ) ) ;
#30686 = ORIENTED_EDGE ( 'NONE', *, *, #12845, .F. ) ;
#30687 = CARTESIAN_POINT ( 'NONE',  ( 107.4934547166204624, -17.99061096458791198, 5.137745733581649432 ) ) ;
#30689 = VERTEX_POINT ( 'NONE', #7220 ) ;
#30688 = CARTESIAN_POINT ( 'NONE',  ( 17.32050807568873552, 10.00000000000002309, 1.500000000000000000 ) ) ;
#30690 = EDGE_LOOP ( 'NONE', ( #11679, #16005, #22644, #13758, #29859 ) ) ;
#30691 = CARTESIAN_POINT ( 'NONE',  ( 5.377543748152548986, -4.007137495034764463, -6.940565734314639634 ) ) ;
#30692 = ADVANCED_FACE ( 'NONE', ( #24578 ), #27262, .T. ) ;
#30693 = LOCAL_TIME ( 16, 7, 10.00000000000000000, #17635 ) ;
#30694 = EDGE_CURVE ( 'NONE', #32393, #25811, #17224, .T. ) ;
#30695 = ORIENTED_EDGE ( 'NONE', *, *, #3420, .F. ) ;
#30696 = DIRECTION ( 'NONE',  ( -0.1027947991993879290, 0.9947025833170223263, 0.000000000000000000 ) ) ;
#30698 = ORIENTED_EDGE ( 'NONE', *, *, #13931, .F. ) ;
#30697 = CARTESIAN_POINT ( 'NONE',  ( 7.249760686538667009, 7.953573330858214163, 3.647351267791597795 ) ) ;
#30699 = CARTESIAN_POINT ( 'NONE',  ( -5.712942406915326288, 3.284080845023683730E-15, 3.000000000000000000 ) ) ;
#30700 = CARTESIAN_POINT ( 'NONE',  ( 21.23499999999999943, 0.2613211581691317065, 2.486304738420681559 ) ) ;
#30701 = CARTESIAN_POINT ( 'NONE',  ( -34.48223484310472031, 0.5000000000000000000, 2.552009564962238297 ) ) ;
#30702 = DIRECTION ( 'NONE',  ( -4.458171167563057872E-29, 1.000000000000000000, 5.782411586589359611E-15 ) ) ;
#30703 = CIRCLE ( 'NONE', #18933, 2.524999999999999911 ) ;
#30704 = CARTESIAN_POINT ( 'NONE',  ( 6.038144483126824724, 8.463061282283012687, 0.4487862922133540877 ) ) ;
#30705 = DIRECTION ( 'NONE',  ( 0.1027947991993878873, -0.9947025833170223263, 4.441163149043747538E-14 ) ) ;
#30706 = CARTESIAN_POINT ( 'NONE',  ( 7.577572045913243848, 15.00000000000000178, -4.612695725900422872 ) ) ;
#30707 = EDGE_CURVE ( 'NONE', #30379, #689, #6547, .T. ) ;
#30708 = CARTESIAN_POINT ( 'NONE',  ( 4.749760686538667009, -4.007137495034764463, -6.940565734314639634 ) ) ;
#30709 = CARTESIAN_POINT ( 'NONE',  ( 3.499999999999999556, 5.471841788314708133, 3.018103451449746899 ) ) ;
#30710 = CC_DESIGN_PERSON_AND_ORGANIZATION_ASSIGNMENT ( #154, #12517, ( #28213 ) ) ;
#30711 = DIRECTION ( 'NONE',  ( -1.000000000000000000, -0.000000000000000000, 0.000000000000000000 ) ) ;
#30712 = CARTESIAN_POINT ( 'NONE',  ( 47.68482864957696421, -3.825617316378856714, -0.02339150518254430253 ) ) ;
#30713 = CARTESIAN_POINT ( 'NONE',  ( 18.74780019990317115, -5.996310340153147678, 5.695980980372492120 ) ) ;
#30714 = CARTESIAN_POINT ( 'NONE',  ( -3.400050802731187982, 0.9222479816126443186, 3.113457007523260156 ) ) ;
#30715 = ORIENTED_EDGE ( 'NONE', *, *, #14280, .F. ) ;
#30716 = CARTESIAN_POINT ( 'NONE',  ( -6.687550801365594211, -2.228590825266444586, -2.752080473201636401 ) ) ;
#30717 = CARTESIAN_POINT ( 'NONE',  ( 3.958196854299272687E-16, 4.616489984850558947, -1.946309384392544972 ) ) ;
#30718 = LINE ( 'NONE', #20988, #10343 ) ;
#30719 = VERTEX_POINT ( 'NONE', #29948 ) ;
#30720 = CARTESIAN_POINT ( 'NONE',  ( 85.08949032934708612, -1.315411135598755221, -0.07017451552781628354 ) ) ;
#30721 = CARTESIAN_POINT ( 'NONE',  ( 2.274274201625327230, 7.958834565716768061, 7.593217523260608282 ) ) ;
#30722 = ADVANCED_FACE ( 'NONE', ( #16751 ), #24772, .T. ) ;
#30723 = VECTOR ( 'NONE', #15932, 1000.000000000000000 ) ;
#30724 = VERTEX_POINT ( 'NONE', #2194 ) ;
#30725 = DIRECTION ( 'NONE',  ( -1.000000000000000000, 0.000000000000000000, 0.000000000000000000 ) ) ;
#30726 = PERSON_AND_ORGANIZATION_ROLE ( 'design_supplier' ) ;
#30728 = ORIENTED_EDGE ( 'NONE', *, *, #9242, .F. ) ;
#30727 = CARTESIAN_POINT ( 'NONE',  ( 6.655951778521610684, -18.71196003547629516, -1.499999999999999556 ) ) ;
#30729 = VERTEX_POINT ( 'NONE', #12382 ) ;
#30730 = CARTESIAN_POINT ( 'NONE',  ( 7.720912629997967791, -18.80905748744269701, 1.749363945344754478 ) ) ;
#30731 = EDGE_LOOP ( 'NONE', ( #27560, #7085, #2249, #4336, #3075 ) ) ;
#30732 = CARTESIAN_POINT ( 'NONE',  ( 7.064632816082964339, 0.7071067811866330599, -8.721381771256195847 ) ) ;
#30734 = ORIENTED_EDGE ( 'NONE', *, *, #25903, .F. ) ;
#30733 = DIRECTION ( 'NONE',  ( -1.000000000000000000, -0.000000000000000000, -0.000000000000000000 ) ) ;
#30735 = DIRECTION ( 'NONE',  ( 0.1908089953765452762, -0.000000000000000000, -0.9816271834476639757 ) ) ;
#30737 = CARTESIAN_POINT ( 'NONE',  ( 108.0350161675694238, -18.57358621869218140, 4.153351887601565373 ) ) ;
#30736 = ADVANCED_BREP_SHAPE_REPRESENTATION ( '', ( #32130, #2865 ), #21519 ) ;
#30738 = CARTESIAN_POINT ( 'NONE',  ( 3.499999999999999556, 0.000000000000000000, 0.000000000000000000 ) ) ;
#30739 = DIRECTION ( 'NONE',  ( -1.000000000000000000, 0.000000000000000000, 0.000000000000000000 ) ) ;
#30740 = EDGE_LOOP ( 'NONE', ( #8766, #14326, #18536, #6445 ) ) ;
#30741 = CARTESIAN_POINT ( 'NONE',  ( 0.000000000000000000, 0.000000000000000000, 1.500000000000000000 ) ) ;
#30742 = DIRECTION ( 'NONE',  ( 0.4809547266710044178, 0.000000000000000000, 0.8767454310646958238 ) ) ;
#30743 = CARTESIAN_POINT ( 'NONE',  ( 29.18862856207060119, -8.152784366137925787, -1.169950487275103868 ) ) ;
#30744 = CARTESIAN_POINT ( 'NONE',  ( -0.2059365608663963898, 0.000000000000000000, -4.131740999229418954 ) ) ;
#30745 = ADVANCED_FACE ( 'NONE', ( #19747 ), #32814, .F. ) ;
#30746 = CARTESIAN_POINT ( 'NONE',  ( 24.75456913062235031, -17.48748849332650579, 1.499999999999906075 ) ) ;
#30747 = CARTESIAN_POINT ( 'NONE',  ( 10.00000000000000000, 4.681538312723528605, -0.8254815157534771686 ) ) ;
#30748 = CARTESIAN_POINT ( 'NONE',  ( -56.74498568481996585, 0.3183045829754697076, -1.046596361453495216 ) ) ;
#30749 = CARTESIAN_POINT ( 'NONE',  ( 0.000000000000000000, 1.999317321091499400, 10.76487093102065451 ) ) ;
#30750 = ORIENTED_EDGE ( 'NONE', *, *, #22054, .F. ) ;
#30751 = CARTESIAN_POINT ( 'NONE',  ( -6.762550801365593500, -2.752080473201636845, 2.228590825266444586 ) ) ;
#30752 = ORIENTED_EDGE ( 'NONE', *, *, #10140, .F. ) ;
#30753 = CARTESIAN_POINT ( 'NONE',  ( -5.004531657079158258, 1.883076972206379374, 2.325406398514293205 ) ) ;
#30754 = CARTESIAN_POINT ( 'NONE',  ( 107.6037974194920679, 18.80702961649189575, 5.126032704575725241 ) ) ;
#30755 = FACE_OUTER_BOUND ( 'NONE', #25586, .T. ) ;
#30756 = CARTESIAN_POINT ( 'NONE',  ( 9.360049167875386544, -11.53021799246641343, 1.000000000000000000 ) ) ;
#30757 = ORIENTED_EDGE ( 'NONE', *, *, #851, .F. ) ;
#30758 = ADVANCED_FACE ( 'NONE', ( #19442 ), #2039, .T. ) ;
#30759 = CARTESIAN_POINT ( 'NONE',  ( 34.98223484310472031, 0.5000000000000000000, -2.552009564962228527 ) ) ;
#30760 = EDGE_CURVE ( 'NONE', #17637, #3652, #19270, .T. ) ;
#30761 = EDGE_LOOP ( 'NONE', ( #15651, #12558, #11520, #22990 ) ) ;
#30762 = CARTESIAN_POINT ( 'NONE',  ( 0.5032040285356975673, 9.002252291012739605, 3.698073368192989818 ) ) ;
#30763 = EDGE_CURVE ( 'NONE', #5413, #10538, #17080, .T. ) ;
#30764 = PERSON_AND_ORGANIZATION_ROLE ( 'creator' ) ;
#30765 = CARTESIAN_POINT ( 'NONE',  ( 18.76136331414632252, -5.844701943473404882, 4.043900693813307079 ) ) ;
#30766 = CARTESIAN_POINT ( 'NONE',  ( 25.52557118915447987, -17.56218954043521663, -1.000000000000000444 ) ) ;
#30768 = DIRECTION ( 'NONE',  ( -0.000000000000000000, -0.000000000000000000, -1.000000000000000000 ) ) ;
#30767 = CARTESIAN_POINT ( 'NONE',  ( 0.08034252392847902879, -10.58792409793185030, -2.072171912280182493 ) ) ;
#30769 = EDGE_LOOP ( 'NONE', ( #26578, #18439, #21420, #25119 ) ) ;
#30770 = CARTESIAN_POINT ( 'NONE',  ( -7.700050802731188249, 1.549418761218566143, -2.853674364686379583 ) ) ;
#30771 = CYLINDRICAL_SURFACE ( 'NONE', #1127, 4.000000000000001776 ) ;
#30772 = DIRECTION ( 'NONE',  ( 0.000000000000000000, 0.000000000000000000, 1.000000000000000000 ) ) ;
#30773 = CARTESIAN_POINT ( 'NONE',  ( 1.750000000000000222, 4.058600654062949786, -7.468451026206159860 ) ) ;
#30775 = EDGE_LOOP ( 'NONE', ( #11445, #10349, #12030, #21309 ) ) ;
#30774 = CARTESIAN_POINT ( 'NONE',  ( 107.4505081161385363, 17.92734912429073191, 4.774562840296773025 ) ) ;
#30776 = CARTESIAN_POINT ( 'NONE',  ( -5.162550801365593856, -2.752080473201636845, 2.228590825266444586 ) ) ;
#30777 = DIRECTION ( 'NONE',  ( 2.637475533091417728E-15, 0.000000000000000000, 1.000000000000000000 ) ) ;
#30778 = DIRECTION ( 'NONE',  ( -1.000000000000000000, 8.574039729943017111E-17, -3.081487911019577365E-33 ) ) ;
#30779 = CARTESIAN_POINT ( 'NONE',  ( -29.24402871571405882, -25.93932300454937945, 11.00000000000000000 ) ) ;
#30780 = ORIENTED_EDGE ( 'NONE', *, *, #3466, .F. ) ;
#30781 = ORIENTED_EDGE ( 'NONE', *, *, #6221, .T. ) ;
#30782 = CARTESIAN_POINT ( 'NONE',  ( 10.90258948330155953, 17.51112508050605854, -4.612695725900421984 ) ) ;
#30783 = CARTESIAN_POINT ( 'NONE',  ( 0.6708088701982989344, 0.000000000000000000, -4.612695725900422872 ) ) ;
#30784 = CARTESIAN_POINT ( 'NONE',  ( 23.17250000136559862, -3.024605502323851169, 0.3178988483021052969 ) ) ;
#30785 = CARTESIAN_POINT ( 'NONE',  ( -29.24806983202650557, 6.485688093852433944, 1.500000000000000000 ) ) ;
#30786 = LINE ( 'NONE', #26711, #23115 ) ;
#30787 = EDGE_CURVE ( 'NONE', #18631, #11534, #16684, .T. ) ;
#30788 = CARTESIAN_POINT ( 'NONE',  ( 2.274274201625315239, -10.82112760146740449, 1.975651141462185789 ) ) ;
#30789 = B_SPLINE_CURVE_WITH_KNOTS ( 'NONE', 3,
 ( #10377, #20239, #20585, #352, #22903, #25423, #2377, #30793 ),
 .UNSPECIFIED., .F., .F.,
 ( 4, 2, 2, 4 ),
 ( 2.197717257069985215E-07, 0.001262070444977237251, 0.001892995781603003420, 0.002523921118228769373 ),
 .UNSPECIFIED. ) ;
#30790 = DIRECTION ( 'NONE',  ( 0.000000000000000000, 0.000000000000000000, 1.000000000000000000 ) ) ;
#30791 = CARTESIAN_POINT ( 'NONE',  ( -32.99878091140236336, 0.000000000000000000, 3.000000000000004441 ) ) ;
#30792 = EDGE_LOOP ( 'NONE', ( #29564, #2041, #19593 ) ) ;
#30793 = CARTESIAN_POINT ( 'NONE',  ( 3.063284526839887167, 6.772677083992467928, -5.538577986808824960 ) ) ;
#30794 = EDGE_CURVE ( 'NONE', #17553, #30211, #11349, .T. ) ;
#30795 = EDGE_CURVE ( 'NONE', #32393, #14212, #9663, .T. ) ;
#30796 =( NAMED_UNIT ( * ) SI_UNIT ( $, .STERADIAN. ) SOLID_ANGLE_UNIT ( ) );
#30797 = CARTESIAN_POINT ( 'NONE',  ( 19.03654924710325602, -2.768675503676416572, 2.713652344655542503 ) ) ;
#30798 = VERTEX_POINT ( 'NONE', #12707 ) ;
#30799 = SHAPE_REPRESENTATION ( 'Part7_handle1Sleeve', ( #2865 ), #21519 ) ;
#30800 = CARTESIAN_POINT ( 'NONE',  ( 107.5519901325125716, 18.50907416150531049, -5.131959998105128484 ) ) ;
#30801 = EDGE_LOOP ( 'NONE', ( #32718, #19537, #4418, #30698 ) ) ;
#30802 = CARTESIAN_POINT ( 'NONE',  ( -21.11158745431430361, 4.499601903092431243, 2.132273290772896512 ) ) ;
#30804 = ORIENTED_EDGE ( 'NONE', *, *, #24510, .T. ) ;
#30803 = CARTESIAN_POINT ( 'NONE',  ( 18.84882253404822094, -4.867083393560534432, -4.150065909464428771 ) ) ;
#30805 = VERTEX_POINT ( 'NONE', #11368 ) ;
#30806 = CARTESIAN_POINT ( 'NONE',  ( -3.889464452585704723, -3.181828567483031112, -1.500000000000000000 ) ) ;
#30807 = CARTESIAN_POINT ( 'NONE',  ( -6.262550801365593500, 3.521866450007987037, 0.3701630799359328372 ) ) ;
#30808 = PLANE ( 'NONE',  #17753 ) ;
#30809 = DIRECTION ( 'NONE',  ( -1.000000000000000000, -0.000000000000000000, 0.000000000000000000 ) ) ;
#30811 = ORIENTED_EDGE ( 'NONE', *, *, #23669, .T. ) ;
#30810 = CARTESIAN_POINT ( 'NONE',  ( 22.17250000273118715, 2.378061970571979433, -1.291182301015470602 ) ) ;
#30812 = CARTESIAN_POINT ( 'NONE',  ( -23.54713438637982748, 13.62472719076215988, 10.27593816114768011 ) ) ;
#30813 = CARTESIAN_POINT ( 'NONE',  ( 25.25107927547938758, 18.67207037180926221, 1.049999999999822853 ) ) ;
#30814 = CARTESIAN_POINT ( 'NONE',  ( -3.674210872405168082, -10.80251965388255364, 1.499999999999999112 ) ) ;
#30815 = CARTESIAN_POINT ( 'NONE',  ( 25.29750000136559507, -0.3178988483021076838, -3.024605502323848949 ) ) ;
#30816 = DIRECTION ( 'NONE',  ( -1.000000000000000000, -0.000000000000000000, -0.000000000000000000 ) ) ;
#30818 = ORIENTED_EDGE ( 'NONE', *, *, #18380, .T. ) ;
#30817 = CARTESIAN_POINT ( 'NONE',  ( 21.08401840680096129, -16.78474387324269657, -1.500000000000000000 ) ) ;
#30819 = DIRECTION ( 'NONE',  ( 0.9999770835954139292, -0.006769954505784861812, 0.000000000000000000 ) ) ;
#30820 = ADVANCED_FACE ( 'NONE', ( #23745 ), #7078, .T. ) ;
#30821 = CARTESIAN_POINT ( 'NONE',  ( 2.785385763235068701, 9.518934100285017408, 2.300561732649628155 ) ) ;
#30822 = CARTESIAN_POINT ( 'NONE',  ( 21.04750000136559507, -3.024605502323851169, 0.3178988483021052969 ) ) ;
#30823 = CARTESIAN_POINT ( 'NONE',  ( 22.00111451137534502, -1.241879311143409511E-16, -2.499999999999998668 ) ) ;
#30824 = CARTESIAN_POINT ( 'NONE',  ( 7.064423539573518873, 8.721381771257245674, -0.7071067811875828557 ) ) ;
#30825 = CARTESIAN_POINT ( 'NONE',  ( -33.81874022276151237, 20.00000000000000000, 2.395703997917905337 ) ) ;
#30826 = EDGE_CURVE ( 'NONE', #18318, #29863, #21639, .T. ) ;
#30827 = ORIENTED_EDGE ( 'NONE', *, *, #29276, .T. ) ;
#30828 = DIRECTION ( 'NONE',  ( 0.000000000000000000, -0.1045284632676534292, 0.9945218953682734009 ) ) ;
#30829 = EDGE_CURVE ( 'NONE', #29275, #5198, #13352, .T. ) ;
#30830 = DIRECTION ( 'NONE',  ( -0.000000000000000000, -0.000000000000000000, -1.000000000000000000 ) ) ;
#30831 = ADVANCED_FACE ( 'NONE', ( #16368 ), #1002, .T. ) ;
#30832 = CARTESIAN_POINT ( 'NONE',  ( 107.5306748766070939, -18.53203061720905254, -5.070947615523107466 ) ) ;
#30833 = ORIENTED_EDGE ( 'NONE', *, *, #12017, .T. ) ;
#30834 = DIRECTION ( 'NONE',  ( 0.000000000000000000, 0.000000000000000000, 1.000000000000000000 ) ) ;
#30835 = CARTESIAN_POINT ( 'NONE',  ( 7.064423637758999952, -8.437262856155475887, -2.318425219013692473 ) ) ;
#30836 = EDGE_CURVE ( 'NONE', #15946, #5049, #25771, .T. ) ;
#30837 = CARTESIAN_POINT ( 'NONE',  ( 0.8174570305809125692, -9.170357625429589987, -1.500000000000000444 ) ) ;
#30838 = DIRECTION ( 'NONE',  ( 0.9993908270190957621, 0.03489949670250118430, 0.000000000000000000 ) ) ;
#30839 = ORIENTED_EDGE ( 'NONE', *, *, #17254, .T. ) ;
#30840 = ORIENTED_EDGE ( 'NONE', *, *, #32900, .F. ) ;
#30841 = CARTESIAN_POINT ( 'NONE',  ( 2.864530875629067275, 0.6595692664038855790, -9.539603485476124689 ) ) ;
#30843 = EDGE_LOOP ( 'NONE', ( #11983, #27266, #7289, #26568 ) ) ;
#30842 = CARTESIAN_POINT ( 'NONE',  ( -50.81000000000000227, -10.96999999999998643, 1.949999999999999956 ) ) ;
#30844 = ORIENTED_EDGE ( 'NONE', *, *, #18537, .F. ) ;
#30845 = CARTESIAN_POINT ( 'NONE',  ( -57.40374817251313999, -2.616512360834426953, 5.500000000000000000 ) ) ;
#30846 = EDGE_CURVE ( 'NONE', #1971, #30410, #2836, .T. ) ;
#30847 = VERTEX_POINT ( 'NONE', #31598 ) ;
#30848 = CARTESIAN_POINT ( 'NONE',  ( 2.619288827430985567, 0.4094970184090461762, -1.491740999229418829 ) ) ;
#30850 = ORIENTED_EDGE ( 'NONE', *, *, #25118, .T. ) ;
#30849 = CARTESIAN_POINT ( 'NONE',  ( 1.305960519821096844, -9.941484022874826465, 1.500000000000000000 ) ) ;
#30851 = ORIENTED_EDGE ( 'NONE', *, *, #19550, .T. ) ;
#30852 = CARTESIAN_POINT ( 'NONE',  ( 56.97280603064904625, -277.2763395528616002, 566.7009208965938569 ) ) ;
#30853 = DIRECTION ( 'NONE',  ( -1.000000000000000000, -0.000000000000000000, -0.000000000000000000 ) ) ;
#30854 = CARTESIAN_POINT ( 'NONE',  ( 4.285194126261599773E-30, 4.979297819079224069E-14, -4.753758587302147731 ) ) ;
#30855 = CARTESIAN_POINT ( 'NONE',  ( 0.000000000000000000, 0.000000000000000000, 0.000000000000000000 ) ) ;
#30856 = CARTESIAN_POINT ( 'NONE',  ( 10.00000000000000000, -3.055657119358826446, 3.641590349731918863 ) ) ;
#30857 = DIRECTION ( 'NONE',  ( 0.000000000000000000, 0.000000000000000000, 1.000000000000000000 ) ) ;
#30858 = FACE_OUTER_BOUND ( 'NONE', #316, .T. ) ;
#30859 = LINE ( 'NONE', #7779, #30723 ) ;
#30860 = CARTESIAN_POINT ( 'NONE',  ( 10.55147673363118876, -2.718385644597205442, 4.208382051008182856 ) ) ;
#30861 = CARTESIAN_POINT ( 'NONE',  ( 54.77277180716814087, -8.244003004416214253, -0.02339150517595086839 ) ) ;
#30862 = CARTESIAN_POINT ( 'NONE',  ( 6.880159540721329847, -3.624895993596817245, -7.943102264535292001 ) ) ;
#30863 = ADVANCED_FACE ( 'NONE', ( #15875 ), #31432, .T. ) ;
#30864 = CARTESIAN_POINT ( 'NONE',  ( 6.037141812302426302, -8.411869123983608532, -1.028012177296172780 ) ) ;
#30865 = ADVANCED_FACE ( 'NONE', ( #1351 ), #26434, .F. ) ;
#30866 = PLANE ( 'NONE',  #17235 ) ;
#30867 = ORIENTED_EDGE ( 'NONE', *, *, #20793, .T. ) ;
#30868 = CARTESIAN_POINT ( 'NONE',  ( -5.387550801365593500, -0.3701630799359326152, 3.521866450007987037 ) ) ;
#30869 = CARTESIAN_POINT ( 'NONE',  ( 9.187365643239736812, 0.07845480144325966965, -1.031721989605145051 ) ) ;
#30870 = FACE_OUTER_BOUND ( 'NONE', #30260, .T. ) ;
#30871 = ORIENTED_EDGE ( 'NONE', *, *, #13752, .F. ) ;
#30872 = CYLINDRICAL_SURFACE ( 'NONE', #25607, 11.00000000000000000 ) ;
#30873 = ADVANCED_FACE ( 'NONE', ( #3678 ), #26085, .F. ) ;
#30874 = ORIENTED_EDGE ( 'NONE', *, *, #20462, .T. ) ;
#30875 = DIRECTION ( 'NONE',  ( 0.000000000000000000, 0.000000000000000000, 1.000000000000000000 ) ) ;
#30876 = COORDINATED_UNIVERSAL_TIME_OFFSET ( 0, 0, .AHEAD. ) ;
#30878 = ORIENTED_EDGE ( 'NONE', *, *, #9062, .F. ) ;
#30877 = CARTESIAN_POINT ( 'NONE',  ( -4.317168503051449946, -7.715934794172482292, -1.499999999999999556 ) ) ;
#30879 = ORIENTED_EDGE ( 'NONE', *, *, #23541, .F. ) ;
#30880 = CARTESIAN_POINT ( 'NONE',  ( -2.940647560480709188, -11.38358483011127120, 1.743664474335998582 ) ) ;
#30881 = EDGE_CURVE ( 'NONE', #19151, #28496, #17663, .T. ) ;
#30882 = ORIENTED_EDGE ( 'NONE', *, *, #8073, .T. ) ;
#30883 = DIRECTION ( 'NONE',  ( 0.000000000000000000, 0.000000000000000000, 1.000000000000000000 ) ) ;
#30885 = EDGE_LOOP ( 'NONE', ( #31226, #16246, #13130, #20036 ) ) ;
#30884 = PLANE ( 'NONE',  #17072 ) ;
#30886 = CARTESIAN_POINT ( 'NONE',  ( 18.91213585445015610, 14.46970239064985719, 1.050000000000000044 ) ) ;
#30887 = FACE_OUTER_BOUND ( 'NONE', #22081, .T. ) ;
#30888 = DIRECTION ( 'NONE',  ( 1.000000000000000000, 0.000000000000000000, 0.000000000000000000 ) ) ;
#30889 = CARTESIAN_POINT ( 'NONE',  ( 0.5032039771612139001, 9.456648240374295966, -2.299586922890421103 ) ) ;
#30890 = ORIENTED_EDGE ( 'NONE', *, *, #1096, .F. ) ;
#30891 = CARTESIAN_POINT ( 'NONE',  ( 21.23500000273118715, 2.486304738420679783, -0.2613211581691337604 ) ) ;
#30892 = CARTESIAN_POINT ( 'NONE',  ( 102.8580990270160385, -4.820463887425400884, 4.522129901861162260 ) ) ;
#30893 = DIRECTION ( 'NONE',  ( 0.000000000000000000, -0.9993908270190956511, 0.03489949670250104552 ) ) ;
#30894 = DIRECTION ( 'NONE',  ( 0.000000000000000000, 0.000000000000000000, 1.000000000000000000 ) ) ;
#30895 = CARTESIAN_POINT ( 'NONE',  ( -8.000050799999998574, -1.094676798671502471, 2.924497836550261187 ) ) ;
#30896 = CARTESIAN_POINT ( 'NONE',  ( 21.03177542174473658, -17.18603084754145982, -1.753176640694677380 ) ) ;
#30897 = CARTESIAN_POINT ( 'NONE',  ( 23.80656763371926843, 0.8852964313267427388, -2.499999999999999112 ) ) ;
#30898 = DIRECTION ( 'NONE',  ( -0.6916610887771488247, 0.000000000000000000, -0.7222222222222250965 ) ) ;
#30899 = ORIENTED_EDGE ( 'NONE', *, *, #24908, .F. ) ;
#30900 = EDGE_CURVE ( 'NONE', #4370, #13391, #22577, .T. ) ;
#30901 = CARTESIAN_POINT ( 'NONE',  ( -5.462550801365593678, 3.521866450007987037, 0.3701630799359328372 ) ) ;
#30902 = ORIENTED_EDGE ( 'NONE', *, *, #25516, .T. ) ;
#30903 = CARTESIAN_POINT ( 'NONE',  ( -3.354531657079158347, 0.9198621039125853827, 3.105402419394639235 ) ) ;
#30904 = CARTESIAN_POINT ( 'NONE',  ( 108.0895235638783163, 18.67666245286735105, 4.597069131703993783 ) ) ;
#30905 = CARTESIAN_POINT ( 'NONE',  ( -3.424298583717139316E-16, -3.993798362933287383, -3.024842911000732215 ) ) ;
#30906 = CARTESIAN_POINT ( 'NONE',  ( 7.931701155948623239, -9.929036424222896784, 1.000000000000000000 ) ) ;
#30907 = EDGE_LOOP ( 'NONE', ( #18127, #15139, #12862 ) ) ;
#30908 = CARTESIAN_POINT ( 'NONE',  ( 28.71260074195899037, -4.863490077430783209, -2.787782631220622864 ) ) ;
#30909 = VERTEX_POINT ( 'NONE', #6330 ) ;
#30910 = CARTESIAN_POINT ( 'NONE',  ( -1.265925305626697234E-16, -1.476463073999670028, 4.787500056513361635 ) ) ;
#30911 = PERSON_AND_ORGANIZATION ( #6766, #25292 ) ;
#30912 = CARTESIAN_POINT ( 'NONE',  ( 102.4192815113620725, -3.941896998588075185, 4.073741746331570823 ) ) ;
#30913 = EDGE_CURVE ( 'NONE', #5967, #8298, #25664, .T. ) ;
#30914 = CARTESIAN_POINT ( 'NONE',  ( 9.295257658903679499, 0.2358351158402515468, 1.049999985396302904 ) ) ;
#30916 = FACE_OUTER_BOUND ( 'NONE', #11433, .T. ) ;
#30915 = CARTESIAN_POINT ( 'NONE',  ( 3.499999999999999556, 0.005878491403554959860, -7.047692205288322853 ) ) ;
#30917 = VERTEX_POINT ( 'NONE', #6021 ) ;
#30918 = CARTESIAN_POINT ( 'NONE',  ( 107.5617944031221640, -18.98359742639815551, -4.522129901861166701 ) ) ;
#30919 = DIRECTION ( 'NONE',  ( 0.000000000000000000, 0.8660254037844362651, 0.5000000000000038858 ) ) ;
#30920 = CARTESIAN_POINT ( 'NONE',  ( 9.096376384877638444, -0.1528062924499160868, 1.364612494264895837 ) ) ;
#30921 = CARTESIAN_POINT ( 'NONE',  ( -30.51827900900860158, 4.402097243136374516, 5.049999999999999822 ) ) ;
#30923 = EDGE_LOOP ( 'NONE', ( #25403, #14069, #25582, #5692 ) ) ;
#30922 = CARTESIAN_POINT ( 'NONE',  ( 0.5859972064454824769, -5.135271408404158855, 0.9788672205888330202 ) ) ;
#30924 = CARTESIAN_POINT ( 'NONE',  ( -5.912550801365592967, -3.675193018007246071, 1.088641768524163167 ) ) ;
#30925 = CARTESIAN_POINT ( 'NONE',  ( 6.038145268433180668, -6.771555838910892966, 5.096160642893628356 ) ) ;
#30926 = CARTESIAN_POINT ( 'NONE',  ( 18.69136968068997007, -6.627090290223585534, -2.787782631232023967 ) ) ;
#30927 = ORIENTED_EDGE ( 'NONE', *, *, #22373, .F. ) ;
#30928 = ORIENTED_EDGE ( 'NONE', *, *, #1566, .T. ) ;
#30929 = EDGE_CURVE ( 'NONE', #10505, #10948, #8361, .T. ) ;
#30930 = CARTESIAN_POINT ( 'NONE',  ( 108.5619817448483531, 15.65002148400668247, -0.4463807625373593657 ) ) ;
#30931 = CARTESIAN_POINT ( 'NONE',  ( 107.6996442589673819, 19.35565155597529596, -4.612695725900422872 ) ) ;
#30932 = EDGE_CURVE ( 'NONE', #72, #28120, #29594, .T. ) ;
#30933 = CARTESIAN_POINT ( 'NONE',  ( 22.17250000136559507, -3.024605502323851169, 0.3178988483021052969 ) ) ;
#30934 = CARTESIAN_POINT ( 'NONE',  ( 109.3697760341437970, 14.49066428361112813, -0.4463807625373593657 ) ) ;
#30935 = CARTESIAN_POINT ( 'NONE',  ( 2.425585535379221280, -9.314797388879910045, 5.239665997526856245 ) ) ;
#30936 = LINE ( 'NONE', #2528, #25787 ) ;
#30937 = CARTESIAN_POINT ( 'NONE',  ( 5.061877160328730696, 19.51744974835124680, 5.285536848417998534 ) ) ;
#30938 = ORIENTED_EDGE ( 'NONE', *, *, #16834, .F. ) ;
#30939 = CARTESIAN_POINT ( 'NONE',  ( -50.60000000000000142, -10.96966150227468972, -1.000000000000000000 ) ) ;
#30940 = DATE_TIME_ROLE ( 'classification_date' ) ;
#30941 = DIRECTION ( 'NONE',  ( -1.000000000000000000, -0.000000000000000000, -0.000000000000000000 ) ) ;
#30942 = ORIENTED_EDGE ( 'NONE', *, *, #4041, .F. ) ;
#30943 = CARTESIAN_POINT ( 'NONE',  ( 0.000000000000000000, 0.000000000000000000, 0.000000000000000000 ) ) ;
#30944 = ORIENTED_EDGE ( 'NONE', *, *, #21404, .T. ) ;
#30945 = CARTESIAN_POINT ( 'NONE',  ( 102.7595417042496706, -3.401262957566509204, 3.636029349014984202 ) ) ;
#30947 = ORIENTED_EDGE ( 'NONE', *, *, #8526, .F. ) ;
#30946 = CARTESIAN_POINT ( 'NONE',  ( 102.3836362560080033, -3.427337902198302366, -4.312042181584450518 ) ) ;
#30948 = ORIENTED_EDGE ( 'NONE', *, *, #4698, .F. ) ;
#30949 = CARTESIAN_POINT ( 'NONE',  ( 7.249760686538667009, -7.892520144992426268, -1.391664247347309535 ) ) ;
#30950 = FACE_OUTER_BOUND ( 'NONE', #20790, .T. ) ;
#30951 = DIRECTION ( 'NONE',  ( 0.000000000000000000, 0.2588190451025135785, 0.9659258262890703106 ) ) ;
#30952 = CARTESIAN_POINT ( 'NONE',  ( 41.45057005843676734, -9.239282957736854485, -1.915219082070897638 ) ) ;
#30953 = VECTOR ( 'NONE', #27109, 1000.000000000000000 ) ;
#30955 = VERTEX_POINT ( 'NONE', #19710 ) ;
#30954 = DIRECTION ( 'NONE',  ( -1.000000000000000000, 0.000000000000000000, 0.000000000000000000 ) ) ;
#30956 = DIRECTION ( 'NONE',  ( 0.000000000000000000, 1.000000000000000000, 0.000000000000000000 ) ) ;
#30957 = CARTESIAN_POINT ( 'NONE',  ( 22.17513219109303080, 17.52220421518676829, 1.500000000000000000 ) ) ;
#30958 = CARTESIAN_POINT ( 'NONE',  ( -3.176043528763360602, -11.78095770713099277, 1.499999999999999556 ) ) ;
#30959 = CARTESIAN_POINT ( 'NONE',  ( 7.249760686538667009, 0.000000000000000000, 0.000000000000000000 ) ) ;
#30960 = DIRECTION ( 'NONE',  ( 0.000000000000000000, 0.000000000000000000, 1.000000000000000000 ) ) ;
#30961 = EDGE_CURVE ( 'NONE', #7524, #24271, #21498, .T. ) ;
#30963 = ORIENTED_EDGE ( 'NONE', *, *, #13539, .T. ) ;
#30962 = CARTESIAN_POINT ( 'NONE',  ( 107.6641948605228123, -20.45809826282219746, -1.499999999999999556 ) ) ;
#30964 = LINE ( 'NONE', #30466, #16747 ) ;
#30965 = EDGE_CURVE ( 'NONE', #15944, #31023, #22063, .T. ) ;
#30966 = CARTESIAN_POINT ( 'NONE',  ( -29.87068905793955409, 13.45819068726228984, 1.895815882016619991 ) ) ;
#30967 = CARTESIAN_POINT ( 'NONE',  ( 22.11000000136559507, -3.156283516753370044, -0.9349337715887220401 ) ) ;
#30968 = CARTESIAN_POINT ( 'NONE',  ( -8.000050800000000351, 0.1053597294728410155, -2.998641260211496462 ) ) ;
#30969 = AXIS2_PLACEMENT_3D ( 'NONE', #10367, #25567, #27921 ) ;
#30970 = FACE_OUTER_BOUND ( 'NONE', #30775, .T. ) ;
#30971 = CARTESIAN_POINT ( 'NONE',  ( -3.105859910357408271, -0.009789559233441965172, -1.118159719381818018 ) ) ;
#30972 = EDGE_LOOP ( 'NONE', ( #5599, #20854, #27534, #5781 ) ) ;
#30973 = DIRECTION ( 'NONE',  ( -0.8571673007021120005, 1.049727191138618326E-16, 0.5150380749100547106 ) ) ;
#30974 = AXIS2_PLACEMENT_3D ( 'NONE', #29444, #6709, #16899 ) ;
#30975 = FACE_OUTER_BOUND ( 'NONE', #10111, .T. ) ;
#30976 = ORIENTED_EDGE ( 'NONE', *, *, #7811, .T. ) ;
#30977 =( BOUNDED_CURVE ( )  B_SPLINE_CURVE ( 2, ( #16997, #11505, #4312, #26889, #24700, #12501, #33057, #32568, #15171, #19863, #20538 ),
 .UNSPECIFIED., .F., .F. ) 
 B_SPLINE_CURVE_WITH_KNOTS ( ( 3, 2, 2, 2, 2, 3 ),
 ( 0.1966116191895003751, 0.2000000000000000111, 0.2250000000000000056, 0.2500000000000000000, 0.2750000000000000222, 0.2966116191895003529 ),
 .UNSPECIFIED. ) 
 CURVE ( )  GEOMETRIC_REPRESENTATION_ITEM ( )  RATIONAL_B_SPLINE_CURVE ( ( 0.9821626249036858880, 0.9896829947469992783, 1.000000000000000000, 0.9238795325112867385, 1.000000000000000000, 0.9238795325112867385, 1.000000000000000000, 0.9238795325112867385, 1.000000000000000000, 0.9341965377642874602, 0.9821626249036858880 ) ) 
 REPRESENTATION_ITEM ( '' )  );
#30978 = CYLINDRICAL_SURFACE ( 'NONE', #1807, 11.00000000000000000 ) ;
#30979 = CARTESIAN_POINT ( 'NONE',  ( 6.356382228872881512, -8.265862592379907170, -2.398350474622027662 ) ) ;
#30980 = DIRECTION ( 'NONE',  ( -1.000000000000000000, 0.000000000000000000, 0.000000000000000000 ) ) ;
#30982 = CARTESIAN_POINT ( 'NONE',  ( 107.9493749606654234, -17.34037414412194877, 4.559070180965012042 ) ) ;
#30981 = CARTESIAN_POINT ( 'NONE',  ( 102.9885081044300534, -6.698322160490901567, -0.07017451552783579571 ) ) ;
#30983 = ORIENTED_EDGE ( 'NONE', *, *, #18889, .F. ) ;
#30984 = FACE_OUTER_BOUND ( 'NONE', #31217, .T. ) ;
#30985 = ORIENTED_EDGE ( 'NONE', *, *, #12026, .F. ) ;
#30986 = DIRECTION ( 'NONE',  ( 0.000000000000000000, 0.000000000000000000, 1.000000000000000000 ) ) ;
#30988 = ORIENTED_EDGE ( 'NONE', *, *, #3048, .F. ) ;
#30987 = CARTESIAN_POINT ( 'NONE',  ( 24.38302348701595079, -17.39153354041035726, 1.380603655064675861 ) ) ;
#30989 = EDGE_LOOP ( 'NONE', ( #21571, #31700, #7369, #2787, #32915 ) ) ;
#30990 = CARTESIAN_POINT ( 'NONE',  ( 6.037141869538512395, -4.619542287584855522, -7.104659103919393814 ) ) ;
#30991 = VECTOR ( 'NONE', #5604, 1000.000000000000000 ) ;
#30992 = CARTESIAN_POINT ( 'NONE',  ( 13.06177556439308418, 19.50000000000000000, 8.787599961869133836 ) ) ;
#30993 = EDGE_CURVE ( 'NONE', #21159, #32554, #32092, .T. ) ;
#30995 = ORIENTED_EDGE ( 'NONE', *, *, #17718, .T. ) ;
#30994 = CARTESIAN_POINT ( 'NONE',  ( -3.312942406915326377, -5.022711880624455567E-15, 2.999999999999999556 ) ) ;
#30996 = VERTEX_POINT ( 'NONE', #1500 ) ;
#30997 = VECTOR ( 'NONE', #32684, 1000.000000000000000 ) ;
#30998 = CARTESIAN_POINT ( 'NONE',  ( 0.6630161036174202493, -9.073167597564687270, -1.769313562487350611 ) ) ;
#30999 = CARTESIAN_POINT ( 'NONE',  ( 21.65220420020125758, -21.84595744892894231, -1.292937544721162402 ) ) ;
#31000 = CARTESIAN_POINT ( 'NONE',  ( 107.9128139062042919, -20.39012166861468600, -1.488290602270338159 ) ) ;
#31001 = CARTESIAN_POINT ( 'NONE',  ( -8.000050800000000351, 3.673940397442060361E-16, 3.000000000000000444 ) ) ;
#31002 = CARTESIAN_POINT ( 'NONE',  ( 107.8806307222008627, -16.35047421165092985, 1.384330804614037236 ) ) ;
#31003 = AXIS2_PLACEMENT_3D ( 'NONE', #28694, #31525, #5641 ) ;
#31004 = DIRECTION ( 'NONE',  ( 0.000000000000000000, 0.000000000000000000, -1.000000000000000000 ) ) ;
#31005 = EDGE_CURVE ( 'NONE', #901, #12812, #14871, .T. ) ;
#31006 = DIRECTION ( 'NONE',  ( 0.9947025833170223263, 0.1027947991993880261, -0.000000000000000000 ) ) ;
#31007 = CARTESIAN_POINT ( 'NONE',  ( 35.27967220683390082, -7.797546999730709416, 2.184956776445863280 ) ) ;
#31008 = FACE_OUTER_BOUND ( 'NONE', #22143, .T. ) ;
#31009 = CARTESIAN_POINT ( 'NONE',  ( -30.13448816962999643, 4.180515498708627931, 5.128141679950118714 ) ) ;
#31010 = EDGE_LOOP ( 'NONE', ( #103, #7006, #13981, #28469 ) ) ;
#31011 = CARTESIAN_POINT ( 'NONE',  ( 0.000000000000000000, -1.239665997526818053, -9.314797388894906049 ) ) ;
#31012 = CIRCLE ( 'NONE', #7507, 0.5000000000000004441 ) ;
#31013 = ADVANCED_FACE ( 'NONE', ( #27221 ), #9342, .T. ) ;
#31014 = VECTOR ( 'NONE', #30407, 1000.000000000000000 ) ;
#31015 = CARTESIAN_POINT ( 'NONE',  ( 5.377543748152551650, -7.892520144992426268, -1.391664247347309535 ) ) ;
#31016 = CARTESIAN_POINT ( 'NONE',  ( 13.56178860298438593, 21.92012725262058481, -1.183869197697829279 ) ) ;
#31017 = ORIENTED_EDGE ( 'NONE', *, *, #7967, .F. ) ;
#31018 = TOROIDAL_SURFACE ( 'NONE', #2177, 300.0401151713995773, 1.799999999999978728 ) ;
#31019 = CIRCLE ( 'NONE', #16572, 0.5000000000000004441 ) ;
#31020 = CARTESIAN_POINT ( 'NONE',  ( 25.32128608521642832, -1.774145575271474540, 1.889914159312680919 ) ) ;
#31021 = ADVANCED_FACE ( 'NONE', ( #25037 ), #9162, .F. ) ;
#31022 = DIRECTION ( 'NONE',  ( 0.000000000000000000, 0.000000000000000000, 1.000000000000000000 ) ) ;
#31023 = VERTEX_POINT ( 'NONE', #11853 ) ;
#31024 = DIRECTION ( 'NONE',  ( 0.000000000000000000, 0.000000000000000000, -1.000000000000000000 ) ) ;
#31025 = AXIS2_PLACEMENT_3D ( 'NONE', #9704, #9881, #15041 ) ;
#31026 = ORIENTED_EDGE ( 'NONE', *, *, #1343, .F. ) ;
#31027 = DIRECTION ( 'NONE',  ( -1.000000000000000000, 8.574039729943019576E-17, 0.000000000000000000 ) ) ;
#31028 = ADVANCED_FACE ( 'NONE', ( #19552 ), #29750, .T. ) ;
#31029 = SECURITY_CLASSIFICATION_LEVEL ( 'unclassified' ) ;
#31030 = ORIENTED_EDGE ( 'NONE', *, *, #5897, .F. ) ;
#31031 = ORIENTED_EDGE ( 'NONE', *, *, #27235, .F. ) ;
#31032 = CARTESIAN_POINT ( 'NONE',  ( -2.794738735352966685, 0.000000000000000000, 1.508259000770582059 ) ) ;
#31033 = EDGE_LOOP ( 'NONE', ( #22442, #28723, #11101, #27835, #22950 ) ) ;
#31034 = CARTESIAN_POINT ( 'NONE',  ( 10.56183597391177464, -0.2499999999999476807, -5.003758587302151284 ) ) ;
#31036 = ORIENTED_EDGE ( 'NONE', *, *, #24442, .T. ) ;
#31035 = DIRECTION ( 'NONE',  ( 0.000000000000000000, 0.000000000000000000, 1.000000000000000000 ) ) ;
#31037 = CARTESIAN_POINT ( 'NONE',  ( 26.08945412691624099, 19.05746434167065928, 1.050000000000000044 ) ) ;
#31038 = DIRECTION ( 'NONE',  ( 0.000000000000000000, 0.000000000000000000, 1.000000000000000000 ) ) ;
#31039 = CIRCLE ( 'NONE', #27816, 4.999999999999997335 ) ;
#31040 = EDGE_CURVE ( 'NONE', #10337, #20196, #10301, .T. ) ;
#31041 = VECTOR ( 'NONE', #20520, 1000.000000000000000 ) ;
#31042 = DIRECTION ( 'NONE',  ( 1.000000000000000000, 0.000000000000000000, 0.000000000000000000 ) ) ;
#31043 = EDGE_CURVE ( 'NONE', #32504, #26433, #29217, .T. ) ;
#31044 = CARTESIAN_POINT ( 'NONE',  ( -5.175170698068149555, 0.5000000000000000000, -5.403836275575627290 ) ) ;
#31045 = AXIS2_PLACEMENT_3D ( 'NONE', #15619, #13411, #16726 ) ;
#31046 = AXIS2_PLACEMENT_3D ( 'NONE', #4109, #14431, #21811 ) ;
#31047 = ORIENTED_EDGE ( 'NONE', *, *, #4582, .T. ) ;
#31048 = AXIS2_PLACEMENT_3D ( 'NONE', #21, #5553, #10205 ) ;
#31049 = CARTESIAN_POINT ( 'NONE',  ( -3.800050800000000617, -1.887961173149512062, -2.331437884370912261 ) ) ;
#31050 = CARTESIAN_POINT ( 'NONE',  ( 0.1517578099453120721, -1.375880305419411309, -4.522129901861164925 ) ) ;
#31051 = CARTESIAN_POINT ( 'NONE',  ( 108.2850536699472883, 19.76545123595448672, 0.4463807625373348298 ) ) ;
#31052 = LINE ( 'NONE', #20838, #25889 ) ;
#31053 = CARTESIAN_POINT ( 'NONE',  ( 24.49428966819754194, -17.44778713273094084, 1.472392441597068613 ) ) ;
#31054 = CARTESIAN_POINT ( 'NONE',  ( 22.16007320322699314, -17.32365168620639650, -1.743368838329845572 ) ) ;
#31055 = CARTESIAN_POINT ( 'NONE',  ( 10.00000000000000000, 4.467071865485493731, -1.625881193364653088 ) ) ;
#31056 = CARTESIAN_POINT ( 'NONE',  ( 0.000000000000000000, 37.67766952966368876, 0.000000000000000000 ) ) ;
#31057 = CARTESIAN_POINT ( 'NONE',  ( -4.462550801365592790, -0.3701630799359326152, 3.521866450007987037 ) ) ;
#31058 = EDGE_LOOP ( 'NONE', ( #1307, #15416, #7099, #27237 ) ) ;
#31059 = EDGE_CURVE ( 'NONE', #32897, #2837, #9745, .T. ) ;
#31060 = CARTESIAN_POINT ( 'NONE',  ( -4.804531657079157192, -2.325406398514293205, 1.883076972206379818 ) ) ;
#31061 = CARTESIAN_POINT ( 'NONE',  ( 1.750000000000000222, -8.497168642645966941, 0.2193742428684632428 ) ) ;
#31062 = DIRECTION ( 'NONE',  ( -1.000000000000000000, 0.000000000000000000, 0.000000000000000000 ) ) ;
#31063 = CARTESIAN_POINT ( 'NONE',  ( 23.01404055077173183, -17.34213939868515553, 1.500000000000000000 ) ) ;
#31064 = ORIENTED_EDGE ( 'NONE', *, *, #20101, .T. ) ;
#31065 = DIRECTION ( 'NONE',  ( 0.000000000000000000, 0.7431448254773954654, -0.6691306063588569053 ) ) ;
#31066 = VECTOR ( 'NONE', #13512, 1000.000000000000114 ) ;
#31067 = AXIS2_PLACEMENT_3D ( 'NONE', #9275, #21501, #31714 ) ;
#31068 = AXIS2_PLACEMENT_3D ( 'NONE', #16837, #17158, #9126 ) ;
#31069 = B_SPLINE_CURVE_WITH_KNOTS ( 'NONE', 3,
 ( #3622, #23206, #18160, #23350, #950, #23504, #11129, #16314 ),
 .UNSPECIFIED., .F., .F.,
 ( 4, 2, 2, 4 ),
 ( 5.099451029764644560E-07, 0.001229190215587238830, 0.001843530350829370671, 0.002457870486071502512 ),
 .UNSPECIFIED. ) ;
#31070 = ORIENTED_EDGE ( 'NONE', *, *, #16235, .T. ) ;
#31071 = CARTESIAN_POINT ( 'NONE',  ( 2.386646147131364248, -0.3554301312245131683, 1.500000000000000000 ) ) ;
#31072 = APPLICATION_PROTOCOL_DEFINITION ( 'international standard', 'config_control_design', 1994, #19317 ) ;
#31073 = CARTESIAN_POINT ( 'NONE',  ( 102.4077201195289319, -3.775001509873114447, 4.215290384257519563 ) ) ;
#31074 = VECTOR ( 'NONE', #553, 999.9999999999998863 ) ;
#31075 = EDGE_CURVE ( 'NONE', #25757, #22634, #21286, .T. ) ;
#31076 = VECTOR ( 'NONE', #16788, 1000.000000000000227 ) ;
#31077 = VECTOR ( 'NONE', #18373, 1000.000000000000000 ) ;
#31078 = CARTESIAN_POINT ( 'NONE',  ( 7.064632879756605810, -8.466096581343467875, -2.210816291636299002 ) ) ;
#31080 = CARTESIAN_POINT ( 'NONE',  ( 7.249760686538667009, 7.135485519861997972, 5.064320921489847471 ) ) ;
#31079 = DIRECTION ( 'NONE',  ( 1.000000000000000000, -8.574039729943018344E-17, -0.000000000000000000 ) ) ;
#31081 = ORIENTED_EDGE ( 'NONE', *, *, #19838, .T. ) ;
#31082 = EDGE_CURVE ( 'NONE', #1994, #20387, #23096, .T. ) ;
#31083 = CARTESIAN_POINT ( 'NONE',  ( 5.489343806296449024, -7.976812024616034336, 1.512045527216178575 ) ) ;
#31084 = EDGE_CURVE ( 'NONE', #19335, #8885, #12111, .T. ) ;
#31085 = DIRECTION ( 'NONE',  ( 0.9896144216807900573, 0.000000000000000000, 0.1437473352845035912 ) ) ;
#31086 = CARTESIAN_POINT ( 'NONE',  ( 21.36000000136559507, -1.570731468192933633, -2.892927487894330074 ) ) ;
#31088 = ORIENTED_EDGE ( 'NONE', *, *, #12794, .T. ) ;
#31087 = CARTESIAN_POINT ( 'NONE',  ( 2.117172266158205751, -1.242920418748529432, 0.9788672205888330202 ) ) ;
#31089 = CARTESIAN_POINT ( 'NONE',  ( -6.562550801365594211, -2.228590825266444586, -2.752080473201636401 ) ) ;
#31090 = B_SPLINE_SURFACE_WITH_KNOTS ( 'NONE', 1, 3, ( 
 ( #28247, #28099, #23558, #10686, #679, #8356, #21081, #18058 ),
 ( #8019, #18406, #25578, #12861, #18552, #10379, #20588, #30797 ) ),
 .UNSPECIFIED., .F., .F., .F.,
 ( 2, 2 ),
 ( 4, 2, 2, 4 ),
 ( 0.000000000000000000, 1.000000000000000000 ),
 ( 0.000000000000000000, 0.5000000000000000000, 0.7500000000000000000, 1.000000000000000000 ),
 .UNSPECIFIED. ) ;
#31091 = B_SPLINE_CURVE_WITH_KNOTS ( 'NONE', 3,
 ( #4599, #2085, #29512, #27000, #4251, #24633, #22157, #17110 ),
 .UNSPECIFIED., .F., .F.,
 ( 4, 2, 2, 4 ),
 ( 2.333100327429635409E-07, 0.001262083418496911602, 0.001893008472728995983, 0.002523933526961080580 ),
 .UNSPECIFIED. ) ;
#31092 = DIRECTION ( 'NONE',  ( 1.000000000000000000, -8.574039729943018344E-17, -0.000000000000000000 ) ) ;
#31093 = CARTESIAN_POINT ( 'NONE',  ( 69.12694021457272697, -7.241784863855113663, -2.184957268911293493 ) ) ;
#31094 = ORIENTED_EDGE ( 'NONE', *, *, #18789, .F. ) ;
#31095 = EDGE_LOOP ( 'NONE', ( #5053, #24928, #9064, #9614 ) ) ;
#31096 = CIRCLE ( 'NONE', #7033, 2.750000000000000444 ) ;
#31097 = VECTOR ( 'NONE', #7163, 1000.000000000000000 ) ;
#31099 = AXIS2_PLACEMENT_3D ( 'NONE', #31480, #8562, #19603 ) ;
#31098 = CARTESIAN_POINT ( 'NONE',  ( 108.5970690979676334, 15.84540171098336714, -1.732900873336792547 ) ) ;
#31100 = CARTESIAN_POINT ( 'NONE',  ( 10.52034268205830259, -3.641590349731909537, -3.055657119358837992 ) ) ;
#31101 = AXIS2_PLACEMENT_3D ( 'NONE', #25591, #31134, #20601 ) ;
#31102 = CARTESIAN_POINT ( 'NONE',  ( 24.35832023931602208, -17.33818253687209676, 1.317734466820223549 ) ) ;
#31103 = VECTOR ( 'NONE', #14108, 1000.000000000000000 ) ;
#31104 = EDGE_CURVE ( 'NONE', #1745, #10723, #2971, .T. ) ;
#31105 = CARTESIAN_POINT ( 'NONE',  ( 0.08034253207417903220, -9.783802610459691351, 4.547003328334568550 ) ) ;
#31106 = CC_DESIGN_PERSON_AND_ORGANIZATION_ASSIGNMENT ( #13312, #18668, ( #7706 ) ) ;
#31107 = LINE ( 'NONE', #20581, #30074 ) ;
#31108 = CARTESIAN_POINT ( 'NONE',  ( 56.97280603064898941, -277.2763395528616002, -0.4463807625373608645 ) ) ;
#31109 = DIRECTION ( 'NONE',  ( -1.000000000000000000, 0.000000000000000000, 0.000000000000000000 ) ) ;
#31110 = EDGE_LOOP ( 'NONE', ( #16951, #22232, #14570, #13283 ) ) ;
#31111 = CARTESIAN_POINT ( 'NONE',  ( 6.524595395369781947, -2.369138865965884744, 8.328507089302171096 ) ) ;
#31112 = TOROIDAL_SURFACE ( 'NONE', #3359, 9.269952810656748809, 0.4500000000000000111 ) ;
#31113 = EDGE_LOOP ( 'NONE', ( #24953, #32389, #11037, #10620, #721 ) ) ;
#31115 = CIRCLE ( 'NONE', #16668, 0.5000000000000000000 ) ;
#31114 = PERSON_AND_ORGANIZATION_ROLE ( 'design_owner' ) ;
#31116 = DIRECTION ( 'NONE',  ( 1.000000000000000000, -8.574039729943018344E-17, -0.000000000000000000 ) ) ;
#31117 = CIRCLE ( 'NONE', #27345, 8.749000000000002331 ) ;
#31118 = ORIENTED_EDGE ( 'NONE', *, *, #25129, .F. ) ;
#31119 = ADVANCED_FACE ( 'NONE', ( #25395 ), #18031, .T. ) ;
#31120 = AXIS2_PLACEMENT_3D ( 'NONE', #9890, #19751, #4061 ) ;
#31121 = VECTOR ( 'NONE', #10561, 1000.000000000000000 ) ;
#31122 = CARTESIAN_POINT ( 'NONE',  ( 10.39650919157949893, -12.30877965038158450, -1.000000000000000000 ) ) ;
#31123 = ORIENTED_EDGE ( 'NONE', *, *, #31204, .T. ) ;
#31124 = DIRECTION ( 'NONE',  ( -1.000000000000000000, 0.000000000000000000, 0.000000000000000000 ) ) ;
#31127 = ORIENTED_EDGE ( 'NONE', *, *, #18107, .T. ) ;
#31126 = VECTOR ( 'NONE', #7730, 1000.000000000000227 ) ;
#31125 = CARTESIAN_POINT ( 'NONE',  ( 28.69019293160051731, -5.747507130675590048, -4.150065909478398041 ) ) ;
#31128 = EDGE_LOOP ( 'NONE', ( #25973, #30331, #1996, #13020 ) ) ;
#31129 = VECTOR ( 'NONE', #7174, 999.9999999999998863 ) ;
#31130 = DIRECTION ( 'NONE',  ( 0.000000000000000000, 0.000000000000000000, -1.000000000000000000 ) ) ;
#31131 = CARTESIAN_POINT ( 'NONE',  ( -4.012550801365593500, 1.828967928396027398, -3.368539882008727115 ) ) ;
#31132 = DIRECTION ( 'NONE',  ( -0.000000000000000000, -1.000000000000000000, -0.000000000000000000 ) ) ;
#31133 = AXIS2_PLACEMENT_3D ( 'NONE', #10001, #28070, #15504 ) ;
#31134 = DIRECTION ( 'NONE',  ( 0.000000000000000000, -0.5735764363510434949, -0.8191520442889936859 ) ) ;
#31136 = ORIENTED_EDGE ( 'NONE', *, *, #14012, .F. ) ;
#31135 = CARTESIAN_POINT ( 'NONE',  ( 20.31145943757101335, 16.24075847989571386, -1.499999999999999556 ) ) ;
#31137 = CARTESIAN_POINT ( 'NONE',  ( 5.865515302491333571, 15.00000000000002132, 1.508259000770582059 ) ) ;
#31138 = CARTESIAN_POINT ( 'NONE',  ( 0.000000000000000000, 19.50000000000000000, 6.818740222761507042 ) ) ;
#31139 = ADVANCED_BREP_SHAPE_REPRESENTATION ( '', ( #32572, #2865 ), #7102 ) ;
#31140 = CARTESIAN_POINT ( 'NONE',  ( -4.272725277965156110, -6.149870187536970789, 1.499999999999759304 ) ) ;
#31141 = CARTESIAN_POINT ( 'NONE',  ( 0.1574692421723833113, -7.841623826006576259, 7.165523657697594473 ) ) ;
#31142 = CARTESIAN_POINT ( 'NONE',  ( 44.05836296525849605, -19.40445080606635386, 1.499999999999999778 ) ) ;
#31144 = ORIENTED_EDGE ( 'NONE', *, *, #17710, .F. ) ;
#31143 = SPHERICAL_SURFACE ( 'NONE', #17094, 0.5000000000000000000 ) ;
#31145 = CYLINDRICAL_SURFACE ( 'NONE', #31195, 4.000000000000001776 ) ;
#31146 = VECTOR ( 'NONE', #29560, 1000.000000000000000 ) ;
#31147 = AXIS2_PLACEMENT_3D ( 'NONE', #25964, #5393, #7561 ) ;
#31148 = CARTESIAN_POINT ( 'NONE',  ( -13.84999999999999964, -10.96966150227469505, -1.499999999999999556 ) ) ;
#31149 = CARTESIAN_POINT ( 'NONE',  ( 24.61000000273118715, -1.573300977624594976, 1.942864903642425700 ) ) ;
#31150 = VECTOR ( 'NONE', #23953, 1000.000000000000000 ) ;
#31151 = EDGE_CURVE ( 'NONE', #27630, #9752, #16413, .T. ) ;
#31152 = AXIS2_PLACEMENT_3D ( 'NONE', #22628, #17578, #27781 ) ;
#31153 = LINE ( 'NONE', #8238, #9197 ) ;
#31154 = VECTOR ( 'NONE', #12198, 1000.000000000000000 ) ;
#31155 = DIRECTION ( 'NONE',  ( -0.000000000000000000, -0.000000000000000000, 1.000000000000000000 ) ) ;
#31156 = CARTESIAN_POINT ( 'NONE',  ( 107.9988851051869716, -18.05330790866155510, 4.637841734569910557 ) ) ;
#31157 = CARTESIAN_POINT ( 'NONE',  ( 12.44989959798878232, 0.4999999999999998890, 2.482234843104758060 ) ) ;
#31158 = ORIENTED_EDGE ( 'NONE', *, *, #19557, .F. ) ;
#31159 = LINE ( 'NONE', #6057, #21475 ) ;
#31160 = DIRECTION ( 'NONE',  ( -1.000000000000000000, 8.574039729943018344E-17, -3.081487911019577365E-33 ) ) ;
#31161 = DIRECTION ( 'NONE',  ( 8.574039729943018344E-17, 1.000000000000000000, 0.000000000000000000 ) ) ;
#31163 = CARTESIAN_POINT ( 'NONE',  ( 107.4499696397440545, -17.35889446679003356, 4.518584177339137753 ) ) ;
#31162 = CARTESIAN_POINT ( 'NONE',  ( 108.1104793158158230, 18.79335234840002400, -4.459574495179032816 ) ) ;
#31164 = EDGE_CURVE ( 'NONE', #11105, #9082, #26833, .T. ) ;
#31165 = VERTEX_POINT ( 'NONE', #20378 ) ;
#31166 = ADVANCED_FACE ( 'NONE', ( #12823 ), #27898, .T. ) ;
#31167 = CARTESIAN_POINT ( 'NONE',  ( 9.282537329959740902, 0.2172754300396697036, 1.050000000000000044 ) ) ;
#31168 = ORIENTED_EDGE ( 'NONE', *, *, #28687, .F. ) ;
#31169 = CARTESIAN_POINT ( 'NONE',  ( 85.45070076415389337, -7.158483446636730640, 2.713652344655544724 ) ) ;
#31170 = EDGE_CURVE ( 'NONE', #26634, #26820, #22823, .T. ) ;
#31171 = CIRCLE ( 'NONE', #2338, 0.5000000000000005551 ) ;
#31173 = ORIENTED_EDGE ( 'NONE', *, *, #20385, .T. ) ;
#31172 = DIRECTION ( 'NONE',  ( -4.458171167563057872E-29, 1.000000000000000000, 5.782411586589359611E-15 ) ) ;
#31174 = EDGE_LOOP ( 'NONE', ( #3922, #579, #9037, #8949, #15046 ) ) ;
#31175 = CARTESIAN_POINT ( 'NONE',  ( -8.000050800000009232, 2.460349816355251296, -2.612134329618188922 ) ) ;
#31176 = AXIS2_PLACEMENT_3D ( 'NONE', #16856, #27052, #4157 ) ;
#31177 = CIRCLE ( 'NONE', #21539, 8.749000000000002331 ) ;
#31178 = AXIS2_PLACEMENT_3D ( 'NONE', #1512, #31943, #9008 ) ;
#31179 = DIRECTION ( 'NONE',  ( -0.9896144216807899463, 0.000000000000000000, -0.1437473352845038410 ) ) ;
#31181 = ORIENTED_EDGE ( 'NONE', *, *, #13228, .T. ) ;
#31180 = DIRECTION ( 'NONE',  ( -0.000000000000000000, -0.000000000000000000, -1.000000000000000000 ) ) ;
#31182 = ORIENTED_EDGE ( 'NONE', *, *, #22303, .F. ) ;
#31183 = CARTESIAN_POINT ( 'NONE',  ( -2.762625878986976868, -11.69560895226267228, -1.743724257656045662 ) ) ;
#31184 = LINE ( 'NONE', #25639, #20369 ) ;
#31185 = CC_DESIGN_APPROVAL ( #9628, ( #12467 ) ) ;
#31186 = DIRECTION ( 'NONE',  ( 1.000000000000000000, 0.000000000000000000, 0.000000000000000000 ) ) ;
#31187 = CARTESIAN_POINT ( 'NONE',  ( 107.9803609742689900, -17.78656503166756764, -4.329962501461942281 ) ) ;
#31188 = CARTESIAN_POINT ( 'NONE',  ( 101.6304955275671773, -1.577711174297567354, 1.868788700125552094 ) ) ;
#31189 = DIRECTION ( 'NONE',  ( -0.000000000000000000, 0.000000000000000000, 1.000000000000000000 ) ) ;
#31190 = CARTESIAN_POINT ( 'NONE',  ( 2.632061376486628301, -0.5000000000000000000, 1.500000000000000000 ) ) ;
#31191 = CARTESIAN_POINT ( 'NONE',  ( 54.98781319022955927, -6.881869368925546127, 3.390608480947486125 ) ) ;
#31192 = CARTESIAN_POINT ( 'NONE',  ( -1.921189184902823754, -10.44034746380417467, 4.522129901861158707 ) ) ;
#31193 = CARTESIAN_POINT ( 'NONE',  ( 3.066081126419192504, 0.08824576070981422771, 0.7648597189984532863 ) ) ;
#31194 =( BOUNDED_SURFACE ( )  B_SPLINE_SURFACE ( 3, 2, ( 
 ( #25141, #17457, #2090 ),
 ( #27655, #22313, #27818 ),
 ( #32524, #4760, #30017 ),
 ( #9588, #14933, #19807 ) ),
 .UNSPECIFIED., .F., .F., .F. ) 
 B_SPLINE_SURFACE_WITH_KNOTS ( ( 4, 4 ),
 ( 3, 3 ),
 ( 0.004009623062827070289, 0.007419693412580972633 ),
 ( 0.000000000000000000, 1.000000000000000000 ),
 .UNSPECIFIED. ) 
 GEOMETRIC_REPRESENTATION_ITEM ( )  RATIONAL_B_SPLINE_SURFACE ( (
 ( 1.000000000000000000, 0.7074525376967367718, 1.000000000000000000),
 ( 1.000000000000000000, 0.7074519917808602676, 1.000000000000000000),
 ( 1.000000000000000000, 0.7074511013184006103, 1.000000000000000000),
 ( 1.000000000000000000, 0.7074498840443311787, 1.000000000000000000) ) ) 
 REPRESENTATION_ITEM ( '' )  SURFACE ( )  );
#31195 = AXIS2_PLACEMENT_3D ( 'NONE', #8231, #5220, #23107 ) ;
#31196 = VERTEX_POINT ( 'NONE', #159 ) ;
#31197 = CIRCLE ( 'NONE', #22636, 0.5000000000000004441 ) ;
#31198 = CARTESIAN_POINT ( 'NONE',  ( 6.357668022120090079, -5.959864878090717966, 6.210015626210365625 ) ) ;
#31199 = CIRCLE ( 'NONE', #17286, 5.000000000000002665 ) ;
#31200 = DIRECTION ( 'NONE',  ( -1.000000000000000000, 0.000000000000000000, -0.000000000000000000 ) ) ;
#31201 = DIRECTION ( 'NONE',  ( 1.000000000000000000, -0.000000000000000000, -0.000000000000000000 ) ) ;
#31202 = ORIENTED_EDGE ( 'NONE', *, *, #19387, .T. ) ;
#31203 = CARTESIAN_POINT ( 'NONE',  ( 24.61000000136559862, 2.892927487894327410, -1.570731468192931635 ) ) ;
#31204 = EDGE_CURVE ( 'NONE', #299, #9383, #15004, .T. ) ;
#31205 = DIRECTION ( 'NONE',  ( 0.000000000000000000, 0.000000000000000000, -1.000000000000000000 ) ) ;
#31206 = CARTESIAN_POINT ( 'NONE',  ( 20.03174988220904496, -21.67712946496369497, -1.441661034764752936 ) ) ;
#31207 = LOCAL_TIME ( 16, 7, 10.00000000000000000, #26537 ) ;
#31208 = ORIENTED_EDGE ( 'NONE', *, *, #618, .F. ) ;
#31209 = DIRECTION ( 'NONE',  ( 0.000000000000000000, 0.000000000000000000, 1.000000000000000000 ) ) ;
#31210 = ORIENTED_EDGE ( 'NONE', *, *, #14754, .F. ) ;
#31211 = CARTESIAN_POINT ( 'NONE',  ( -41.30970132048468457, -16.45499999999997343, 1.500000000000000000 ) ) ;
#31212 = PERSON_AND_ORGANIZATION_ROLE ( 'classification_officer' ) ;
#31214 = ORIENTED_EDGE ( 'NONE', *, *, #28290, .F. ) ;
#31213 = FACE_OUTER_BOUND ( 'NONE', #19126, .T. ) ;
#31215 = ORIENTED_EDGE ( 'NONE', *, *, #14071, .T. ) ;
#31216 = CARTESIAN_POINT ( 'NONE',  ( 24.73500000136559507, 1.570731468192929858, 2.892927487894329630 ) ) ;
#31217 = EDGE_LOOP ( 'NONE', ( #4781, #23479, #21789 ) ) ;
#31218 = CARTESIAN_POINT ( 'NONE',  ( -1.765934045424250254, -0.3164610288023907980, 3.010925563584172515 ) ) ;
#31219 = AXIS2_PLACEMENT_3D ( 'NONE', #24826, #19651, #20151 ) ;
#31221 = VERTEX_POINT ( 'NONE', #28219 ) ;
#31220 = FACE_OUTER_BOUND ( 'NONE', #30761, .T. ) ;
#31222 = CARTESIAN_POINT ( 'NONE',  ( 0.5032041927271373449, 6.298925283824191368, -7.418882907476054278 ) ) ;
#31223 = CARTESIAN_POINT ( 'NONE',  ( 108.0656705835203297, -19.01500218252613550, 3.248569211028260018 ) ) ;
#31224 = CARTESIAN_POINT ( 'NONE',  ( 10.00000000000000000, -3.672404558090063276, 3.407865132560168320 ) ) ;
#31225 = CARTESIAN_POINT ( 'NONE',  ( 3.499999999999999556, 0.000000000000000000, 0.000000000000000000 ) ) ;
#31226 = ORIENTED_EDGE ( 'NONE', *, *, #22071, .F. ) ;
#31227 = CYLINDRICAL_SURFACE ( 'NONE', #14418, 0.4499999999999990119 ) ;
#31228 = CARTESIAN_POINT ( 'NONE',  ( 4.749760686538667009, -6.139290821770289064, 5.151476664237455871 ) ) ;
#31229 = CARTESIAN_POINT ( 'NONE',  ( 23.63572006016191906, -7.640988024202735041, -1.873789191057743331 ) ) ;
#31230 = DIRECTION ( 'NONE',  ( 1.000000000000000000, -0.000000000000000000, -0.000000000000000000 ) ) ;
#31231 = CC_DESIGN_APPROVAL ( #15523, ( #16786 ) ) ;
#31232 = EDGE_CURVE ( 'NONE', #28176, #29851, #14535, .T. ) ;
#31233 = CARTESIAN_POINT ( 'NONE',  ( 24.65791283128423927, -17.47550391090821265, 1.495278912112739889 ) ) ;
#31234 = DIRECTION ( 'NONE',  ( -1.000000000000000000, 0.000000000000000000, 0.000000000000000000 ) ) ;
#31235 = CARTESIAN_POINT ( 'NONE',  ( 22.50111451137534502, -3.256483526998273983E-15, 2.499999999999998668 ) ) ;
#31236 = DIRECTION ( 'NONE',  ( 0.000000000000000000, 0.000000000000000000, -1.000000000000000000 ) ) ;
#31237 = EDGE_CURVE ( 'NONE', #20422, #10617, #26038, .T. ) ;
#31238 = CARTESIAN_POINT ( 'NONE',  ( -3.812550801365593323, 3.368539882008727115, 1.828967928396026954 ) ) ;
#31239 = ORIENTED_EDGE ( 'NONE', *, *, #4463, .T. ) ;
#31240 = CARTESIAN_POINT ( 'NONE',  ( -2.854531657079157903, 1.545410377633947174, -2.846291840500173365 ) ) ;
#31241 = VECTOR ( 'NONE', #32452, 1000.000000000000000 ) ;
#31242 = DIRECTION ( 'NONE',  ( -0.000000000000000000, 0.9659258262890683122, -0.2588190451025207950 ) ) ;
#31243 = EDGE_CURVE ( 'NONE', #23656, #26528, #20715, .T. ) ;
#31244 = DIRECTION ( 'NONE',  ( 0.000000000000000000, 0.000000000000000000, 1.000000000000000000 ) ) ;
#31245 = CARTESIAN_POINT ( 'NONE',  ( 12.29359089006352335, -13.32350401977120313, 1.500000000000832445 ) ) ;
#31246 = ORIENTED_EDGE ( 'NONE', *, *, #17976, .T. ) ;
#31247 = CARTESIAN_POINT ( 'NONE',  ( 102.3175034158304300, -2.480357097899213770, -3.390608474937876871 ) ) ;
#31248 = ORIENTED_EDGE ( 'NONE', *, *, #11276, .T. ) ;
#31249 = CARTESIAN_POINT ( 'NONE',  ( 0.8233106589072967108, -3.227070907846791403, 1.762270114843585533 ) ) ;
#31250 = PERSON_AND_ORGANIZATION ( #6766, #25292 ) ;
#31251 = CARTESIAN_POINT ( 'NONE',  ( 69.06576509455614143, -6.022595136392056681, 4.112224952814602652 ) ) ;
#31252 = EDGE_CURVE ( 'NONE', #30476, #17825, #15245, .T. ) ;
#31253 = CARTESIAN_POINT ( 'NONE',  ( 6.357667697713667465, -8.357963647880060520, -2.056386458247358551 ) ) ;
#31254 = CARTESIAN_POINT ( 'NONE',  ( 5.887530024394194150, 8.008238305624880482, -2.518482652462476157 ) ) ;
#31255 = VERTEX_POINT ( 'NONE', #6258 ) ;
#31256 = CARTESIAN_POINT ( 'NONE',  ( 0.6791199890552586105, 5.814932665552513313, 7.071625480714526901 ) ) ;
#31257 = CARTESIAN_POINT ( 'NONE',  ( 7.249760686538667009, 4.007137495034909236, -6.940565734314555257 ) ) ;
#31258 = CARTESIAN_POINT ( 'NONE',  ( 21.98500000136559507, -0.9349337715887248157, 3.156283516753367824 ) ) ;
#31259 = EDGE_CURVE ( 'NONE', #14980, #15111, #11376, .T. ) ;
#31261 = VERTEX_POINT ( 'NONE', #16443 ) ;
#31260 = DIRECTION ( 'NONE',  ( -1.000000000000000000, 0.000000000000000000, 0.000000000000000000 ) ) ;
#31262 = CARTESIAN_POINT ( 'NONE',  ( -2.562550801365592879, -2.228590825266444586, -2.752080473201636401 ) ) ;
#31263 = CARTESIAN_POINT ( 'NONE',  ( 4.749760686538667009, 7.530955069117551304, -2.741043480754851380 ) ) ;
#31264 = LINE ( 'NONE', #10514, #11258 ) ;
#31265 = VERTEX_POINT ( 'NONE', #3608 ) ;
#31266 = ORIENTED_EDGE ( 'NONE', *, *, #31560, .T. ) ;
#31267 = DIRECTION ( 'NONE',  ( -0.000000000000000000, -0.000000000000000000, -1.000000000000000000 ) ) ;
#31268 = DIRECTION ( 'NONE',  ( -0.000000000000000000, -0.000000000000000000, -1.000000000000000000 ) ) ;
#31269 = ORIENTED_EDGE ( 'NONE', *, *, #18345, .F. ) ;
#31270 = CLOSED_SHELL ( 'NONE', ( #14058, #29437, #31840, #4983, #27768, #19668, #30150, #3341, #31830, #4328, #8325, #18579, #19795, #24465, #18741, #19859, #23260, #22763, #20527, #32885, #20732, #24529, #9097, #7980, #4455, #13415, #12457 ) ) ;
#31271 = CARTESIAN_POINT ( 'NONE',  ( 25.36142496378537814, -17.53025290272828585, 1.090880951025948953 ) ) ;
#31272 = DIRECTION ( 'NONE',  ( -0.000000000000000000, 0.000000000000000000, 1.000000000000000000 ) ) ;
#31273 = DIRECTION ( 'NONE',  ( 0.000000000000000000, -0.9271838545667856479, -0.3746065934159163446 ) ) ;
#31274 = ADVANCED_FACE ( 'NONE', ( #3758 ), #11453, .F. ) ;
#31275 = CARTESIAN_POINT ( 'NONE',  ( 0.3076688720830436652, -10.24120291391357895, -0.9727984658976240873 ) ) ;
#31276 = CARTESIAN_POINT ( 'NONE',  ( 18.60402535544292490, -7.603424548862588672, 0.07017451552782096036 ) ) ;
#31277 = ORIENTED_EDGE ( 'NONE', *, *, #32437, .T. ) ;
#31278 = CARTESIAN_POINT ( 'NONE',  ( 3.020080204145390468, -7.542713057966098589, -4.831795131253294073 ) ) ;
#31279 = ADVANCED_FACE ( 'NONE', ( #8923 ), #11340, .T. ) ;
#31280 = ORIENTED_EDGE ( 'NONE', *, *, #13580, .F. ) ;
#31281 = COORDINATED_UNIVERSAL_TIME_OFFSET ( 0, 0, .AHEAD. ) ;
#31282 = CARTESIAN_POINT ( 'NONE',  ( -53.35155202832373078, 4.402097243136376292, 5.050000000000000711 ) ) ;
#31283 = EDGE_CURVE ( 'NONE', #6630, #3234, #2770, .T. ) ;
#31284 = ORIENTED_EDGE ( 'NONE', *, *, #9278, .T. ) ;
#31285 = CARTESIAN_POINT ( 'NONE',  ( -13.84999999999999964, -10.96966150227469505, -1.499999999999999556 ) ) ;
#31286 = VERTEX_POINT ( 'NONE', #14115 ) ;
#31287 = DIRECTION ( 'NONE',  ( 0.000000000000000000, 1.000000000000000000, 0.000000000000000000 ) ) ;
#31289 = VERTEX_POINT ( 'NONE', #23969 ) ;
#31288 = CARTESIAN_POINT ( 'NONE',  ( 28.68905448306377792, -5.791583630846771413, -4.185347664757491870 ) ) ;
#31290 = ORIENTED_EDGE ( 'NONE', *, *, #9103, .T. ) ;
#31291 = DIRECTION ( 'NONE',  ( 1.000000000000000000, -8.574039729943018344E-17, -0.000000000000000000 ) ) ;
#31292 = CARTESIAN_POINT ( 'NONE',  ( -3.062550801365593323, 3.521866450007987037, 0.3701630799359328372 ) ) ;
#31293 = CARTESIAN_POINT ( 'NONE',  ( 7.429379966294792581, -10.00822258298154388, 1.500000000000000000 ) ) ;
#31294 = EDGE_CURVE ( 'NONE', #12581, #13848, #32669, .T. ) ;
#31295 = LINE ( 'NONE', #13541, #26800 ) ;
#31297 = EDGE_LOOP ( 'NONE', ( #29007, #32265, #30452, #22956 ) ) ;
#31296 = CARTESIAN_POINT ( 'NONE',  ( 7.064423637759001728, 7.953573330858883850, -3.647351267792822149 ) ) ;
#31298 = CARTESIAN_POINT ( 'NONE',  ( -6.087550801365593678, -2.752080473201636845, 2.228590825266444586 ) ) ;
#31299 = CARTESIAN_POINT ( 'NONE',  ( 17.56297300373453041, 13.04222886866727826, 1.499999999999999112 ) ) ;
#31300 = DIRECTION ( 'NONE',  ( 0.9993908270190957621, 0.03489949670250133695, 0.000000000000000000 ) ) ;
#31301 = CARTESIAN_POINT ( 'NONE',  ( 22.36000000136559152, 0.9349337715887185984, -3.156283516753368268 ) ) ;
#31302 = CARTESIAN_POINT ( 'NONE',  ( 3.660726896358641014, -5.717472393966525748E-18, 1.077884872112069514 ) ) ;
#31304 = VERTEX_POINT ( 'NONE', #24316 ) ;
#31303 = CARTESIAN_POINT ( 'NONE',  ( -7.750050802731187183, 0.3135853898029611342, -2.983565686104819648 ) ) ;
#31305 = CARTESIAN_POINT ( 'NONE',  ( -59.37247738224319704, -6.026451378431818107, 5.049999999999999822 ) ) ;
#31306 = DIRECTION ( 'NONE',  ( 0.000000000000000000, -0.7071067811865570096, 0.7071067811865380248 ) ) ;
#31307 = CARTESIAN_POINT ( 'NONE',  ( 21.48500000136559507, 2.892927487894327410, -1.570731468192931635 ) ) ;
#31308 = CARTESIAN_POINT ( 'NONE',  ( 24.95054824997649590, -17.50694965296897365, 1.454185466667848869 ) ) ;
#31309 = CARTESIAN_POINT ( 'NONE',  ( -15.12340757463330476, -28.43932300454937590, -1.000000000000000000 ) ) ;
#31310 = CARTESIAN_POINT ( 'NONE',  ( -2.785986023666280786, -0.02407431902641572752, -1.185596063490282015 ) ) ;
#31311 = DIRECTION ( 'NONE',  ( 0.000000000000000000, -0.9848077530122079093, -0.1736481776669314414 ) ) ;
#31312 = ADVANCED_FACE ( 'NONE', ( #1576 ), #11763, .F. ) ;
#31313 = DIRECTION ( 'NONE',  ( 1.000000000000000000, 0.000000000000000000, 0.000000000000000000 ) ) ;
#31314 = ORIENTED_EDGE ( 'NONE', *, *, #18151, .T. ) ;
#31315 = CARTESIAN_POINT ( 'NONE',  ( 17.39502519978884010, -21.04076415203780215, 1.751145182513948129 ) ) ;
#31316 = CARTESIAN_POINT ( 'NONE',  ( -3.115565086446475895, -0.007767237976396394912, -1.107297703164631608 ) ) ;
#31317 = CARTESIAN_POINT ( 'NONE',  ( 41.20585001718415441, -8.497180311780732964, -0.07017451552784181867 ) ) ;
#31319 = CARTESIAN_POINT ( 'NONE',  ( 107.9496392939063298, -17.34418047704120269, 4.568272308424636385 ) ) ;
#31318 = CARTESIAN_POINT ( 'NONE',  ( 108.0375581208015205, 18.38729836123134831, -4.602450496903218280 ) ) ;
#31320 = VERTEX_POINT ( 'NONE', #474 ) ;
#31321 = LINE ( 'NONE', #15771, #5921 ) ;
#31322 = ORIENTED_EDGE ( 'NONE', *, *, #29356, .T. ) ;
#31323 = CARTESIAN_POINT ( 'NONE',  ( -7.948539046346460246, -3.109529733928910744, 0.8848824693245758155 ) ) ;
#31325 = ORIENTED_EDGE ( 'NONE', *, *, #32540, .F. ) ;
#31324 = DIRECTION ( 'NONE',  ( -1.000000000000000000, 8.574039729943018344E-17, -0.000000000000000000 ) ) ;
#31326 = ORIENTED_EDGE ( 'NONE', *, *, #6966, .T. ) ;
#31327 = CARTESIAN_POINT ( 'NONE',  ( 41.44567272411835290, -7.615257740949710197, -4.522129901861164036 ) ) ;
#31328 = EDGE_CURVE ( 'NONE', #2806, #15877, #4446, .T. ) ;
#31329 = CARTESIAN_POINT ( 'NONE',  ( 7.249760686538667009, -7.199384779417155045, 4.973063321323851760 ) ) ;
#31331 = ORIENTED_EDGE ( 'NONE', *, *, #20380, .F. ) ;
#31330 = CARTESIAN_POINT ( 'NONE',  ( 7.064423659272770273, -3.748318449931968832, 7.906491560605070745 ) ) ;
#31332 = ORIENTED_EDGE ( 'NONE', *, *, #27056, .F. ) ;
#31333 = CARTESIAN_POINT ( 'NONE',  ( -0.1873139951646253798, -14.67771805109925332, -1.745313736529866100 ) ) ;
#31334 = CARTESIAN_POINT ( 'NONE',  ( -10.00000000000000000, 0.000000000000000000, 0.000000000000000000 ) ) ;
#31335 = DIRECTION ( 'NONE',  ( 6.062761635205522753E-17, 0.7071067811865410224, 0.7071067811865540120 ) ) ;
#31336 = CARTESIAN_POINT ( 'NONE',  ( 107.9482084786819343, -17.32357709375119015, -4.515156556222997608 ) ) ;
#31337 = CARTESIAN_POINT ( 'NONE',  ( 12.44989959798877699, 0.5000000000000000000, 2.982234843104758060 ) ) ;
#31338 = CARTESIAN_POINT ( 'NONE',  ( 3.499999999999999556, 8.357095590591338663, -1.552080310331533486 ) ) ;
#31339 = CARTESIAN_POINT ( 'NONE',  ( 4.129189561419488896, -11.96871115988036394, 1.500000000000000888 ) ) ;
#31340 = LINE ( 'NONE', #18612, #29077 ) ;
#31341 = ADVANCED_FACE ( 'NONE', ( #16948 ), #20866, .T. ) ;
#31342 = CARTESIAN_POINT ( 'NONE',  ( -1.218076164763124636, -14.00532792343563848, 1.500000000000000000 ) ) ;
#31343 = FACE_OUTER_BOUND ( 'NONE', #20662, .T. ) ;
#31344 = ORIENTED_EDGE ( 'NONE', *, *, #7108, .T. ) ;
#31345 = CARTESIAN_POINT ( 'NONE',  ( -29.24402871571405882, -27.93932300454937590, 11.00000000000000000 ) ) ;
#31346 = EDGE_CURVE ( 'NONE', #25565, #29734, #4359, .T. ) ;
#31347 = CARTESIAN_POINT ( 'NONE',  ( 107.7530755790422319, 16.80318731729154891, 2.547137921104602132 ) ) ;
#31348 = CARTESIAN_POINT ( 'NONE',  ( 18.68265047573912341, -6.724553502642427461, -4.522129901861163148 ) ) ;
#31349 = VERTEX_POINT ( 'NONE', #17604 ) ;
#31350 = CARTESIAN_POINT ( 'NONE',  ( 22.42250000136559507, -0.3178988483021076838, -3.024605502323848949 ) ) ;
#31351 = CARTESIAN_POINT ( 'NONE',  ( 25.55608012950906982, -0.1743803405538818241, -2.821080129508247936 ) ) ;
#31352 = CARTESIAN_POINT ( 'NONE',  ( 17.75999999999999801, -1.902510934646483477E-15, 2.499999999999996891 ) ) ;
#31353 = ORIENTED_EDGE ( 'NONE', *, *, #18502, .T. ) ;
#31354 = CARTESIAN_POINT ( 'NONE',  ( 0.7531256266104227048, -8.135089508258609214, -1.499999999999999778 ) ) ;
#31355 = VERTEX_POINT ( 'NONE', #19638 ) ;
#31356 = ORIENTED_EDGE ( 'NONE', *, *, #25009, .F. ) ;
#31357 = CARTESIAN_POINT ( 'NONE',  ( 107.6641948605228123, -20.45809826282219746, -1.499999999999999556 ) ) ;
#31358 = B_SPLINE_SURFACE_WITH_KNOTS ( 'NONE', 3, 3, ( 
 ( #28242, #8499, #5686, #18699, #5350, #13340, #28593, #15721, #10679, #31276 ),
 ( #26243, #15864, #8013, #13522, #18548, #23735, #23390, #3525, #3178, #18213 ),
 ( #25926, #21074, #28738, #28901, #3033, #28421, #496, #11025, #8351, #10524 ),
 ( #21224, #6008, #13680, #10375, #5537, #8198, #18399, #23552, #672, #20583 ),
 ( #5829, #7863, #18055, #15536, #25749, #2880, #13046, #23246, #24032, #21377 ),
 ( #23883, #24222, #9150, #29585, #1651, #4323, #19544, #21864, #17008, #14006 ),
 ( #13826, #11354, #8986, #6319, #992, #21557, #31768, #29236, #22051, #1158 ) ),
 .UNSPECIFIED., .F., .F., .F.,
 ( 4, 3, 4 ),
 ( 4, 3, 3, 4 ),
 ( -8.385610576351451352E-15, 0.4999999999999957812, 1.000000000000000000 ),
 ( 0.003581794793000731177, 0.5017908973965004016, 0.7508954486982502008, 1.000000000000000000 ),
 .UNSPECIFIED. ) ;
#31359 = PERSON_AND_ORGANIZATION ( #26331, #20535 ) ;
#31361 = VERTEX_POINT ( 'NONE', #7409 ) ;
#31360 = CARTESIAN_POINT ( 'NONE',  ( 14.21659522551972010, -20.98447794504473762, -0.9788672205760856615 ) ) ;
#31362 = ORIENTED_EDGE ( 'NONE', *, *, #8704, .F. ) ;
#31363 = CARTESIAN_POINT ( 'NONE',  ( 24.36000000136559507, 0.9349337715887185984, -3.156283516753368268 ) ) ;
#31364 = ORIENTED_EDGE ( 'NONE', *, *, #31252, .T. ) ;
#31365 = CARTESIAN_POINT ( 'NONE',  ( -7.357304906975410397, 1.062355717592093463, 3.000000000000000000 ) ) ;
#31367 = ORIENTED_EDGE ( 'NONE', *, *, #26118, .F. ) ;
#31366 = CARTESIAN_POINT ( 'NONE',  ( 23.86731473546760540, -3.600650094290393621, -1.169950778968975369 ) ) ;
#31368 = DIRECTION ( 'NONE',  ( 0.000000000000000000, -0.9945218953682744001, 0.1045284632676436593 ) ) ;
#31369 = CARTESIAN_POINT ( 'NONE',  ( -7.077711312404032898E-17, -0.8254815157534933778, -4.681538312723525053 ) ) ;
#31370 = CARTESIAN_POINT ( 'NONE',  ( 0.000000000000000000, 0.000000000000000000, 0.000000000000000000 ) ) ;
#31371 = CARTESIAN_POINT ( 'NONE',  ( 25.56776753627337229, -17.11417227705151589, -0.9999999999999993339 ) ) ;
#31372 = CARTESIAN_POINT ( 'NONE',  ( 107.5611841629995098, -18.97506626684318931, 4.544690123031810636 ) ) ;
#31373 = DIRECTION ( 'NONE',  ( 0.000000000000000000, 0.000000000000000000, 1.000000000000000000 ) ) ;
#31374 = CARTESIAN_POINT ( 'NONE',  ( 10.00000000000000178, -2.718385644597206330, 4.208382051008184632 ) ) ;
#31375 = CYLINDRICAL_SURFACE ( 'NONE', #14993, 4.000000000000001776 ) ;
#31376 = EDGE_CURVE ( 'NONE', #15578, #16944, #27623, .T. ) ;
#31377 = DIRECTION ( 'NONE',  ( 0.000000000000000000, -0.5735764363510537089, 0.8191520442889864695 ) ) ;
#31378 = ADVANCED_FACE ( 'NONE', ( #27809 ), #4924, .F. ) ;
#31379 = ADVANCED_FACE ( 'NONE', ( #22305 ), #32516, .T. ) ;
#31380 = LINE ( 'NONE', #1102, #11799 ) ;
#31381 = CARTESIAN_POINT ( 'NONE',  ( 4.749760686538667009, 7.892520144992453801, -1.391664247347147443 ) ) ;
#31382 = DIRECTION ( 'NONE',  ( 0.4999999999999977796, 0.8660254037844398178, 0.000000000000000000 ) ) ;
#31383 = CARTESIAN_POINT ( 'NONE',  ( 22.01492382911872880, -21.80158502930289544, 1.372788961212862313 ) ) ;
#31384 = DIRECTION ( 'NONE',  ( -1.000000000000000000, 0.000000000000000000, 0.000000000000000000 ) ) ;
#31385 = CARTESIAN_POINT ( 'NONE',  ( -4.212550801365593678, -3.368539882008727115, -1.828967928396028064 ) ) ;
#31386 = ORIENTED_EDGE ( 'NONE', *, *, #14721, .T. ) ;
#31387 = CARTESIAN_POINT ( 'NONE',  ( -5.550050800000001061, -3.113457007523259268, 0.9222479816126455399 ) ) ;
#31388 = CARTESIAN_POINT ( 'NONE',  ( 108.1863001008973555, 19.21555239728606779, 4.746593323837460687 ) ) ;
#31389 = CARTESIAN_POINT ( 'NONE',  ( -12.44989959798873791, -0.06979899340500209104, -1.001218345961804257 ) ) ;
#31390 = CARTESIAN_POINT ( 'NONE',  ( 8.103242287716968306, -10.98376420866808978, 1.500000000000000000 ) ) ;
#31391 = VERTEX_POINT ( 'NONE', #22151 ) ;
#31392 = CARTESIAN_POINT ( 'NONE',  ( 18.92745801356166169, -3.988096551854396488, -2.787782631232336161 ) ) ;
#31393 = ORIENTED_EDGE ( 'NONE', *, *, #2151, .F. ) ;
#31394 = LINE ( 'NONE', #26206, #23586 ) ;
#31395 = COORDINATED_UNIVERSAL_TIME_OFFSET ( 0, 0, .AHEAD. ) ;
#31396 = CARTESIAN_POINT ( 'NONE',  ( 84.98546029191203388, -4.383222815445155796, 4.275175582421200993 ) ) ;
#31397 = DIRECTION ( 'NONE',  ( 0.000000000000000000, -0.7071067811865465735, -0.7071067811865484609 ) ) ;
#31398 = CARTESIAN_POINT ( 'NONE',  ( 11.90652295052632503, 20.12228623747235901, 4.629213727441584325 ) ) ;
#31399 = ORIENTED_EDGE ( 'NONE', *, *, #11569, .F. ) ;
#31400 = CARTESIAN_POINT ( 'NONE',  ( 107.8192447519188306, -18.91582588990454639, -4.500896179815041087 ) ) ;
#31401 = DIRECTION ( 'NONE',  ( -1.000000000000000000, 8.574039729943018344E-17, -0.000000000000000000 ) ) ;
#31402 = CARTESIAN_POINT ( 'NONE',  ( 2.661997627134198741, -7.629706518865811304, -6.664939678585263927 ) ) ;
#31403 = ADVANCED_FACE ( 'NONE', ( #14615 ), #32859, .T. ) ;
#31405 = ORIENTED_EDGE ( 'NONE', *, *, #23840, .F. ) ;
#31404 = DIRECTION ( 'NONE',  ( -1.000000000000000000, 0.000000000000000000, 0.000000000000000000 ) ) ;
#31406 = CARTESIAN_POINT ( 'NONE',  ( -2.962550801365593234, 2.228590825266444142, 2.752080473201636845 ) ) ;
#31407 = CARTESIAN_POINT ( 'NONE',  ( 108.3696618535068126, 20.23658298680886958, 1.395260099363828665 ) ) ;
#31408 = CARTESIAN_POINT ( 'NONE',  ( 23.68974245684628244, -6.697273116524492309, -3.390608483637468584 ) ) ;
#31409 = ORIENTED_EDGE ( 'NONE', *, *, #17119, .T. ) ;
#31410 = ORIENTED_EDGE ( 'NONE', *, *, #8473, .T. ) ;
#31411 = EDGE_CURVE ( 'NONE', #16537, #18185, #32363, .T. ) ;
#31412 = CARTESIAN_POINT ( 'NONE',  ( 3.249999999999999556, -4.057423117305330784, -8.475820894093018865 ) ) ;
#31413 = CYLINDRICAL_SURFACE ( 'NONE', #10733, 2.999999999999999112 ) ;
#31414 = LINE ( 'NONE', #13814, #24753 ) ;
#31415 = CARTESIAN_POINT ( 'NONE',  ( 0.5220033361344494915, 0.000000000000000000, 5.485967528433933538 ) ) ;
#31416 = EDGE_CURVE ( 'NONE', #11749, #7524, #18458, .T. ) ;
#31417 = CYLINDRICAL_SURFACE ( 'NONE', #3391, 3.000000000000000444 ) ;
#31418 = CARTESIAN_POINT ( 'NONE',  ( 0.000000000000000000, -9.884132761439094139, 4.709950686174575907 ) ) ;
#31419 = CARTESIAN_POINT ( 'NONE',  ( -1.799351409542603308, -0.03945526729468277344, 3.068704260183690913 ) ) ;
#31420 = EDGE_CURVE ( 'NONE', #22752, #20668, #17300, .T. ) ;
#31421 = CARTESIAN_POINT ( 'NONE',  ( -3.087550801365593234, 2.228590825266444142, 2.752080473201636845 ) ) ;
#31422 = CYLINDRICAL_SURFACE ( 'NONE', #11916, 4.000000000000001776 ) ;
#31423 = CARTESIAN_POINT ( 'NONE',  ( 7.249760686538667009, 2.318425219014230265, 8.437262856154170265 ) ) ;
#31424 = VERTEX_POINT ( 'NONE', #27648 ) ;
#31425 = CARTESIAN_POINT ( 'NONE',  ( 6.356382228872880624, -2.398350474622000128, 8.265862592379914275 ) ) ;
#31426 = ORIENTED_EDGE ( 'NONE', *, *, #3260, .T. ) ;
#31427 = PERSON_AND_ORGANIZATION_ROLE ( 'creator' ) ;
#31428 = EDGE_CURVE ( 'NONE', #993, #12444, #29834, .T. ) ;
#31429 = DIRECTION ( 'NONE',  ( 1.000000000000000000, -8.574039729943018344E-17, -0.000000000000000000 ) ) ;
#31430 = CARTESIAN_POINT ( 'NONE',  ( 8.099355570077825917, -10.14921976342372467, -1.000000000000000000 ) ) ;
#31431 = ORIENTED_EDGE ( 'NONE', *, *, #6609, .T. ) ;
#31432 = CYLINDRICAL_SURFACE ( 'NONE', #32726, 8.749000000000002331 ) ;
#31433 = ADVANCED_FACE ( 'NONE', ( #6910 ), #14923, .F. ) ;
#31434 = ORIENTED_EDGE ( 'NONE', *, *, #25300, .T. ) ;
#31435 = VERTEX_POINT ( 'NONE', #12600 ) ;
#31436 = DIRECTION ( 'NONE',  ( -0.4809547266710045288, -0.000000000000000000, -0.8767454310646958238 ) ) ;
#31437 = CARTESIAN_POINT ( 'NONE',  ( -5.462550801365593678, 3.521866450007987037, 0.3701630799359328372 ) ) ;
#31438 = CARTESIAN_POINT ( 'NONE',  ( 17.05941372759280483, -15.60161612857925739, 1.500000000000000222 ) ) ;
#31439 = CARTESIAN_POINT ( 'NONE',  ( 0.3844419896858671248, -5.169620074766034357, -1.500000000000035083 ) ) ;
#31441 = EDGE_LOOP ( 'NONE', ( #2275, #25558, #16129, #29982, #9737 ) ) ;
#31440 = CARTESIAN_POINT ( 'NONE',  ( 13.23256811278013778, 7.534661545873150068, -1.499999999999999778 ) ) ;
#31442 = CARTESIAN_POINT ( 'NONE',  ( -5.037550801365593856, -1.088641768524163389, -3.675193018007246071 ) ) ;
#31443 = CARTESIAN_POINT ( 'NONE',  ( 9.302055952181040865, 0.2457637073014104223, 1.500000000000000000 ) ) ;
#31444 = CARTESIAN_POINT ( 'NONE',  ( -5.304000690461529555E-12, -21.43932300456189566, 1.000000000000000000 ) ) ;
#31446 = ADVANCED_FACE ( 'NONE', ( #14771 ), #17105, .F. ) ;
#31445 = CARTESIAN_POINT ( 'NONE',  ( 3.063284526839890720, 6.772677083992379110, 5.538577986808916442 ) ) ;
#31448 = ORIENTED_EDGE ( 'NONE', *, *, #25073, .T. ) ;
#31447 = DIRECTION ( 'NONE',  ( 6.062761635205574522E-17, 0.7071067811865465735, -0.7071067811865484609 ) ) ;
#31449 = EDGE_CURVE ( 'NONE', #26510, #21433, #3834, .T. ) ;
#31450 = CARTESIAN_POINT ( 'NONE',  ( -27.70354918513814368, 5.575484043998305772, 2.102665754804134313 ) ) ;
#31451 = CARTESIAN_POINT ( 'NONE',  ( 21.73500000273118715, -2.486304738420683780, 0.2613211581691335383 ) ) ;
#31452 = EDGE_CURVE ( 'NONE', #25735, #8635, #26785, .T. ) ;
#31453 = CARTESIAN_POINT ( 'NONE',  ( 10.00000000000000000, 3.641590349731929077, 3.055657119358814011 ) ) ;
#31454 = CARTESIAN_POINT ( 'NONE',  ( 16.10106094948405797, 19.71584668020019038, 5.412820279296879811 ) ) ;
#31455 = CARTESIAN_POINT ( 'NONE',  ( 5.377543748152548986, -6.139290821770289064, 5.151476664237455871 ) ) ;
#31456 = DIRECTION ( 'NONE',  ( -1.000000000000000000, 0.000000000000000000, -0.000000000000000000 ) ) ;
#31457 = CARTESIAN_POINT ( 'NONE',  ( -60.22964952008683781, -5.531562813905958720, 2.028141679950118625 ) ) ;
#31458 = CARTESIAN_POINT ( 'NONE',  ( -6.037550801365592967, -3.675193018007246071, 1.088641768524163167 ) ) ;
#31459 = ORIENTED_EDGE ( 'NONE', *, *, #3981, .F. ) ;
#31460 = ADVANCED_FACE ( 'NONE', ( #20144 ), #15779, .F. ) ;
#31461 = CARTESIAN_POINT ( 'NONE',  ( 20.05745782660446608, -21.55152848446436309, 1.510982242220422433 ) ) ;
#31462 = DIRECTION ( 'NONE',  ( 1.000000000000000000, -8.574039729943018344E-17, -0.000000000000000000 ) ) ;
#31463 = CYLINDRICAL_SURFACE ( 'NONE', #12259, 0.4500000000000025646 ) ;
#31465 = CARTESIAN_POINT ( 'NONE',  ( 108.0106719622584848, -18.22303571829002422, 4.627257122494635055 ) ) ;
#31464 = DIRECTION ( 'NONE',  ( 0.000000000000000000, 1.000000000000000000, 0.000000000000000000 ) ) ;
#31466 = ORIENTED_EDGE ( 'NONE', *, *, #2443, .F. ) ;
#31467 = CARTESIAN_POINT ( 'NONE',  ( 7.249760686538667009, 0.8180878109962995692, -8.711672189281419065 ) ) ;
#31468 = ORIENTED_EDGE ( 'NONE', *, *, #9492, .T. ) ;
#31469 = CARTESIAN_POINT ( 'NONE',  ( -7.998722633285748174, -2.371517779863575370, 1.837526800715260533 ) ) ;
#31471 = ORIENTED_EDGE ( 'NONE', *, *, #20462, .F. ) ;
#31470 = CARTESIAN_POINT ( 'NONE',  ( -50.81000000000000227, -10.96999999999998643, 1.949999999999999956 ) ) ;
#31472 = EDGE_LOOP ( 'NONE', ( #13921, #30489, #9725, #3001 ) ) ;
#31473 = FACE_OUTER_BOUND ( 'NONE', #21088, .T. ) ;
#31474 = ADVANCED_FACE ( 'NONE', ( #13400 ), #5247, .T. ) ;
#31475 = DIRECTION ( 'NONE',  ( 0.000000000000000000, 0.000000000000000000, 1.000000000000000000 ) ) ;
#31477 = ORIENTED_EDGE ( 'NONE', *, *, #8102, .F. ) ;
#31476 = CARTESIAN_POINT ( 'NONE',  ( 107.9391920281211839, 17.83955714378018342, 3.608571156949641257 ) ) ;
#31478 = CARTESIAN_POINT ( 'NONE',  ( 16.86324541463584481, 12.23239806835116816, -1.499999999999407585 ) ) ;
#31479 = CARTESIAN_POINT ( 'NONE',  ( -1.487278458322581098, -13.44708787814461637, -1.744337816817864262 ) ) ;
#31480 = CARTESIAN_POINT ( 'NONE',  ( 10.00000000000000178, -8.574039729943018837E-16, 0.000000000000000000 ) ) ;
#31481 = EDGE_CURVE ( 'NONE', #4711, #18415, #9174, .T. ) ;
#31482 = CARTESIAN_POINT ( 'NONE',  ( 9.851448552575103434, -11.91728849018499581, -1.000000000000000000 ) ) ;
#31483 = CARTESIAN_POINT ( 'NONE',  ( -3.100050802731187272, -2.853674364686378695, -1.549418761218566809 ) ) ;
#31484 = EDGE_CURVE ( 'NONE', #20064, #4337, #32802, .T. ) ;
#31485 = DIRECTION ( 'NONE',  ( -1.000000000000000000, -0.000000000000000000, 0.000000000000000000 ) ) ;
#31486 = CIRCLE ( 'NONE', #33087, 10.99999999999999822 ) ;
#31487 = CIRCLE ( 'NONE', #26142, 0.4499999999999990119 ) ;
#31488 = CARTESIAN_POINT ( 'NONE',  ( 7.249760686538667009, -6.226446564517957860, 6.147671362329200306 ) ) ;
#31489 = LINE ( 'NONE', #9905, #21622 ) ;
#31490 = CARTESIAN_POINT ( 'NONE',  ( 6.037141848526923482, 8.105561522824309861, 2.473100090966190656 ) ) ;
#31491 = CARTESIAN_POINT ( 'NONE',  ( 2.748213864407174079, 0.2993382933193597939, 1.561876010259294789 ) ) ;
#31492 = AXIS2_PLACEMENT_3D ( 'NONE', #10931, #1048, #10749 ) ;
#31493 = EDGE_LOOP ( 'NONE', ( #32352, #10881, #4899, #24554, #4990 ) ) ;
#31494 = CARTESIAN_POINT ( 'NONE',  ( 19.01480233880806381, -3.011762293215139330, 0.07017451552781951707 ) ) ;
#31495 = FACE_OUTER_BOUND ( 'NONE', #22293, .T. ) ;
#31496 = CARTESIAN_POINT ( 'NONE',  ( 12.84707270680543267, 21.67305773080836673, -1.472686733844490004 ) ) ;
#31497 = VERTEX_POINT ( 'NONE', #25982 ) ;
#31498 = ADVANCED_FACE ( 'NONE', ( #28302 ), #15921, .F. ) ;
#31499 = CARTESIAN_POINT ( 'NONE',  ( 25.42165046702202602, -2.650206603605265610, -0.4742644350702509004 ) ) ;
#31500 = CARTESIAN_POINT ( 'NONE',  ( 18.06290729145209184, -21.14813556147793605, 1.751201132231453572 ) ) ;
#31501 = ORIENTED_EDGE ( 'NONE', *, *, #2032, .T. ) ;
#31502 = CARTESIAN_POINT ( 'NONE',  ( 0.8194515883087264418, -4.592504314968420154, -1.499999999999999334 ) ) ;
#31503 = VERTEX_POINT ( 'NONE', #10583 ) ;
#31504 = AXIS2_PLACEMENT_3D ( 'NONE', #20681, #12975, #31035 ) ;
#31505 = ORIENTED_EDGE ( 'NONE', *, *, #26118, .T. ) ;
#31506 = CARTESIAN_POINT ( 'NONE',  ( 25.52557090713695231, -17.56218951387349492, -1.057622280107180845 ) ) ;
#31507 = DATE_TIME_ROLE ( 'classification_date' ) ;
#31509 = EDGE_LOOP ( 'NONE', ( #21955, #25363, #11360, #13767, #4911 ) ) ;
#31508 = DIRECTION ( 'NONE',  ( 0.000000000000000000, -0.08715574274766220431, 0.9961946980917452121 ) ) ;
#31510 = VERTEX_POINT ( 'NONE', #15423 ) ;
#31511 = CARTESIAN_POINT ( 'NONE',  ( 20.50111451137534857, -3.256483526998273983E-15, 2.499999999999998668 ) ) ;
#31512 = B_SPLINE_CURVE_WITH_KNOTS ( 'NONE', 3,
 ( #28592, #18398, #13339, #8673, #18891, #19043, #26074, #16358, #29235, #23551 ),
 .UNSPECIFIED., .F., .F.,
 ( 4, 2, 2, 2, 4 ),
 ( 0.000000000000000000, 0.0003394344854501923632, 0.0006788689709003847264, 0.001018303456350577035, 0.001357737941800769453 ),
 .UNSPECIFIED. ) ;
#31513 = ADVANCED_FACE ( 'NONE', ( #25633 ), #2748, .T. ) ;
#31514 = VERTEX_POINT ( 'NONE', #13102 ) ;
#31515 = AXIS2_PLACEMENT_3D ( 'NONE', #3286, #10970, #13455 ) ;
#31516 = DIRECTION ( 'NONE',  ( -0.000000000000000000, 0.8191520442889909104, 0.5735764363510474917 ) ) ;
#31518 = ORIENTED_EDGE ( 'NONE', *, *, #20839, .T. ) ;
#31517 = CARTESIAN_POINT ( 'NONE',  ( 84.86779539662992988, -2.484919561747313210, -1.169950239651971646 ) ) ;
#31519 = PLANE ( 'NONE',  #26309 ) ;
#31520 = CARTESIAN_POINT ( 'NONE',  ( 5.377543748152548098, -2.789499415801756586E-14, 8.014274990069656823 ) ) ;
#31521 = EDGE_CURVE ( 'NONE', #16776, #10415, #31673, .T. ) ;
#31522 = CARTESIAN_POINT ( 'NONE',  ( 26.29336354336543735, 19.59588486419533382, 5.471072653610983494 ) ) ;
#31523 = DIRECTION ( 'NONE',  ( -1.000000000000000000, 0.000000000000000000, 0.000000000000000000 ) ) ;
#31524 = CARTESIAN_POINT ( 'NONE',  ( 108.0618741790777193, -18.96033490297902091, 4.492441070042681339 ) ) ;
#31525 = DIRECTION ( 'NONE',  ( -2.219124775575043125E-17, -0.2588190451025343397, 0.9659258262890646485 ) ) ;
#31526 = CARTESIAN_POINT ( 'NONE',  ( -31.80940264096945924, 1.734723475976807094E-15, 0.000000000000000000 ) ) ;
#31527 = CARTESIAN_POINT ( 'NONE',  ( 79.92595492699416582, 21.43178168691304819, 1.508259000770581393 ) ) ;
#31528 = FACE_OUTER_BOUND ( 'NONE', #32434, .T. ) ;
#31529 = AXIS2_PLACEMENT_3D ( 'NONE', #11851, #22062, #32281 ) ;
#31530 = AXIS2_PLACEMENT_3D ( 'NONE', #1016, #23582, #8377 ) ;
#31531 = CARTESIAN_POINT ( 'NONE',  ( 32.99878091140236336, 0.000000000000000000, -3.000000000000002665 ) ) ;
#31532 = DIRECTION ( 'NONE',  ( 0.000000000000000000, 0.000000000000000000, -1.000000000000000000 ) ) ;
#31533 = CARTESIAN_POINT ( 'NONE',  ( 22.86000000273118715, -1.942864903642428587, -1.573300977624592756 ) ) ;
#31534 = CARTESIAN_POINT ( 'NONE',  ( 22.04243029792654340, -21.80478118307064861, 1.499729010651354777 ) ) ;
#31535 = CIRCLE ( 'NONE', #25658, 6.249000000000000554 ) ;
#31536 = B_SPLINE_CURVE_WITH_KNOTS ( 'NONE', 3,
 ( #30477, #14594, #9910, #7391, #27784, #19616, #22285, #15079, #30170, #17279 ),
 .UNSPECIFIED., .F., .F.,
 ( 4, 2, 2, 2, 4 ),
 ( 1.968338519003008803E-07, 0.0005467926395225666770, 0.001093388445193233015, 0.001639984250863899245, 0.002186580056534565691 ),
 .UNSPECIFIED. ) ;
#31537 = DIRECTION ( 'NONE',  ( 0.000000000000000000, 1.000000000000000000, 0.000000000000000000 ) ) ;
#31538 = CARTESIAN_POINT ( 'NONE',  ( -2.062550801365593323, -0.3701630799359326152, 3.521866450007987037 ) ) ;
#31539 = ORIENTED_EDGE ( 'NONE', *, *, #32319, .T. ) ;
#31540 = CARTESIAN_POINT ( 'NONE',  ( -7.400050800000000706, 1.887961173149511618, 2.331437884370912705 ) ) ;
#31541 = VECTOR ( 'NONE', #26465, 1000.000000000000000 ) ;
#31542 = CARTESIAN_POINT ( 'NONE',  ( 9.578960313758919654, 17.92714876365089793, -5.396302277755719246 ) ) ;
#31543 = CARTESIAN_POINT ( 'NONE',  ( 0.000000000000000000, -9.620177616657944242, -5.227991826304196010 ) ) ;
#31544 = CARTESIAN_POINT ( 'NONE',  ( 9.283830569144180700, -0.1241467202002616427, 1.500000000000000000 ) ) ;
#31545 = ORIENTED_EDGE ( 'NONE', *, *, #22732, .T. ) ;
#31546 = FACE_OUTER_BOUND ( 'NONE', #23515, .T. ) ;
#31547 = EDGE_LOOP ( 'NONE', ( #21208, #23995, #20612, #26921 ) ) ;
#31548 = CARTESIAN_POINT ( 'NONE',  ( 3.708020185722930240, -12.03545600470719279, 1.500000000000000666 ) ) ;
#31549 = CALENDAR_DATE ( 2026, 6, 10 ) ;
#31550 = CIRCLE ( 'NONE', #17120, 5.000000000000001776 ) ;
#31551 = CARTESIAN_POINT ( 'NONE',  ( 54.95446108372983929, -5.684089628153301099, 4.275175838002291506 ) ) ;
#31552 = EDGE_CURVE ( 'NONE', #23417, #20990, #23446, .T. ) ;
#31553 = EDGE_CURVE ( 'NONE', #469, #16936, #17247, .T. ) ;
#31554 = VECTOR ( 'NONE', #16343, 1000.000000000000114 ) ;
#31555 = CIRCLE ( 'NONE', #5404, 302.4235430809786749 ) ;
#31556 = PLANE ( 'NONE',  #21895 ) ;
#31557 = AXIS2_PLACEMENT_3D ( 'NONE', #10507, #2508, #12343 ) ;
#31558 = CARTESIAN_POINT ( 'NONE',  ( 24.16865442153064691, -17.43004354390603083, -1.504494863253570403 ) ) ;
#31559 = CARTESIAN_POINT ( 'NONE',  ( 2.976845824368062665, 4.933977349953576841, 7.725179967474386622 ) ) ;
#31560 = EDGE_CURVE ( 'NONE', #9323, #8122, #13246, .T. ) ;
#31561 = ORIENTED_EDGE ( 'NONE', *, *, #11058, .T. ) ;
#31562 = CARTESIAN_POINT ( 'NONE',  ( 4.285194126261599773E-30, 4.979297819079224069E-14, -4.753758587302147731 ) ) ;
#31563 = CARTESIAN_POINT ( 'NONE',  ( 26.08945412691624099, 19.05746434167065928, -1.050000000000000044 ) ) ;
#31564 = DIRECTION ( 'NONE',  ( -0.04852105321274532979, 0.4695180821586686926, 0.8815886103626632275 ) ) ;
#31565 = CIRCLE ( 'NONE', #17133, 2.999999999999999112 ) ;
#31567 = ORIENTED_EDGE ( 'NONE', *, *, #11244, .F. ) ;
#31566 = CARTESIAN_POINT ( 'NONE',  ( -10.00000000000000000, 0.000000000000000000, 0.000000000000000000 ) ) ;
#31568 = CARTESIAN_POINT ( 'NONE',  ( -3.762550801365593500, 2.228590825266444142, 2.752080473201636845 ) ) ;
#31569 = LINE ( 'NONE', #23719, #31554 ) ;
#31570 = LINE ( 'NONE', #5521, #8608 ) ;
#31571 = VERTEX_POINT ( 'NONE', #10927 ) ;
#31572 = CARTESIAN_POINT ( 'NONE',  ( 108.0291781248179177, -18.48951985539285658, 4.325670280512381005 ) ) ;
#31573 = CARTESIAN_POINT ( 'NONE',  ( 0.6728001045953904136, -3.357496170320726225, 8.512517952474004446 ) ) ;
#31574 = CARTESIAN_POINT ( 'NONE',  ( 10.00000000000000000, 4.616489984850557171, -1.946309384392544528 ) ) ;
#31575 = CARTESIAN_POINT ( 'NONE',  ( 3.551765900376501861, -15.35947713381495383, 5.485967528433935314 ) ) ;
#31576 = VECTOR ( 'NONE', #31870, 1000.000000000000000 ) ;
#31577 = DIRECTION ( 'NONE',  ( 1.000000000000000000, -0.000000000000000000, -0.000000000000000000 ) ) ;
#31578 = ORIENTED_EDGE ( 'NONE', *, *, #32659, .T. ) ;
#31579 = CIRCLE ( 'NONE', #5937, 4.000000000000001776 ) ;
#31580 = AXIS2_PLACEMENT_3D ( 'NONE', #17167, #27378, #20837 ) ;
#31581 = LINE ( 'NONE', #16197, #19393 ) ;
#31582 = CARTESIAN_POINT ( 'NONE',  ( -58.35512979123338084, -4.055258467324091676, 5.700934511681459149 ) ) ;
#31583 = AXIS2_PLACEMENT_3D ( 'NONE', #3578, #3425, #9044 ) ;
#31584 =( BOUNDED_SURFACE ( )  B_SPLINE_SURFACE ( 3, 2, ( 
 ( #16831, #26686, #13798 ),
 ( #31740, #21686, #3802 ),
 ( #21531, #23859, #6638 ),
 ( #3984, #13970, #24190 ),
 ( #9303, #8817, #29206 ),
 ( #24497, #11490, #8958 ),
 ( #22017, #13655, #21348 ),
 ( #6452, #16657, #14153 ),
 ( #31558, #24351, #966 ),
 ( #32049, #27031, #4132 ),
 ( #1616, #11147, #11810 ),
 ( #19519, #29868, #25178 ) ),
 .UNSPECIFIED., .F., .F., .F. ) 
 B_SPLINE_SURFACE_WITH_KNOTS ( ( 4, 2, 2, 2, 2, 4 ),
 ( 3, 3 ),
 ( 0.02103335055024949107, 0.02276256425196081928, 0.02362717110281648339, 0.02405947452824431371, 0.02427562624095823060, 0.02449177795367214749 ),
 ( 0.000000000000000000, 1.000000000000000000 ),
 .UNSPECIFIED. ) 
 GEOMETRIC_REPRESENTATION_ITEM ( )  RATIONAL_B_SPLINE_SURFACE ( (
 ( 1.000000000000000000, 0.8477574071936589961, 1.000000000000000000),
 ( 1.000000000000000000, 0.8716452794063324072, 1.000000000000000000),
 ( 1.000000000000000000, 0.8956763213344164365, 1.000000000000000000),
 ( 1.000000000000000000, 0.9319482906208321760, 1.000000000000000000),
 ( 1.000000000000000000, 0.9440737053932664047, 1.000000000000000000),
 ( 1.000000000000000000, 0.9620964665818899642, 1.000000000000000000),
 ( 1.000000000000000000, 0.9681025352174974508, 1.000000000000000000),
 ( 1.000000000000000000, 0.9768916256376188878, 1.000000000000000000),
 ( 1.000000000000000000, 0.9797842808059200603, 1.000000000000000000),
 ( 1.000000000000000000, 0.9854258872291279392, 1.000000000000000000),
 ( 1.000000000000000000, 0.9882007853475626158, 1.000000000000000000),
 ( 1.000000000000000000, 0.9906937806494816590, 1.000000000000000000) ) ) 
 REPRESENTATION_ITEM ( '' )  SURFACE ( )  );
#31585 = CARTESIAN_POINT ( 'NONE',  ( -4.237550801365593145, -1.088641768524163611, -3.675193018007245627 ) ) ;
#31586 = CARTESIAN_POINT ( 'NONE',  ( 107.9095081641845582, -17.54872683406297540, -4.428332375768106566 ) ) ;
#31587 = CARTESIAN_POINT ( 'NONE',  ( -2.162942409646512854, 4.884725290497410777E-15, -2.999999999999999556 ) ) ;
#31588 = AXIS2_PLACEMENT_3D ( 'NONE', #26959, #1223, #31816 ) ;
#31589 = VERTEX_POINT ( 'NONE', #10743 ) ;
#31590 = CARTESIAN_POINT ( 'NONE',  ( 2.274274201625327230, -9.680994141368730155, -5.222868219166962866 ) ) ;
#31591 = VECTOR ( 'NONE', #22653, 1000.000000000000000 ) ;
#31592 = EDGE_CURVE ( 'NONE', #28679, #10493, #15026, .T. ) ;
#31593 = EDGE_LOOP ( 'NONE', ( #6760, #27849, #6157, #3607, #3600 ) ) ;
#31594 = CALENDAR_DATE ( 2026, 6, 10 ) ;
#31595 = CARTESIAN_POINT ( 'NONE',  ( 28.66415240725487479, -6.763317863709993993, 3.996604665448017624 ) ) ;
#31596 = CARTESIAN_POINT ( 'NONE',  ( 7.778677572338311030, -9.608974357934672028, -1.000000000000000222 ) ) ;
#31597 = ORIENTED_EDGE ( 'NONE', *, *, #27124, .T. ) ;
#31598 = CARTESIAN_POINT ( 'NONE',  ( 7.249760686538667009, -7.906491560603691404, 3.748318449932265484 ) ) ;
#31599 = ORIENTED_EDGE ( 'NONE', *, *, #29972, .T. ) ;
#31600 = VECTOR ( 'NONE', #9402, 1000.000000000000000 ) ;
#31601 = ORIENTED_EDGE ( 'NONE', *, *, #17958, .T. ) ;
#31602 = LINE ( 'NONE', #1173, #10728 ) ;
#31603 = CARTESIAN_POINT ( 'NONE',  ( -3.812550801365593323, 3.368539882008727115, 1.828967928396027176 ) ) ;
#31604 = AXIS2_PLACEMENT_3D ( 'NONE', #4987, #12995, #28200 ) ;
#31605 = CARTESIAN_POINT ( 'NONE',  ( 26.23500000000000298, 0.2613211581691317065, 2.486304738420681559 ) ) ;
#31606 = CIRCLE ( 'NONE', #29984, 10.99999999999999822 ) ;
#31607 = DIRECTION ( 'NONE',  ( 1.000000000000000000, -0.000000000000000000, 0.000000000000000000 ) ) ;
#31609 = ORIENTED_EDGE ( 'NONE', *, *, #28300, .F. ) ;
#31608 = DIRECTION ( 'NONE',  ( 1.000000000000000000, 0.000000000000000000, 0.000000000000000000 ) ) ;
#31610 = CARTESIAN_POINT ( 'NONE',  ( -5.637550801365595277, 3.675193018007247403, -1.088641768524161391 ) ) ;
#31611 = AXIS2_PLACEMENT_3D ( 'NONE', #16717, #3381, #21098 ) ;
#31612 = CARTESIAN_POINT ( 'NONE',  ( 16.87315779114032566, 12.21951710881648090, 1.499999999999999112 ) ) ;
#31613 = CARTESIAN_POINT ( 'NONE',  ( 7.064632879756604034, 2.210816291636326980, -8.466096581343460770 ) ) ;
#31614 = CARTESIAN_POINT ( 'NONE',  ( 22.23500000136559862, -1.570731468192933633, -2.892927487894330074 ) ) ;
#31615 = AXIS2_PLACEMENT_3D ( 'NONE', #9700, #11552, #9201 ) ;
#31617 = ORIENTED_EDGE ( 'NONE', *, *, #13464, .T. ) ;
#31616 = CARTESIAN_POINT ( 'NONE',  ( 0.7632845268398871230, -4.729683950898817102, -7.360373001730970977 ) ) ;
#31618 = AXIS2_PLACEMENT_3D ( 'NONE', #22832, #33035, #5278 ) ;
#31619 = AXIS2_PLACEMENT_3D ( 'NONE', #18452, #28646, #1043 ) ;
#31620 = CARTESIAN_POINT ( 'NONE',  ( 47.75999538435724645, -8.435302152663906483, 0.07017451552781736601 ) ) ;
#31621 = CARTESIAN_POINT ( 'NONE',  ( 22.92250000273118715, -1.291182301015472378, -2.378061970571982098 ) ) ;
#31622 = EDGE_CURVE ( 'NONE', #22141, #16462, #2868, .T. ) ;
#31623 = DIRECTION ( 'NONE',  ( 1.000000000000000000, 0.000000000000000000, 0.000000000000000000 ) ) ;
#31624 = CARTESIAN_POINT ( 'NONE',  ( -4.524729257728259846, -7.612611013041808761, -1.499999999999999556 ) ) ;
#31625 = VECTOR ( 'NONE', #11707, 1000.000000000000000 ) ;
#31626 = CARTESIAN_POINT ( 'NONE',  ( 0.1574692421723846159, -7.165523657697560722, -7.841623826006603792 ) ) ;
#31627 = ADVANCED_FACE ( 'NONE', ( #2585 ), #23147, .T. ) ;
#31628 = VECTOR ( 'NONE', #17318, 1000.000000000000000 ) ;
#31629 = VECTOR ( 'NONE', #2720, 1000.000000000000114 ) ;
#31630 = DIRECTION ( 'NONE',  ( -0.000000000000000000, 0.000000000000000000, 1.000000000000000000 ) ) ;
#31631 = CARTESIAN_POINT ( 'NONE',  ( -6.437550801365593323, 3.675193018007247403, -1.088641768524161391 ) ) ;
#31632 = ORIENTED_EDGE ( 'NONE', *, *, #4240, .T. ) ;
#31633 = CIRCLE ( 'NONE', #1204, 2.999999999999999112 ) ;
#31634 = AXIS2_PLACEMENT_3D ( 'NONE', #26666, #24649, #17126 ) ;
#31635 = TOROIDAL_SURFACE ( 'NONE', #8064, 5.587650971692158741, 0.4500000000000000111 ) ;
#31636 = CARTESIAN_POINT ( 'NONE',  ( 18.70218739253826357, -21.34730519116122949, 1.543632415228167076 ) ) ;
#31637 = VECTOR ( 'NONE', #20110, 999.9999999999998863 ) ;
#31638 = EDGE_CURVE ( 'NONE', #30501, #26497, #7106, .T. ) ;
#31639 = CARTESIAN_POINT ( 'NONE',  ( 3.499999999999999556, 1.418488851014487073, -6.085876303339362359 ) ) ;
#31642 = CARTESIAN_POINT ( 'NONE',  ( 0.000000000000000000, 7.593217523260693547, -7.958834565716684573 ) ) ;
#31641 = DIRECTION ( 'NONE',  ( 1.000000000000000000, 0.000000000000000000, 0.000000000000000000 ) ) ;
#31640 = AXIS2_PLACEMENT_3D ( 'NONE', #32807, #5352, #4855 ) ;
#31643 = EDGE_CURVE ( 'NONE', #7869, #23146, #6488, .T. ) ;
#31644 = VERTEX_POINT ( 'NONE', #14228 ) ;
#31645 = CIRCLE ( 'NONE', #19379, 10.00000000000000355 ) ;
#31646 = DIRECTION ( 'NONE',  ( 0.000000000000000000, 0.4067366430758009299, -0.9135454576426005335 ) ) ;
#31647 = VERTEX_POINT ( 'NONE', #26306 ) ;
#31648 = CARTESIAN_POINT ( 'NONE',  ( -14.47914180357919989, -27.93932300454937590, -4.314460059828594041 ) ) ;
#31650 = ORIENTED_EDGE ( 'NONE', *, *, #28299, .T. ) ;
#31649 = CARTESIAN_POINT ( 'NONE',  ( 24.39659513448239991, -17.41072360183627055, 1.416990234759656575 ) ) ;
#31651 = ORIENTED_EDGE ( 'NONE', *, *, #21227, .T. ) ;
#31652 = DIRECTION ( 'NONE',  ( 0.000000000000000000, 1.000000000000000000, 0.000000000000000000 ) ) ;
#31653 = EDGE_CURVE ( 'NONE', #27732, #32541, #8802, .T. ) ;
#31654 = DIRECTION ( 'NONE',  ( 0.000000000000000000, 0.000000000000000000, -1.000000000000000000 ) ) ;
#31656 = VERTEX_POINT ( 'NONE', #6558 ) ;
#31655 = CARTESIAN_POINT ( 'NONE',  ( -45.71000000000000085, -10.96999999999998643, 5.700000000000000178 ) ) ;
#31657 = VECTOR ( 'NONE', #7160, 1000.000000000000000 ) ;
#31658 = PLANE ( 'NONE',  #30045 ) ;
#31659 = CARTESIAN_POINT ( 'NONE',  ( -7.000050800000001239, 4.286263797015736102E-16, -3.499999999999999556 ) ) ;
#31660 = AXIS2_PLACEMENT_3D ( 'NONE', #18438, #6353, #1200 ) ;
#31661 = PLANE ( 'NONE',  #17153 ) ;
#31662 = CIRCLE ( 'NONE', #9760, 6.249000000000000554 ) ;
#31663 = CARTESIAN_POINT ( 'NONE',  ( 9.360049168479326553, -11.53021799169701112, -1.500000000000000000 ) ) ;
#31664 = CARTESIAN_POINT ( 'NONE',  ( 107.9203180492143588, -16.92196184768069145, -2.556177043345751798 ) ) ;
#31665 = CYLINDRICAL_SURFACE ( 'NONE', #26864, 5.010000000000000675 ) ;
#31666 = AXIS2_PLACEMENT_3D ( 'NONE', #18582, #13559, #26110 ) ;
#31668 = EDGE_CURVE ( 'NONE', #2488, #9130, #9687, .T. ) ;
#31667 = CIRCLE ( 'NONE', #18292, 8.750000000000000000 ) ;
#31669 =( BOUNDED_SURFACE ( )  B_SPLINE_SURFACE ( 3, 2, ( 
 ( #26919, #31783, #6028 ),
 ( #16712, #16526, #21093 ),
 ( #16222, #3376, #11191 ),
 ( #23751, #13844, #3854 ),
 ( #16030, #8367, #3686 ),
 ( #8854, #21727, #10885 ),
 ( #695, #11042, #24239 ),
 ( #21241, #31439, #18718 ),
 ( #16374, #28923, #26441 ),
 ( #13698, #21398, #8695 ),
 ( #24052, #4342, #14844 ),
 ( #32440, #2008, #30112 ),
 ( #14698, #2161, #30265 ),
 ( #22230, #24896, #12035 ),
 ( #32779, #29601, #22381 ),
 ( #7337, #9173, #9857 ),
 ( #14191, #32597, #29915 ),
 ( #19559, #6684, #16873 ),
 ( #20069, #24389, #6836 ),
 ( #1858, #9501, #22072 ),
 ( #17211, #4171, #32098 ),
 ( #1506, #14522, #24544 ),
 ( #9670, #12345, #17527 ),
 ( #11684, #19403, #27227 ),
 ( #1668, #27069, #17381 ),
 ( #19716, #12181, #7188 ),
 ( #19898, #22565, #4024 ),
 ( #6998, #27575, #27417 ),
 ( #21882, #14338, #4674 ),
 ( #11863, #32288, #9349 ),
 ( #29756, #25043, #4523 ),
 ( #17021, #24733, #170 ),
 ( #30603, #2856, #12831 ),
 ( #25726, #33086, #2511 ),
 ( #15010, #4829, #13025 ),
 ( #25232, #20384, #27908 ),
 ( #28226, #10509, #7996 ),
 ( #2352, #12527, #5331 ) ),
 .UNSPECIFIED., .F., .F., .F. ) 
 B_SPLINE_SURFACE_WITH_KNOTS ( ( 4, 2, 2, 2, 2, 2, 2, 2, 2, 2, 2, 2, 2, 2, 2, 2, 2, 2, 4 ),
 ( 3, 3 ),
 ( 0.000000000000000000, 0.001918043520347785828, 0.003836087040695571656, 0.004795108800869464678, 0.005754130561043357267, 0.006713152321217250723, 0.007192663201304197451, 0.007672174081391143312, 0.008631195841565035901, 0.009590217601738929357, 0.01150826112208671453, 0.01246728288226060799, 0.01342630464243450145, 0.01534434816278228662, 0.01726239168313007180, 0.01918043520347785871, 0.02301652224417342907, 0.02685260928486900289, 0.03068869632556457325 ),
 ( 0.000000000000000000, 1.000000000000000000 ),
 .UNSPECIFIED. ) 
 GEOMETRIC_REPRESENTATION_ITEM ( )  RATIONAL_B_SPLINE_SURFACE ( (
 ( 1.000000000000000000, 0.8449619147701439292, 1.000000000000000000),
 ( 1.000000000000000000, 0.8445678029926584340, 1.000000000000000000),
 ( 1.000000000000000000, 0.8440734858009981689, 1.000000000000000000),
 ( 1.000000000000000000, 0.8426715424874036131, 1.000000000000000000),
 ( 1.000000000000000000, 0.8417777985993892820, 1.000000000000000000),
 ( 1.000000000000000000, 0.8396981493403768981, 1.000000000000000000),
 ( 1.000000000000000000, 0.8389573580692519794, 1.000000000000000000),
 ( 1.000000000000000000, 0.8374408369630492732, 1.000000000000000000),
 ( 1.000000000000000000, 0.8366690632723572385, 1.000000000000000000),
 ( 1.000000000000000000, 0.8350101717998674733, 1.000000000000000000),
 ( 1.000000000000000000, 0.8340755910242153570, 1.000000000000000000),
 ( 1.000000000000000000, 0.8336678922694548133, 1.000000000000000000),
 ( 1.000000000000000000, 0.8336623316996139010, 1.000000000000000000),
 ( 1.000000000000000000, 0.8338837348179357623, 1.000000000000000000),
 ( 1.000000000000000000, 0.8341121628413028510, 1.000000000000000000),
 ( 1.000000000000000000, 0.8349642705193365266, 1.000000000000000000),
 ( 1.000000000000000000, 0.8357234841175039675, 1.000000000000000000),
 ( 1.000000000000000000, 0.8375342318403898867, 1.000000000000000000),
 ( 1.000000000000000000, 0.8383883957943909504, 1.000000000000000000),
 ( 1.000000000000000000, 0.8406684190711074534, 1.000000000000000000),
 ( 1.000000000000000000, 0.8419347305613049670, 1.000000000000000000),
 ( 1.000000000000000000, 0.8434083992945078379, 1.000000000000000000),
 ( 1.000000000000000000, 0.8438015669660346996, 1.000000000000000000),
 ( 1.000000000000000000, 0.8444527818707109335, 1.000000000000000000),
 ( 1.000000000000000000, 0.8447125394710991442, 1.000000000000000000),
 ( 1.000000000000000000, 0.8453649836267845830, 1.000000000000000000),
 ( 1.000000000000000000, 0.8456341134025172623, 1.000000000000000000),
 ( 1.000000000000000000, 0.8460541031445641957, 1.000000000000000000),
 ( 1.000000000000000000, 0.8462025651636095880, 1.000000000000000000),
 ( 1.000000000000000000, 0.8464941699322370283, 1.000000000000000000),
 ( 1.000000000000000000, 0.8466725352208778199, 1.000000000000000000),
 ( 1.000000000000000000, 0.8470349366253309142, 1.000000000000000000),
 ( 1.000000000000000000, 0.8471950700188056738, 1.000000000000000000),
 ( 1.000000000000000000, 0.8474407502799835568, 1.000000000000000000),
 ( 1.000000000000000000, 0.8475244277276142713, 1.000000000000000000),
 ( 1.000000000000000000, 0.8476586531197746188, 1.000000000000000000),
 ( 1.000000000000000000, 0.8477086645732269110, 1.000000000000000000),
 ( 1.000000000000000000, 0.8477574071928573041, 1.000000000000000000) ) ) 
 REPRESENTATION_ITEM ( '' )  SURFACE ( )  );
#31670 = AXIS2_PLACEMENT_3D ( 'NONE', #2890, #12705, #13055 ) ;
#31671 = CARTESIAN_POINT ( 'NONE',  ( 4.749760686538667009, 2.741043480755029016, -7.530955069117485579 ) ) ;
#31672 = DIRECTION ( 'NONE',  ( 1.000000000000000000, 0.000000000000000000, 0.000000000000000000 ) ) ;
#31673 = CIRCLE ( 'NONE', #11297, 8.750000000000000000 ) ;
#31674 = CARTESIAN_POINT ( 'NONE',  ( 6.524595395369781059, 8.328507089302179978, 2.369138865965855878 ) ) ;
#31675 = CYLINDRICAL_SURFACE ( 'NONE', #4931, 3.000000000000000444 ) ;
#31676 = VERTEX_POINT ( 'NONE', #11233 ) ;
#31677 = CARTESIAN_POINT ( 'NONE',  ( 10.00000000000000000, -1.625881193364728805, 4.467071865485467086 ) ) ;
#31678 = B_SPLINE_CURVE_WITH_KNOTS ( 'NONE', 3,
 ( #13551, #5713, #16039, #26102, #13706, #20923, #21585, #18428, #871, #21249 ),
 .UNSPECIFIED., .F., .F.,
 ( 4, 2, 2, 2, 4 ),
 ( -0.0002335416784056200705, 0.0001933787568668222175, 0.0006202991921392645054, 0.001474140062684159598, 0.003181821803773939375 ),
 .UNSPECIFIED. ) ;
#31679 = CARTESIAN_POINT ( 'NONE',  ( 33.81874022276151237, 20.00000000000000000, -1.977928362984232802 ) ) ;
#31680 = DIRECTION ( 'NONE',  ( 0.000000000000000000, 1.000000000000000000, 0.000000000000000000 ) ) ;
#31681 = ORIENTED_EDGE ( 'NONE', *, *, #11617, .T. ) ;
#31682 = CIRCLE ( 'NONE', #23138, 4.000000000000001776 ) ;
#31683 = DIRECTION ( 'NONE',  ( 0.000000000000000000, 0.000000000000000000, -1.000000000000000000 ) ) ;
#31684 = EDGE_CURVE ( 'NONE', #5744, #9758, #25180, .T. ) ;
#31685 = CARTESIAN_POINT ( 'NONE',  ( 21.20754276729287469, -21.72113672149310304, 1.466027919133091384 ) ) ;
#31687 = ORIENTED_EDGE ( 'NONE', *, *, #22874, .F. ) ;
#31686 = AXIS2_PLACEMENT_3D ( 'NONE', #9603, #19825, #30032 ) ;
#31688 = CARTESIAN_POINT ( 'NONE',  ( 17.32050807568873552, 10.00000000000002309, -1.491740999229417941 ) ) ;
#31689 = EDGE_CURVE ( 'NONE', #3605, #8263, #91, .T. ) ;
#31690 = ORIENTED_EDGE ( 'NONE', *, *, #9034, .F. ) ;
#31691 = CIRCLE ( 'NONE', #2883, 5.010000000000000675 ) ;
#31692 = CIRCLE ( 'NONE', #11925, 4.000000000000001776 ) ;
#31693 = EDGE_LOOP ( 'NONE', ( #30448, #27918, #8257, #18555, #6786 ) ) ;
#31694 = CARTESIAN_POINT ( 'NONE',  ( 5.612974259723589654, 2.996912441296280427, -7.650268724902028694 ) ) ;
#31696 = ORIENTED_EDGE ( 'NONE', *, *, #1497, .F. ) ;
#31695 = CARTESIAN_POINT ( 'NONE',  ( 84.41210159610484709, -2.963446145442715451, -2.184954676722655087 ) ) ;
#31697 = EDGE_LOOP ( 'NONE', ( #2431, #10117, #23176, #15917 ) ) ;
#31698 = CARTESIAN_POINT ( 'NONE',  ( 25.67250000136559507, 2.363507492473148286, 1.913930629741525058 ) ) ;
#31699 = CC_DESIGN_APPROVAL ( #5764, ( #6052 ) ) ;
#31700 = ORIENTED_EDGE ( 'NONE', *, *, #23362, .T. ) ;
#31701 = CARTESIAN_POINT ( 'NONE',  ( -2.386718424894567203, -9.330009425478154483, 4.522129901861158707 ) ) ;
#31702 = CARTESIAN_POINT ( 'NONE',  ( 0.08034252392815226240, 2.072171912279953343, -10.58792409793259992 ) ) ;
#31704 = ORIENTED_EDGE ( 'NONE', *, *, #30286, .T. ) ;
#31703 = PLANE ( 'NONE',  #27749 ) ;
#31705 = CARTESIAN_POINT ( 'NONE',  ( 21.55656763645044904, -0.8852964313267484009, 2.499999999999997780 ) ) ;
#31706 = CARTESIAN_POINT ( 'NONE',  ( 0.5664946525207626982, 9.241976615239526183, 2.300561732649596181 ) ) ;
#31707 = CARTESIAN_POINT ( 'NONE',  ( -56.77654246901312263, 0.4654628299899072896, 1.959872961020660664 ) ) ;
#31708 = FACE_OUTER_BOUND ( 'NONE', #23403, .T. ) ;
#31709 = CARTESIAN_POINT ( 'NONE',  ( 108.0291954987227712, -18.48977003530059804, 4.324986740352072090 ) ) ;
#31710 = EDGE_CURVE ( 'NONE', #24312, #22183, #13219, .T. ) ;
#31711 = PRODUCT_DEFINITION ( 'UNKNOWN', '', #7706, #16583 ) ;
#31712 = AXIS2_PLACEMENT_3D ( 'NONE', #3729, #26624, #1401 ) ;
#31713 = CARTESIAN_POINT ( 'NONE',  ( -0.7739934281325310250, -8.972773999336027373, -4.522129901861164925 ) ) ;
#31714 = DIRECTION ( 'NONE',  ( 0.000000000000000000, 0.000000000000000000, -1.000000000000000000 ) ) ;
#31715 = FACE_OUTER_BOUND ( 'NONE', #21482, .T. ) ;
#31716 = AXIS2_PLACEMENT_3D ( 'NONE', #7079, #2069, #17438 ) ;
#31717 = AXIS2_PLACEMENT_3D ( 'NONE', #20507, #18478, #23174 ) ;
#31718 = CARTESIAN_POINT ( 'NONE',  ( -50.60000000000000142, -10.96966150227468972, 6.999999999999999112 ) ) ;
#31719 = DIRECTION ( 'NONE',  ( 0.000000000000000000, 0.000000000000000000, 1.000000000000000000 ) ) ;
#31720 = CARTESIAN_POINT ( 'NONE',  ( 107.6996442589673819, 19.35565155597529596, -4.612695725900422872 ) ) ;
#31721 = CARTESIAN_POINT ( 'NONE',  ( 23.99290772595112742, -0.1310194482076044442, -2.499999999999998668 ) ) ;
#31722 = APPROVAL_PERSON_ORGANIZATION ( #1495, #12877, #32277 ) ;
#31723 = FACE_OUTER_BOUND ( 'NONE', #7800, .T. ) ;
#31724 = CARTESIAN_POINT ( 'NONE',  ( -4.912550801365593856, -1.088641768524163389, -3.675193018007246071 ) ) ;
#31725 = ORIENTED_EDGE ( 'NONE', *, *, #18735, .F. ) ;
#31726 = EDGE_CURVE ( 'NONE', #502, #1423, #6224, .T. ) ;
#31727 = CARTESIAN_POINT ( 'NONE',  ( -5.400050800000000706, -1.887961173149512062, -2.331437884370912261 ) ) ;
#31728 = CARTESIAN_POINT ( 'NONE',  ( 13.41780342409107973, 19.07609913100965571, -4.612695725900421984 ) ) ;
#31729 = CARTESIAN_POINT ( 'NONE',  ( -5.000050800000001239, 1.887961173149511618, 2.331437884370912705 ) ) ;
#31730 = CARTESIAN_POINT ( 'NONE',  ( 7.166310627377590059, -7.340520188496220122, 1.499999999999999112 ) ) ;
#31731 = ORIENTED_EDGE ( 'NONE', *, *, #20802, .T. ) ;
#31732 = CARTESIAN_POINT ( 'NONE',  ( 8.045354371110279956, -1.465502149859512881, -1.500000000000000000 ) ) ;
#31733 = CIRCLE ( 'NONE', #13037, 8.500000000000000000 ) ;
#31734 = ORIENTED_EDGE ( 'NONE', *, *, #16934, .T. ) ;
#31735 = CARTESIAN_POINT ( 'NONE',  ( 0.7549893952831980837, -8.141048257043983938, 1.499999999999999556 ) ) ;
#31736 = COORDINATED_UNIVERSAL_TIME_OFFSET ( 0, 0, .AHEAD. ) ;
#31737 = CARTESIAN_POINT ( 'NONE',  ( 85.00835009345571791, -4.756612885545567160, 4.312042181580753031 ) ) ;
#31738 = B_SPLINE_CURVE_WITH_KNOTS ( 'NONE', 3,
 ( #3514, #11503, #13670, #29571, #21366, #31572 ),
 .UNSPECIFIED., .F., .F.,
 ( 4, 2, 4 ),
 ( 4.036569264948304377E-14, 0.0003910668831145792121, 0.0007821337661887927100 ),
 .UNSPECIFIED. ) ;
#31739 = CARTESIAN_POINT ( 'NONE',  ( 11.61992484759235644, 3.867395925924771660, -1.050000000000000044 ) ) ;
#31740 = CARTESIAN_POINT ( 'NONE',  ( 21.60307794872525022, -17.26039173292211970, -1.753143643193426193 ) ) ;
#31741 = DIRECTION ( 'NONE',  ( 0.1767573132311666129, 0.9842544651762059615, 0.000000000000000000 ) ) ;
#31742 = EDGE_LOOP ( 'NONE', ( #20228, #21378, #21155, #27479 ) ) ;
#31743 = LOCAL_TIME ( 16, 7, 10.00000000000000000, #10959 ) ;
#31744 = CARTESIAN_POINT ( 'NONE',  ( 9.192617927958339763, 0.08611596088385452263, 1.322472180770052352 ) ) ;
#31745 = EDGE_CURVE ( 'NONE', #12210, #31785, #15564, .T. ) ;
#31746 = DIRECTION ( 'NONE',  ( -0.1290991311227714933, -0.9916316928897268568, 0.000000000000000000 ) ) ;
#31747 = CARTESIAN_POINT ( 'NONE',  ( 7.064423637759001728, -7.953573330858861645, 3.647351267792873220 ) ) ;
#31749 = ORIENTED_EDGE ( 'NONE', *, *, #15175, .F. ) ;
#31748 = CARTESIAN_POINT ( 'NONE',  ( 25.60517990396913390, 1.170994586158331296, -2.631221474790117032 ) ) ;
#31750 = CARTESIAN_POINT ( 'NONE',  ( -3.162550801365593856, 2.752080473201636845, -2.228590825266444142 ) ) ;
#31751 = CARTESIAN_POINT ( 'NONE',  ( 0.000000000000000000, -2.834406817834963732, 8.013497238472769624 ) ) ;
#31752 = CARTESIAN_POINT ( 'NONE',  ( 3.063284526839887167, -2.223716399045513992, -8.461683424509338636 ) ) ;
#31753 = PLANE ( 'NONE',  #5984 ) ;
#31754 = AXIS2_PLACEMENT_3D ( 'NONE', #22853, #1981, #25372 ) ;
#31755 = FACE_OUTER_BOUND ( 'NONE', #14224, .T. ) ;
#31756 = CARTESIAN_POINT ( 'NONE',  ( 108.1288400433390393, -19.92462668933127290, 1.384270303710046335 ) ) ;
#31757 = CARTESIAN_POINT ( 'NONE',  ( -2.461002521556363565, -6.738986457086103776, 5.485967528433935314 ) ) ;
#31758 = ORIENTED_EDGE ( 'NONE', *, *, #9879, .T. ) ;
#31759 = EDGE_CURVE ( 'NONE', #24872, #1705, #899, .T. ) ;
#31760 = CARTESIAN_POINT ( 'NONE',  ( 24.54847674045369743, -17.37474032055271067, 1.294225383761794967 ) ) ;
#31761 = ORIENTED_EDGE ( 'NONE', *, *, #19665, .F. ) ;
#31762 = ADVANCED_FACE ( 'NONE', ( #3721 ), #9039, .F. ) ;
#31763 = CARTESIAN_POINT ( 'NONE',  ( 25.47590240457303423, -17.55751406574353979, -1.147657805880700321 ) ) ;
#31764 = DIRECTION ( 'NONE',  ( 0.000000000000000000, 0.000000000000000000, -1.000000000000000000 ) ) ;
#31765 = ADVANCED_FACE ( 'NONE', ( #11417 ), #13942, .F. ) ;
#31766 = CARTESIAN_POINT ( 'NONE',  ( -4.737550801365594033, 3.368539882008727115, 1.828967928396027176 ) ) ;
#31767 = LINE ( 'NONE', #5685, #21534 ) ;
#31768 = CARTESIAN_POINT ( 'NONE',  ( 35.27971914370861839, -7.797547734959289656, 2.184956776477424700 ) ) ;
#31769 = ORIENTED_EDGE ( 'NONE', *, *, #12479, .F. ) ;
#31770 = LINE ( 'NONE', #6321, #31129 ) ;
#31771 = ORIENTED_EDGE ( 'NONE', *, *, #8828, .F. ) ;
#31772 = APPROVAL_STATUS ( 'not_yet_approved' ) ;
#31773 = CARTESIAN_POINT ( 'NONE',  ( 102.4232908028732538, -3.999773562718685671, 3.993434327300716458 ) ) ;
#31774 = VECTOR ( 'NONE', #24749, 1000.000000000000000 ) ;
#31775 = CARTESIAN_POINT ( 'NONE',  ( -3.600050802731187716, 3.113457007523260156, -0.9222479816126439855 ) ) ;
#31776 = VERTEX_POINT ( 'NONE', #19098 ) ;
#31777 = DIRECTION ( 'NONE',  ( 0.000000000000000000, 1.000000000000000000, 0.000000000000000000 ) ) ;
#31778 = ORIENTED_EDGE ( 'NONE', *, *, #23916, .T. ) ;
#31779 = ORIENTED_EDGE ( 'NONE', *, *, #25130, .T. ) ;
#31780 = DIRECTION ( 'NONE',  ( -1.000000000000000000, -0.000000000000000000, 0.000000000000000000 ) ) ;
#31781 = CARTESIAN_POINT ( 'NONE',  ( -4.412550801365592079, -1.828967928396026732, 3.368539882008728004 ) ) ;
#31782 = CARTESIAN_POINT ( 'NONE',  ( 22.54750000000000654, -2.594547506269383685, -0.7685399846772043020 ) ) ;
#31783 = CARTESIAN_POINT ( 'NONE',  ( 2.386646147131364692, -0.3554301312245157773, -1.499999999999999112 ) ) ;
#31785 = VERTEX_POINT ( 'NONE', #29286 ) ;
#31784 = DIRECTION ( 'NONE',  ( 0.000000000000000000, 0.000000000000000000, -1.000000000000000000 ) ) ;
#31786 = CARTESIAN_POINT ( 'NONE',  ( -7.637550801365593500, -3.675193018007246071, 1.088641768524163167 ) ) ;
#31787 = DIRECTION ( 'NONE',  ( 0.000000000000000000, 0.000000000000000000, 1.000000000000000000 ) ) ;
#31788 = CARTESIAN_POINT ( 'NONE',  ( 7.452958749828057172, -19.12795340808451527, 1.499999999999999112 ) ) ;
#31789 = CARTESIAN_POINT ( 'NONE',  ( 0.000000000000000000, 0.000000000000000000, 1.500000000000000000 ) ) ;
#31791 = ORIENTED_EDGE ( 'NONE', *, *, #9823, .F. ) ;
#31790 = CARTESIAN_POINT ( 'NONE',  ( -5.175170698068149555, 0.5000000000000000000, -5.403836275575627290 ) ) ;
#31792 =( BOUNDED_SURFACE ( )  B_SPLINE_SURFACE ( 3, 1, ( 
 ( #5749, #21282 ),
 ( #25990, #11083 ),
 ( #2755, #20795 ),
 ( #8082, #7923 ) ),
 .UNSPECIFIED., .F., .F., .F. ) 
 B_SPLINE_SURFACE_WITH_KNOTS ( ( 4, 4 ),
 ( 2, 2 ),
 ( 0.000000000000000000, 1.000000000000000000 ),
 ( 0.000000000000000000, 1.000000000000000000 ),
 .UNSPECIFIED. ) 
 GEOMETRIC_REPRESENTATION_ITEM ( )  RATIONAL_B_SPLINE_SURFACE ( (
 ( 1.000000000000000000, 1.000000000000000000),
 ( 0.6539698177806696489, 0.6539698177806696489),
 ( 0.6539698177806696489, 0.6539698177806696489),
 ( 1.000000000000000000, 1.000000000000000000) ) ) 
 REPRESENTATION_ITEM ( '' )  SURFACE ( )  );
#31793 = CARTESIAN_POINT ( 'NONE',  ( 21.67250000273118715, -2.378061970571983430, 1.291182301015471712 ) ) ;
#31794 = EDGE_CURVE ( 'NONE', #15946, #28338, #6372, .T. ) ;
#31795 = ADVANCED_FACE ( 'NONE', ( #24277 ), #21926, .T. ) ;
#31796 = FACE_OUTER_BOUND ( 'NONE', #11637, .T. ) ;
#31797 = EDGE_CURVE ( 'NONE', #10158, #14757, #12389, .T. ) ;
#31798 = CARTESIAN_POINT ( 'NONE',  ( 2.440333653313245144, -4.424884217110343521, -9.715096239900912423 ) ) ;
#31799 = CARTESIAN_POINT ( 'NONE',  ( -4.174600725233243104, -9.415483487261550266, -1.500000000000000000 ) ) ;
#31800 = CARTESIAN_POINT ( 'NONE',  ( 0.000000000000000000, 0.000000000000000000, 0.000000000000000000 ) ) ;
#31801 = DIRECTION ( 'NONE',  ( -0.000000000000000000, 0.9063077870366493816, 0.4226182617407007736 ) ) ;
#31802 = CARTESIAN_POINT ( 'NONE',  ( -7.077711312404582636E-17, -0.8254815157535566605, 4.681538312723514395 ) ) ;
#31803 = ORIENTED_EDGE ( 'NONE', *, *, #5679, .F. ) ;
#31804 = DIRECTION ( 'NONE',  ( 1.000000000000000000, -8.574039729943018344E-17, -0.000000000000000000 ) ) ;
#31805 = PLANE ( 'NONE',  #11416 ) ;
#31807 = CARTESIAN_POINT ( 'NONE',  ( -31.67864539881508179, -21.93013659627822776, 1.095404497688272194 ) ) ;
#31806 = FACE_OUTER_BOUND ( 'NONE', #13446, .T. ) ;
#31808 = ORIENTED_EDGE ( 'NONE', *, *, #17071, .T. ) ;
#31809 = CARTESIAN_POINT ( 'NONE',  ( 15.84732276226623604, 14.44600775457921493, -1.050000000000000044 ) ) ;
#31810 = ORIENTED_EDGE ( 'NONE', *, *, #10780, .F. ) ;
#31811 = CARTESIAN_POINT ( 'NONE',  ( 0.000000000000000000, 0.000000000000000000, 0.000000000000000000 ) ) ;
#31813 = ORIENTED_EDGE ( 'NONE', *, *, #15628, .T. ) ;
#31812 = CARTESIAN_POINT ( 'NONE',  ( 18.86018730484229167, -4.740048064891443147, -3.999773682854171675 ) ) ;
#31814 = ORIENTED_EDGE ( 'NONE', *, *, #21436, .F. ) ;
#31815 = CARTESIAN_POINT ( 'NONE',  ( 108.0068349480237515, 18.21621961241920573, 4.414771370926588112 ) ) ;
#31816 = DIRECTION ( 'NONE',  ( 0.000000000000000000, -0.4226182617407034936, 0.9063077870366480493 ) ) ;
#31818 = ORIENTED_EDGE ( 'NONE', *, *, #27894, .T. ) ;
#31817 = CARTESIAN_POINT ( 'NONE',  ( 107.3993213344157027, -16.62991701035550562, 3.024831839633950636 ) ) ;
#31819 = CARTESIAN_POINT ( 'NONE',  ( 16.86324541396879795, 12.23239806884165581, -1.050000000000000044 ) ) ;
#31820 = CARTESIAN_POINT ( 'NONE',  ( -2.726590971468680458, 0.1614173311939631483, -1.446082916213561553 ) ) ;
#31821 = EDGE_CURVE ( 'NONE', #24347, #24965, #1186, .T. ) ;
#31822 = DIRECTION ( 'NONE',  ( 0.9816271834476639757, 0.000000000000000000, -0.1908089953765449709 ) ) ;
#31823 = CARTESIAN_POINT ( 'NONE',  ( 13.44509804308993139, -13.81913516398353536, -1.499999999999445111 ) ) ;
#31825 = VERTEX_POINT ( 'NONE', #9893 ) ;
#31824 = DIRECTION ( 'NONE',  ( 0.000000000000000000, 1.000000000000000000, 0.000000000000000000 ) ) ;
#31826 = CARTESIAN_POINT ( 'NONE',  ( 5.377543748152548986, 7.892520144992453801, -1.391664247347147443 ) ) ;
#31827 = ADVANCED_FACE ( 'NONE', ( #9387 ), #23604, .F. ) ;
#31828 = CARTESIAN_POINT ( 'NONE',  ( 2.274274201625327230, 4.762163868918412923, -9.915734732513168836 ) ) ;
#31829 = DIRECTION ( 'NONE',  ( 0.000000000000000000, 0.000000000000000000, 1.000000000000000000 ) ) ;
#31830 = ADVANCED_FACE ( 'NONE', ( #27271 ), #29507, .T. ) ;
#31831 = CARTESIAN_POINT ( 'NONE',  ( 5.885541736258995904, 8.006759975090648851, 2.519172009311959837 ) ) ;
#31832 = CARTESIAN_POINT ( 'NONE',  ( -23.54713438637983103, 11.18299864920563103, 1.403377589220444088 ) ) ;
#31833 = VERTEX_POINT ( 'NONE', #4876 ) ;
#31834 = CARTESIAN_POINT ( 'NONE',  ( 7.249760686538666121, 0.000000000000000000, 0.000000000000000000 ) ) ;
#31835 = ADVANCED_FACE ( 'NONE', ( #29958 ), #16912, .T. ) ;
#31836 = CARTESIAN_POINT ( 'NONE',  ( 107.3679615899517046, -16.17836279666641275, -2.098933649557105596 ) ) ;
#31837 = LINE ( 'NONE', #14397, #30658 ) ;
#31838 = ORIENTED_EDGE ( 'NONE', *, *, #8358, .T. ) ;
#31839 = CARTESIAN_POINT ( 'NONE',  ( 7.249760686538667009, -8.466096581343496297, 2.210816291636187536 ) ) ;
#31840 = ADVANCED_FACE ( 'NONE', ( #17416 ), #14751, .T. ) ;
#31841 = DIRECTION ( 'NONE',  ( 1.000000000000000000, 0.000000000000000000, 0.000000000000000000 ) ) ;
#31842 = ORIENTED_EDGE ( 'NONE', *, *, #16142, .F. ) ;
#31843 = CARTESIAN_POINT ( 'NONE',  ( 18.52607392133363007, -16.42885517518740457, -1.500000000000000222 ) ) ;
#31844 = ORIENTED_EDGE ( 'NONE', *, *, #18359, .T. ) ;
#31845 = ADVANCED_FACE ( 'NONE', ( #5704 ), #32975, .F. ) ;
#31846 = ORIENTED_EDGE ( 'NONE', *, *, #431, .F. ) ;
#31847 = CARTESIAN_POINT ( 'NONE',  ( 101.6022419886208610, -1.170867242066747416, 0.07017451552782490165 ) ) ;
#31848 = CONTEXT_DEPENDENT_SHAPE_REPRESENTATION ( #5214, #15099 ) ;
#31850 = ORIENTED_EDGE ( 'NONE', *, *, #10559, .T. ) ;
#31849 = CARTESIAN_POINT ( 'NONE',  ( 2.857987972556674805, -5.059832898186668260, 8.111531947321665825 ) ) ;
#31851 = ORIENTED_EDGE ( 'NONE', *, *, #3154, .F. ) ;
#31852 = CARTESIAN_POINT ( 'NONE',  ( 1.624999999999999778, -9.680994141368808314, 5.222868219166822534 ) ) ;
#31853 = EDGE_CURVE ( 'NONE', #32058, #32142, #12715, .T. ) ;
#31854 = ORIENTED_EDGE ( 'NONE', *, *, #27562, .F. ) ;
#31855 = CARTESIAN_POINT ( 'NONE',  ( 34.48223484310469900, 0.5000000000000000000, 2.482234843104950350 ) ) ;
#31856 = CARTESIAN_POINT ( 'NONE',  ( -42.85764933975779201, 24.74387538314362800, 1.500000000000000000 ) ) ;
#31858 = ORIENTED_EDGE ( 'NONE', *, *, #15298, .F. ) ;
#31857 = CARTESIAN_POINT ( 'NONE',  ( 29.34042402277836104, -3.698761498127606462, -0.4367664976603571336 ) ) ;
#31859 = DIRECTION ( 'NONE',  ( 1.000000000000000000, 0.000000000000000000, 0.000000000000000000 ) ) ;
#31860 = CARTESIAN_POINT ( 'NONE',  ( -3.222375984151269357, 0.000000000000000000, 1.000000000000000000 ) ) ;
#31861 = EDGE_CURVE ( 'NONE', #28329, #28828, #15884, .T. ) ;
#31862 = CARTESIAN_POINT ( 'NONE',  ( 101.9180142044465356, -5.717908595713207198, 0.8125824202740279389 ) ) ;
#31863 = DIRECTION ( 'NONE',  ( -0.6916610887771522664, 0.000000000000000000, -0.7222222222222217658 ) ) ;
#31864 = CARTESIAN_POINT ( 'NONE',  ( 107.5616947067672129, -18.98247576276246207, 4.525198558126774628 ) ) ;
#31865 = CARTESIAN_POINT ( 'NONE',  ( -1.528445841742497535, -6.248157669861958752, -5.485967528433937979 ) ) ;
#31866 = CARTESIAN_POINT ( 'NONE',  ( 55.02542983044661185, -8.237060396196271839, -0.4367666027069878054 ) ) ;
#31867 = CARTESIAN_POINT ( 'NONE',  ( 11.90652295052632503, 20.12228623747236256, -4.612695725900421984 ) ) ;
#31868 = EDGE_CURVE ( 'NONE', #4598, #24285, #24120, .T. ) ;
#31869 = EDGE_CURVE ( 'NONE', #11786, #22691, #10698, .T. ) ;
#31870 = DIRECTION ( 'NONE',  ( 3.469446951953478110E-15, -0.000000000000000000, -1.000000000000000000 ) ) ;
#31871 = CARTESIAN_POINT ( 'NONE',  ( 10.55147673363118876, 2.376879293651121383, -4.116875700062057497 ) ) ;
#31872 = CARTESIAN_POINT ( 'NONE',  ( 0.000000000000000000, -6.700937042937042065, -2.183447440113257976 ) ) ;
#31873 = DIRECTION ( 'NONE',  ( 0.000000000000000000, 1.000000000000000000, 0.000000000000000000 ) ) ;
#31874 = CARTESIAN_POINT ( 'NONE',  ( -3.830085165118321606E-16, -4.467071865485483961, 1.625881193364682620 ) ) ;
#31875 = EDGE_CURVE ( 'NONE', #11, #30215, #10867, .T. ) ;
#31876 = CARTESIAN_POINT ( 'NONE',  ( -4.650050802731187538, -1.887961173149512062, -2.331437884370912261 ) ) ;
#31877 = ORIENTED_EDGE ( 'NONE', *, *, #4611, .F. ) ;
#31878 = CARTESIAN_POINT ( 'NONE',  ( -7.650050800000001594, 1.549418761218566143, -2.853674364686379583 ) ) ;
#31879 = DIRECTION ( 'NONE',  ( 0.000000000000000000, 0.000000000000000000, 1.000000000000000000 ) ) ;
#31880 = CARTESIAN_POINT ( 'NONE',  ( 68.65514544479461279, -4.985459736524310514, -3.993435577422745908 ) ) ;
#31881 = CARTESIAN_POINT ( 'NONE',  ( 8.842484022064880378, 0.1108283380282882452, 1.500000000000000000 ) ) ;
#31882 = ORIENTED_EDGE ( 'NONE', *, *, #3209, .F. ) ;
#31883 = CARTESIAN_POINT ( 'NONE',  ( 8.970430173840842514, -11.86789775953536363, -1.500000000000000444 ) ) ;
#31884 = EDGE_CURVE ( 'NONE', #508, #16345, #24644, .T. ) ;
#31885 = ORIENTED_EDGE ( 'NONE', *, *, #10481, .F. ) ;
#31886 = CARTESIAN_POINT ( 'NONE',  ( 0.6154272894920587156, -5.548424207151230192, 1.500000000000000444 ) ) ;
#31887 = COORDINATED_UNIVERSAL_TIME_OFFSET ( 0, 0, .AHEAD. ) ;
#31888 = ORIENTED_EDGE ( 'NONE', *, *, #10169, .T. ) ;
#31889 = CARTESIAN_POINT ( 'NONE',  ( 28.68776846593492280, -5.841437261391057234, 4.215290389458900222 ) ) ;
#31890 = DIRECTION ( 'NONE',  ( 0.000000000000000000, 0.000000000000000000, 1.000000000000000000 ) ) ;
#31891 = CARTESIAN_POINT ( 'NONE',  ( 54.95788720338054389, -5.807879973315421829, -4.312042181581901445 ) ) ;
#31892 = CARTESIAN_POINT ( 'NONE',  ( 9.331062908042598636, 15.00000000000002132, 4.629213727441584325 ) ) ;
#31893 = B_SPLINE_CURVE_WITH_KNOTS ( 'NONE', 3,
 ( #13227, #5392, #28129, #20933, #15903, #18088, #31156, #18437, #5228, #12898, #5723, #8241, #15579, #26111 ),
 .UNSPECIFIED., .F., .F.,
 ( 4, 2, 2, 2, 2, 2, 4 ),
 ( 8.673617379884035472E-19, 0.0001249476642875234616, 0.0002498953285750460558, 0.0004997906571500799686, 0.0007496859857251137729, 0.0008746336500126335482, 0.0009995813143001532151 ),
 .UNSPECIFIED. ) ;
#31894 = ORIENTED_EDGE ( 'NONE', *, *, #22464, .T. ) ;
#31895 = PLANE ( 'NONE',  #761 ) ;
#31896 = ADVANCED_FACE ( 'NONE', ( #24 ), #30649, .F. ) ;
#31897 = CARTESIAN_POINT ( 'NONE',  ( 0.000000000000000000, 20.00000000000000000, 0.000000000000000000 ) ) ;
#31898 = CARTESIAN_POINT ( 'NONE',  ( 18.96091535642496240, -3.614110606601104614, -2.184956778830005053 ) ) ;
#31900 = ORIENTED_EDGE ( 'NONE', *, *, #27593, .F. ) ;
#31899 = CARTESIAN_POINT ( 'NONE',  ( 2.921917104085851403E-16, 3.407865132560179866, 3.672404558090050397 ) ) ;
#31901 = CARTESIAN_POINT ( 'NONE',  ( -3.012550801365593500, 3.368539882008727115, 1.828967928396026954 ) ) ;
#31902 = B_SPLINE_SURFACE_WITH_KNOTS ( 'NONE', 3, 3, ( 
 ( #2993, #13293, #13146, #23346, #20692, #452, #26367, #8135, #25688, #3294 ),
 ( #12987, #21019, #10632, #10479, #13631, #18342, #15824, #26032, #31229, #23499 ),
 ( #5789, #610, #10803, #8306, #10977, #8454, #18499, #28696, #28195, #15965 ),
 ( #26186, #13461, #23679, #21179, #18647, #28844, #18008, #30743, #3473, #23833 ),
 ( #945, #11123, #18995, #29031, #3618, #16453, #32020, #6768, #29182, #8790 ),
 ( #1438, #16625, #3770, #31866, #24160, #16309, #27005, #6270, #1771, #26660 ),
 ( #29688, #24469, #9088, #6424, #3953, #19142, #13777, #26519, #19496, #13940 ) ),
 .UNSPECIFIED., .F., .F., .F.,
 ( 4, 3, 4 ),
 ( 4, 3, 3, 4 ),
 ( -5.415659987738848363E-12, 0.4999999999972921660, 1.000000000000000000 ),
 ( 0.003581794793000549898, 0.5017908973965002906, 0.7508954486982502008, 1.000000000000000000 ),
 .UNSPECIFIED. ) ;
#31903 = CARTESIAN_POINT ( 'NONE',  ( -50.81000000000000227, -10.96999999999998643, 5.949999999999999289 ) ) ;
#31904 = CARTESIAN_POINT ( 'NONE',  ( 6.883866601413088482, -3.754588506078551102, -7.883091392499357752 ) ) ;
#31905 = CARTESIAN_POINT ( 'NONE',  ( 10.56183597391177464, 4.753758587302147731, 0.000000000000000000 ) ) ;
#31906 = DIRECTION ( 'NONE',  ( 0.000000000000000000, -0.9659258262890710878, 0.2588190451025100258 ) ) ;
#31907 = ADVANCED_FACE ( 'NONE', ( #23097 ), #216, .T. ) ;
#31908 = CARTESIAN_POINT ( 'NONE',  ( 56.97280603064898941, -277.2763395528616002, -4.999054092451833853 ) ) ;
#31909 = DIRECTION ( 'NONE',  ( 0.000000000000000000, 1.000000000000000000, 0.000000000000000000 ) ) ;
#31910 = FACE_OUTER_BOUND ( 'NONE', #22839, .T. ) ;
#31911 = CARTESIAN_POINT ( 'NONE',  ( -1.327193056402534710, -8.327227690481549871, 5.485967528433933538 ) ) ;
#31912 = ORIENTED_EDGE ( 'NONE', *, *, #12412, .F. ) ;
#31913 = B_SPLINE_CURVE_WITH_KNOTS ( 'NONE', 3,
 ( #20178, #2118, #2298, #9304, #9620, #27183 ),
 .UNSPECIFIED., .F., .F.,
 ( 4, 2, 4 ),
 ( 2.626357090645241657E-13, 0.0003954463998646314048, 0.0007908927994666270847 ),
 .UNSPECIFIED. ) ;
#31914 = DIRECTION ( 'NONE',  ( 1.000000000000000000, 0.000000000000000000, 0.000000000000000000 ) ) ;
#31915 = ORIENTED_EDGE ( 'NONE', *, *, #25836, .T. ) ;
#31916 = CARTESIAN_POINT ( 'NONE',  ( -47.25352234179201361, 16.22999999999998266, -1.500000000000000000 ) ) ;
#31917 = EDGE_CURVE ( 'NONE', #10741, #10253, #13064, .T. ) ;
#31918 = CYLINDRICAL_SURFACE ( 'NONE', #13526, 6.999999999999998224 ) ;
#31919 = CARTESIAN_POINT ( 'NONE',  ( -2.337550801365593678, 3.368539882008727115, 1.828967928396027176 ) ) ;
#31920 = APPLICATION_CONTEXT ( 'configuration controlled 3d designs of mechanical parts and assemblies' ) ;
#31921 = PLANE ( 'NONE',  #25813 ) ;
#31922 = CARTESIAN_POINT ( 'NONE',  ( 4.749760686538667009, 6.940565734314653845, -4.007137495034738706 ) ) ;
#31923 = ORIENTED_EDGE ( 'NONE', *, *, #31643, .T. ) ;
#31924 = CARTESIAN_POINT ( 'NONE',  ( -31.18783180709124636, -25.44850941282521006, 1.500000000000000000 ) ) ;
#31925 = EDGE_CURVE ( 'NONE', #32003, #24925, #1177, .T. ) ;
#31926 = ORIENTED_EDGE ( 'NONE', *, *, #15755, .T. ) ;
#31927 = CALENDAR_DATE ( 2026, 6, 10 ) ;
#31928 = CARTESIAN_POINT ( 'NONE',  ( -3.756376981307136376, 0.1572233378491263989, -2.999999999999999556 ) ) ;
#31929 = ORIENTED_EDGE ( 'NONE', *, *, #20041, .T. ) ;
#31930 = CARTESIAN_POINT ( 'NONE',  ( 6.883866601413089370, 3.754588506078606613, 7.883091392499333772 ) ) ;
#31931 = ORIENTED_EDGE ( 'NONE', *, *, #27733, .T. ) ;
#31932 = VERTEX_POINT ( 'NONE', #18909 ) ;
#31933 = CARTESIAN_POINT ( 'NONE',  ( 0.5704035821694226627, -0.6538686328478068299, -9.519055809314993510 ) ) ;
#31934 = CARTESIAN_POINT ( 'NONE',  ( 2.440333456259504707, 10.60697035673403654, -1.206185435486470281 ) ) ;
#31935 = EDGE_CURVE ( 'NONE', #5744, #25356, #20401, .T. ) ;
#31936 = CARTESIAN_POINT ( 'NONE',  ( 21.85999999999999943, 1.573300977624590313, -1.942864903642426144 ) ) ;
#31938 = ORIENTED_EDGE ( 'NONE', *, *, #2113, .F. ) ;
#31937 = DIRECTION ( 'NONE',  ( 0.000000000000000000, 0.4067366430758009299, -0.9135454576426005335 ) ) ;
#31939 = CARTESIAN_POINT ( 'NONE',  ( -5.237550801365594033, -3.675193018007246071, 1.088641768524163167 ) ) ;
#31940 = CARTESIAN_POINT ( 'NONE',  ( 7.249760686538667009, -0.7071067811864522046, -8.721381771256211834 ) ) ;
#31941 = ADVANCED_FACE ( 'NONE', ( #9002 ), #29252, .F. ) ;
#31942 = CARTESIAN_POINT ( 'NONE',  ( 11.75198736701373825, -19.94169323712718978, 1.750535621815488385 ) ) ;
#31943 = DIRECTION ( 'NONE',  ( 1.000000000000000000, -0.000000000000000000, 0.000000000000000000 ) ) ;
#31944 = EDGE_LOOP ( 'NONE', ( #332, #8997, #5733 ) ) ;
#31946 = ORIENTED_EDGE ( 'NONE', *, *, #32889, .F. ) ;
#31945 = CARTESIAN_POINT ( 'NONE',  ( 21.64180102898656699, -16.89820628832761784, 1.499999999999856559 ) ) ;
#31947 = SPHERICAL_SURFACE ( 'NONE', #16064, 0.5000000000000000000 ) ;
#31948 = B_SPLINE_CURVE_WITH_KNOTS ( 'NONE', 3,
 ( #5539, #850, #674, #10681, #8353, #31425, #31111, #8501, #21379, #18894 ),
 .UNSPECIFIED., .F., .F.,
 ( 4, 2, 2, 2, 4 ),
 ( 2.740849916257185138E-07, 0.0005478761651001761357, 0.001095478245208724843, 0.001643080325317273658, 0.002190682405425822474 ),
 .UNSPECIFIED. ) ;
#31949 = CARTESIAN_POINT ( 'NONE',  ( 22.61000000273118715, -1.573300977624594976, 1.942864903642425700 ) ) ;
#31950 = DIRECTION ( 'NONE',  ( 0.000000000000000000, 1.000000000000000000, 0.000000000000000000 ) ) ;
#31951 = CARTESIAN_POINT ( 'NONE',  ( -30.24316686125445131, 12.14507408406858779, 1.500000000000003109 ) ) ;
#31952 = CARTESIAN_POINT ( 'NONE',  ( -3.729013601334864703, -1.848214304039853095, -1.500000000000000000 ) ) ;
#31953 = DIRECTION ( 'NONE',  ( -1.000000000000000000, -0.000000000000000000, 0.000000000000000000 ) ) ;
#31954 = CARTESIAN_POINT ( 'NONE',  ( 54.89858654025085372, -3.680211708401866399, 0.8105616792983024732 ) ) ;
#31955 = CARTESIAN_POINT ( 'NONE',  ( -3.737550801365593589, -1.828967928396026510, 3.368539882008728004 ) ) ;
#31956 = FACE_OUTER_BOUND ( 'NONE', #32043, .T. ) ;
#31957 = VERTEX_POINT ( 'NONE', #29102 ) ;
#31958 = DIRECTION ( 'NONE',  ( 8.541412920197212419E-17, 0.9961946980917449901, 0.08715574274766461904 ) ) ;
#31959 = DIRECTION ( 'NONE',  ( 1.000000000000000000, -0.000000000000000000, -0.000000000000000000 ) ) ;
#31961 = CARTESIAN_POINT ( 'NONE',  ( 23.81423349025572733, -17.27971345279117088, 1.410233427488315705 ) ) ;
#31960 = CARTESIAN_POINT ( 'NONE',  ( 6.356381935169119757, -2.055898738447941909, -8.357622142800108733 ) ) ;
#31962 = ORIENTED_EDGE ( 'NONE', *, *, #14248, .T. ) ;
#31963 = CARTESIAN_POINT ( 'NONE',  ( 20.99695690729567232, -21.77932090203123749, 1.367431712678154110 ) ) ;
#31964 = VERTEX_POINT ( 'NONE', #26583 ) ;
#31965 = FACE_OUTER_BOUND ( 'NONE', #12778, .T. ) ;
#31967 = ORIENTED_EDGE ( 'NONE', *, *, #18407, .F. ) ;
#31966 = CARTESIAN_POINT ( 'NONE',  ( 28.69356951698349434, -5.616939729258927372, -3.995336671782978577 ) ) ;
#31968 = ORIENTED_EDGE ( 'NONE', *, *, #8162, .T. ) ;
#31969 = EDGE_CURVE ( 'NONE', #27551, #10376, #1357, .T. ) ;
#31970 = EDGE_CURVE ( 'NONE', #17030, #3611, #31295, .T. ) ;
#31971 = CARTESIAN_POINT ( 'NONE',  ( -6.156376981307135843, 0.1572233378491243172, -2.999999999999999556 ) ) ;
#31973 = ORIENTED_EDGE ( 'NONE', *, *, #19564, .F. ) ;
#31972 = PLANE ( 'NONE',  #22977 ) ;
#31974 = CARTESIAN_POINT ( 'NONE',  ( 8.930755659325139817, 0.4999999999999980571, -1.500000000000000000 ) ) ;
#31975 = CARTESIAN_POINT ( 'NONE',  ( 3.499999999999999556, 6.704570150426983233, 5.172265885002680363 ) ) ;
#31976 =( BOUNDED_SURFACE ( )  B_SPLINE_SURFACE ( 1, 2, ( 
 ( #8520, #6339, #13701, #29416, #24055, #26923, #16033, #18721, #19222, #21730, #21581, #31786, #16228, #8857, #21244, #6193, #3379, #18914, #11195, #18567, #19065, #1509, #28926, #29105, #14195, #16715, #26263, #1011, #16377, #6512, #26444, #4027, #26586, #1360, #24392, #6031, #11380, #16531, #23903, #21401, #21096, #3690, #31298, #8370, #28759, #29255, #13849, #3857, #5849, #14031, #3543, #31610, #8698, #13545, #26739, #23754, #1180, #24243, #11535, #31939, #9005, #867, #11046, #31442, #6687, #32292, #9861, #12348, #12184, #22384, #6839, #32601, #11866, #29919, #27072, #9504, #1862, #9177, #9673, #25235, #9352, #19719, #4833, #7340, #16876, #24736, #7001, #30268, #17024, #17530, #17214, #25046, #27724, #19562, #2011, #30115, #4345, #12038, #15013, #27420, #11687, #21886, #19406, #19901, #4527, #27578, #32101, #4677, #29759, #22233, #27230, #29605, #7192, #4174, #14525, #14847, #17384, #2164, #14701, #32443, #14341 ),
 ( #24549, #22568, #1671, #24899, #32782, #20072, #22075, #339, #13029, #23235, #10167, #7496, #17696, #25559, #20875, #27911, #18195, #8000, #5024, #15203, #25404, #15354, #2859, #17887, #2514, #2665, #10512, #20388, #10357, #13177, #31089, #28402, #30606, #33090, #23050, #20724, #12682, #22737, #5519, #8180, #20569, #10665, #22886, #30924, #7688, #7847, #28079, #23378, #482, #5176, #15705, #28578, #18383, #25912, #12835, #12530, #5672, #174, #30776, #18040, #3022, #15852, #28229, #5335, #15516, #25729, #2355, #32941, #10011, #20222, #30417, #26063, #13983, #19030, #5985, #26223, #16342, #3165, #21359, #21209, #13323, #23718, #13505, #6462, #8652, #24014, #31568, #18872, #1324, #11155, #23536, #26551, #11333, #24202, #11009, #652, #16183, #11498, #31750, #21694, #29071, #31901, #31406, #10846, #3812, #13808, #8482, #21060, #18532, #8336, #31262, #28724, #28882, #26408, #8968, #3509, #15997, #13664, #832, #21543, #18681 ) ),
 .UNSPECIFIED., .F., .F., .F. ) 
 B_SPLINE_SURFACE_WITH_KNOTS ( ( 2, 2 ),
 ( 3, 2, 2, 2, 2, 2, 2, 2, 2, 2, 2, 2, 2, 2, 2, 2, 2, 2, 2, 2, 2, 2, 2, 2, 2, 2, 2, 2, 2, 2, 2, 2, 2, 2, 2, 2, 2, 2, 2, 2, 2, 2, 2, 2, 2, 2, 2, 2, 2, 2, 2, 2, 2, 2, 2, 2, 2, 2, 2, 2, 3 ),
 ( 0.000000000000000000, 1.000000000000000000 ),
 ( 0.000000000000000000, 0.01562500000000000000, 0.03125000000000000000, 0.04687500000000000000, 0.06250000000000000000, 0.07812500000000000000, 0.09375000000000000000, 0.1093750000000000000, 0.1250000000000000000, 0.1406250000000000000, 0.1562500000000000000, 0.1718750000000000000, 0.1875000000000000000, 0.2031250000000000000, 0.2187500000000000000, 0.2343750000000000000, 0.2500000000000000000, 0.2656250000000000000, 0.2812500000000000000, 0.2968750000000000000, 0.3125000000000000000, 0.3281250000000000000, 0.3437500000000000000, 0.3593750000000000000, 0.3750000000000000000, 0.3906250000000000000, 0.4062500000000000000, 0.4218750000000000000, 0.4375000000000000000, 0.4531250000000000000, 0.4687500000000000000, 0.4843750000000000000, 0.5000000000000000000, 0.5156250000000000000, 0.5312500000000000000, 0.5468750000000000000, 0.5625000000000000000, 0.5781250000000000000, 0.5937500000000000000, 0.6093750000000000000, 0.6250000000000000000, 0.6406250000000000000, 0.6562500000000000000, 0.6718750000000000000, 0.6875000000000000000, 0.7031250000000000000, 0.7187500000000000000, 0.7343750000000000000, 0.7500000000000000000, 0.7656250000000000000, 0.7812500000000000000, 0.7968750000000000000, 0.8125000000000000000, 0.8281250000000000000, 0.8437500000000000000, 0.8593750000000000000, 0.8750000000000000000, 0.8906250000000000000, 0.9062500000000000000, 0.9218750000000000000, 0.9375000000000000000 ),
 .UNSPECIFIED. ) 
 GEOMETRIC_REPRESENTATION_ITEM ( )  RATIONAL_B_SPLINE_SURFACE ( (
 ( 1.000000000000000000, 0.9238795325112867385, 1.000000000000000000, 0.9238795325112867385, 1.000000000000000000, 0.9238795325112867385, 1.000000000000000000, 0.9238795325112867385, 1.000000000000000000, 0.9238795325112867385, 1.000000000000000000, 0.9238795325112867385, 1.000000000000000000, 0.9238795325112867385, 1.000000000000000000, 0.9238795325112867385, 1.000000000000000000, 0.9238795325112867385, 1.000000000000000000, 0.9238795325112867385, 1.000000000000000000, 0.9238795325112867385, 1.000000000000000000, 0.9238795325112867385, 1.000000000000000000, 0.9238795325112867385, 1.000000000000000000, 0.9238795325112867385, 1.000000000000000000, 0.9238795325112867385, 1.000000000000000000, 0.9238795325112867385, 1.000000000000000000, 0.9238795325112867385, 1.000000000000000000, 0.9238795325112867385, 1.000000000000000000, 0.9238795325112867385, 1.000000000000000000, 0.9238795325112867385, 1.000000000000000000, 0.9238795325112867385, 1.000000000000000000, 0.9238795325112867385, 1.000000000000000000, 0.9238795325112867385, 1.000000000000000000, 0.9238795325112867385, 1.000000000000000000, 0.9238795325112867385, 1.000000000000000000, 0.9238795325112867385, 1.000000000000000000, 0.9238795325112867385, 1.000000000000000000, 0.9238795325112867385, 1.000000000000000000, 0.9238795325112867385, 1.000000000000000000, 0.9238795325112867385, 1.000000000000000000, 0.9238795325112867385, 1.000000000000000000, 0.9238795325112867385, 1.000000000000000000, 0.9238795325112867385, 1.000000000000000000, 0.9238795325112867385, 1.000000000000000000, 0.9238795325112867385, 1.000000000000000000, 0.9238795325112867385, 1.000000000000000000, 0.9238795325112867385, 1.000000000000000000, 0.9238795325112867385, 1.000000000000000000, 0.9238795325112867385, 1.000000000000000000, 0.9238795325112867385, 1.000000000000000000, 0.9238795325112867385, 1.000000000000000000, 0.9238795325112867385, 1.000000000000000000, 0.9238795325112867385, 1.000000000000000000, 0.9238795325112867385, 1.000000000000000000, 0.9238795325112867385, 1.000000000000000000, 0.9238795325112867385, 1.000000000000000000, 0.9238795325112867385, 1.000000000000000000, 0.9238795325112867385, 1.000000000000000000, 0.9238795325112867385, 1.000000000000000000, 0.9238795325112867385, 1.000000000000000000, 0.9238795325112867385, 1.000000000000000000, 0.9238795325112867385, 1.000000000000000000, 0.9238795325112867385, 1.000000000000000000, 0.9238795325112867385, 1.000000000000000000, 0.9238795325112867385, 1.000000000000000000, 0.9238795325112867385, 1.000000000000000000, 0.9238795325112867385, 1.000000000000000000, 0.9238795325112867385, 1.000000000000000000, 0.9238795325112867385, 1.000000000000000000, 0.9238795325112867385, 1.000000000000000000),
 ( 1.000000000000000000, 0.9238795325112867385, 1.000000000000000000, 0.9238795325112867385, 1.000000000000000000, 0.9238795325112867385, 1.000000000000000000, 0.9238795325112867385, 1.000000000000000000, 0.9238795325112867385, 1.000000000000000000, 0.9238795325112867385, 1.000000000000000000, 0.9238795325112867385, 1.000000000000000000, 0.9238795325112867385, 1.000000000000000000, 0.9238795325112867385, 1.000000000000000000, 0.9238795325112867385, 1.000000000000000000, 0.9238795325112867385, 1.000000000000000000, 0.9238795325112867385, 1.000000000000000000, 0.9238795325112867385, 1.000000000000000000, 0.9238795325112867385, 1.000000000000000000, 0.9238795325112867385, 1.000000000000000000, 0.9238795325112867385, 1.000000000000000000, 0.9238795325112867385, 1.000000000000000000, 0.9238795325112867385, 1.000000000000000000, 0.9238795325112867385, 1.000000000000000000, 0.9238795325112867385, 1.000000000000000000, 0.9238795325112867385, 1.000000000000000000, 0.9238795325112867385, 1.000000000000000000, 0.9238795325112867385, 1.000000000000000000, 0.9238795325112867385, 1.000000000000000000, 0.9238795325112867385, 1.000000000000000000, 0.9238795325112867385, 1.000000000000000000, 0.9238795325112867385, 1.000000000000000000, 0.9238795325112867385, 1.000000000000000000, 0.9238795325112867385, 1.000000000000000000, 0.9238795325112867385, 1.000000000000000000, 0.9238795325112867385, 1.000000000000000000, 0.9238795325112867385, 1.000000000000000000, 0.9238795325112867385, 1.000000000000000000, 0.9238795325112867385, 1.000000000000000000, 0.9238795325112867385, 1.000000000000000000, 0.9238795325112867385, 1.000000000000000000, 0.9238795325112867385, 1.000000000000000000, 0.9238795325112867385, 1.000000000000000000, 0.9238795325112867385, 1.000000000000000000, 0.9238795325112867385, 1.000000000000000000, 0.9238795325112867385, 1.000000000000000000, 0.9238795325112867385, 1.000000000000000000, 0.9238795325112867385, 1.000000000000000000, 0.9238795325112867385, 1.000000000000000000, 0.9238795325112867385, 1.000000000000000000, 0.9238795325112867385, 1.000000000000000000, 0.9238795325112867385, 1.000000000000000000, 0.9238795325112867385, 1.000000000000000000, 0.9238795325112867385, 1.000000000000000000, 0.9238795325112867385, 1.000000000000000000, 0.9238795325112867385, 1.000000000000000000, 0.9238795325112867385, 1.000000000000000000, 0.9238795325112867385, 1.000000000000000000, 0.9238795325112867385, 1.000000000000000000, 0.9238795325112867385, 1.000000000000000000, 0.9238795325112867385, 1.000000000000000000, 0.9238795325112867385, 1.000000000000000000, 0.9238795325112867385, 1.000000000000000000, 0.9238795325112867385, 1.000000000000000000, 0.9238795325112867385, 1.000000000000000000) ) ) 
 REPRESENTATION_ITEM ( '' )  SURFACE ( )  );
#31977 = DIRECTION ( 'NONE',  ( 1.000000000000000000, -8.574039729943018344E-17, -0.000000000000000000 ) ) ;
#31978 = CARTESIAN_POINT ( 'NONE',  ( 10.65647057407944942, -13.03481288882011491, -1.500000000000000000 ) ) ;
#31980 = ORIENTED_EDGE ( 'NONE', *, *, #23617, .T. ) ;
#31979 = CARTESIAN_POINT ( 'NONE',  ( 107.5500550589464126, -18.81356462609017655, -4.828513639309408134 ) ) ;
#31981 = DIRECTION ( 'NONE',  ( 0.000000000000000000, 0.000000000000000000, -1.000000000000000000 ) ) ;
#31982 = DIRECTION ( 'NONE',  ( 1.000000000000000000, -0.000000000000000000, -0.000000000000000000 ) ) ;
#31983 = PLANE ( 'NONE',  #17886 ) ;
#31984 = B_SPLINE_CURVE_WITH_KNOTS ( 'NONE', 3,
 ( #25511, #24849, #17483, #22692, #15307, #32730, #2619, #32895, #10115, #113, #4628, #20174, #15152, #4785 ),
 .UNSPECIFIED., .F., .F.,
 ( 4, 2, 2, 2, 2, 2, 4 ),
 ( 8.673617379884034509E-19, 0.0001249451318035515839, 0.0002498902636071023003, 0.0004997805272141984207, 0.0007496707908212945411, 0.0008746159226248436313, 0.0009995610544283927215 ),
 .UNSPECIFIED. ) ;
#31985 = CARTESIAN_POINT ( 'NONE',  ( 24.40244105150047105, -17.41898962163720554, -1.432663565948197437 ) ) ;
#31986 = CARTESIAN_POINT ( 'NONE',  ( 23.68064580653238949, -7.171681651382474598, -4.522129901861164036 ) ) ;
#31987 = ORIENTED_EDGE ( 'NONE', *, *, #6293, .T. ) ;
#31988 = DIRECTION ( 'NONE',  ( -0.9960221812693187404, 0.08910563629484180570, 0.000000000000000000 ) ) ;
#31989 = CARTESIAN_POINT ( 'NONE',  ( 107.3781042300268354, -16.32440815734132045, -2.398398155969891032 ) ) ;
#31990 = DIRECTION ( 'NONE',  ( 1.000000000000000000, 0.000000000000000000, 3.469446951953611033E-15 ) ) ;
#31991 = ORIENTED_EDGE ( 'NONE', *, *, #10526, .T. ) ;
#31992 = CARTESIAN_POINT ( 'NONE',  ( 2.357330058169011533, -7.401770933800293939, 7.915524238820718317 ) ) ;
#31993 = DIRECTION ( 'NONE',  ( 0.000000000000000000, -1.000000000000000000, 0.000000000000000000 ) ) ;
#31994 = VERTEX_POINT ( 'NONE', #6509 ) ;
#31995 = CARTESIAN_POINT ( 'NONE',  ( 3.066471221417552684, -11.21726243446034132, -1.500000000000000222 ) ) ;
#31996 = EDGE_LOOP ( 'NONE', ( #4525, #10700, #2081, #27645 ) ) ;
#31997 = EDGE_CURVE ( 'NONE', #6905, #32970, #19218, .T. ) ;
#31998 = EDGE_LOOP ( 'NONE', ( #10578, #17629, #9867, #17050 ) ) ;
#31999 = CARTESIAN_POINT ( 'NONE',  ( 25.16500339546704978, -17.49275296966160198, -1.172809483625713023 ) ) ;
#32000 = SECURITY_CLASSIFICATION_LEVEL ( 'unclassified' ) ;
#32002 = VERTEX_POINT ( 'NONE', #6336 ) ;
#32001 = CARTESIAN_POINT ( 'NONE',  ( 18.73041676179999726, -21.25644754115815260, -1.734286084696279095 ) ) ;
#32003 = VERTEX_POINT ( 'NONE', #13359 ) ;
#32004 = CARTESIAN_POINT ( 'NONE',  ( 108.6457025336241031, 16.11621187055573046, -2.334455007174250696 ) ) ;
#32005 = EDGE_LOOP ( 'NONE', ( #3946, #10690, #11314, #18219 ) ) ;
#32006 = CARTESIAN_POINT ( 'NONE',  ( 7.064632918400240769, -7.953573330858190182, -3.647351267791651086 ) ) ;
#32008 = ORIENTED_EDGE ( 'NONE', *, *, #3497, .T. ) ;
#32007 = DIRECTION ( 'NONE',  ( 4.917867153432920143E-17, 0.5735764363510367225, 0.8191520442889984599 ) ) ;
#32009 = DIRECTION ( 'NONE',  ( 0.000000000000000000, 0.000000000000000000, 1.000000000000000000 ) ) ;
#32010 = AXIS2_PLACEMENT_3D ( 'NONE', #14955, #30539, #10296 ) ;
#32011 = CARTESIAN_POINT ( 'NONE',  ( 6.880159790065803804, 0.8322990769133554734, -8.691376398188690899 ) ) ;
#32012 = B_SPLINE_CURVE_WITH_KNOTS ( 'NONE', 3,
 ( #3199, #26261, #18565, #23409, #8368, #18719, #29103, #21094, #31296, #2901 ),
 .UNSPECIFIED., .F., .F.,
 ( 4, 2, 2, 2, 4 ),
 ( 2.740849916258459394E-07, 0.0005478761651001745094, 0.001095478245208723325, 0.001643080325317272140, 0.002190682405425820739 ),
 .UNSPECIFIED. ) ;
#32013 = ADVANCED_FACE ( 'NONE', ( #28756 ), #1711, .T. ) ;
#32014 = CARTESIAN_POINT ( 'NONE',  ( -56.76080480439498643, 0.3612510994447631907, 1.709681292476414649 ) ) ;
#32015 = CARTESIAN_POINT ( 'NONE',  ( 6.530491751506347420, 5.074604403564672239, 7.017944781891974237 ) ) ;
#32016 = PLANE ( 'NONE',  #22476 ) ;
#32017 = AXIS2_PLACEMENT_3D ( 'NONE', #2048, #16916, #29466 ) ;
#32018 = FACE_OUTER_BOUND ( 'NONE', #5738, .T. ) ;
#32019 = ADVANCED_FACE ( 'NONE', ( #1008 ), #31669, .F. ) ;
#32020 = CARTESIAN_POINT ( 'NONE',  ( 35.27105150273526846, -8.350847396884441665, -0.8105616794696051119 ) ) ;
#32021 = CARTESIAN_POINT ( 'NONE',  ( 3.499999999999999556, -3.573533178329615367, 5.126388750707211450 ) ) ;
#32022 = CARTESIAN_POINT ( 'NONE',  ( 7.064632918400241657, 7.953573330858215940, 3.647351267791597351 ) ) ;
#32023 = B_SPLINE_CURVE_WITH_KNOTS ( 'NONE', 3,
 ( #18985, #32006, #14265, #3760, #11454, #16949, #16611, #4246, #24629, #18816 ),
 .UNSPECIFIED., .F., .F.,
 ( 4, 2, 2, 2, 4 ),
 ( 1.968338519012340724E-07, 0.0005467927057105486386, 0.001093388577569196071, 0.001639984449427843612, 0.002186580321286490936 ),
 .UNSPECIFIED. ) ;
#32024 = CARTESIAN_POINT ( 'NONE',  ( 3.526383166312418993, 10.27186380921758335, -5.187041768249670781 ) ) ;
#32025 = CYLINDRICAL_SURFACE ( 'NONE', #31634, 11.00000000000000000 ) ;
#32026 = EDGE_CURVE ( 'NONE', #32858, #19214, #5021, .T. ) ;
#32027 = DIRECTION ( 'NONE',  ( 0.000000000000000000, 1.000000000000000000, 0.000000000000000000 ) ) ;
#32028 = CARTESIAN_POINT ( 'NONE',  ( -5.250050802731188071, 2.331437884370912705, -1.887961173149511618 ) ) ;
#32029 = ORIENTED_EDGE ( 'NONE', *, *, #2861, .T. ) ;
#32030 = CARTESIAN_POINT ( 'NONE',  ( -6.600050800000000883, 1.887961173149511618, 2.331437884370912705 ) ) ;
#32031 = VECTOR ( 'NONE', #32950, 1000.000000000000000 ) ;
#32032 = VECTOR ( 'NONE', #31324, 1000.000000000000000 ) ;
#32033 = EDGE_CURVE ( 'NONE', #9995, #4314, #666, .T. ) ;
#32034 = CARTESIAN_POINT ( 'NONE',  ( 23.09505198155390460, -21.93193643537372495, -1.086921436894753956 ) ) ;
#32035 = DIRECTION ( 'NONE',  ( -0.000000000000000000, -0.000000000000000000, -1.000000000000000000 ) ) ;
#32036 = DIRECTION ( 'NONE',  ( 0.000000000000000000, 0.8191520442889912434, -0.5735764363510469366 ) ) ;
#32037 = ORIENTED_EDGE ( 'NONE', *, *, #23362, .F. ) ;
#32038 = CARTESIAN_POINT ( 'NONE',  ( 6.645633185707460200, -7.177124861698851888, -1.500000000000000000 ) ) ;
#32039 = ORIENTED_EDGE ( 'NONE', *, *, #1094, .T. ) ;
#32040 = CARTESIAN_POINT ( 'NONE',  ( 3.640540270743287898, -12.13672865749711605, 1.758210070446800444 ) ) ;
#32041 = DATE_AND_TIME ( #14147, #14082 ) ;
#32042 = CARTESIAN_POINT ( 'NONE',  ( 7.064423669210280643, 6.147671362330681788, 6.226446564518065330 ) ) ;
#32044 = EDGE_CURVE ( 'NONE', #23098, #19482, #15351, .T. ) ;
#32043 = EDGE_LOOP ( 'NONE', ( #30569, #18281, #12417, #23004 ) ) ;
#32045 = CARTESIAN_POINT ( 'NONE',  ( 102.3922829939908183, -3.552157972648799511, 4.312042181580753031 ) ) ;
#32046 = ADVANCED_FACE ( 'NONE', ( #5173 ), #25556, .F. ) ;
#32047 = CARTESIAN_POINT ( 'NONE',  ( 25.10659403416954660, 18.61493763628891784, -1.050000000000000266 ) ) ;
#32048 = CARTESIAN_POINT ( 'NONE',  ( 40.88330980877409360, -6.770793753989999608, -4.155404504729648174 ) ) ;
#32049 = CARTESIAN_POINT ( 'NONE',  ( 24.30482536760584367, -17.42173634883301858, -1.458717893414869904 ) ) ;
#32050 = DIRECTION ( 'NONE',  ( 1.000000000000000000, -0.000000000000000000, -0.000000000000000000 ) ) ;
#32051 = ORIENTED_EDGE ( 'NONE', *, *, #5679, .T. ) ;
#32052 = CIRCLE ( 'NONE', #17089, 8.500000000000000000 ) ;
#32053 = CARTESIAN_POINT ( 'NONE',  ( 9.236821176939054467, 0.1505923090604429360, 1.036667534179766648 ) ) ;
#32054 = CARTESIAN_POINT ( 'NONE',  ( 22.68241379554131854, -21.87740465772118270, -1.258814731508510087 ) ) ;
#32055 = CARTESIAN_POINT ( 'NONE',  ( 5.489343958331425632, -7.593062460271018388, 2.874233210898338609 ) ) ;
#32056 = AXIS2_PLACEMENT_3D ( 'NONE', #24053, #12036, #1178 ) ;
#32058 = VERTEX_POINT ( 'NONE', #20721 ) ;
#32057 = CARTESIAN_POINT ( 'NONE',  ( 25.67092775740384170, 2.589206504880454229, -1.404329851040918342 ) ) ;
#32059 = FACE_OUTER_BOUND ( 'NONE', #23744, .T. ) ;
#32060 = CIRCLE ( 'NONE', #18704, 8.025310301077755781 ) ;
#32061 = CARTESIAN_POINT ( 'NONE',  ( 29.41391112839825794, -2.700987858898180161, 0.07017451552781951707 ) ) ;
#32062 = CARTESIAN_POINT ( 'NONE',  ( -4.500050802731188071, 1.549418761218566143, -2.853674364686379583 ) ) ;
#32063 = LINE ( 'NONE', #19531, #18754 ) ;
#32064 = DIRECTION ( 'NONE',  ( 0.000000000000000000, -0.9063077870366542665, 0.4226182617406900044 ) ) ;
#32065 = EDGE_CURVE ( 'NONE', #32100, #3931, #18037, .T. ) ;
#32066 = CIRCLE ( 'NONE', #3249, 298.4532556727466499 ) ;
#32067 = CARTESIAN_POINT ( 'NONE',  ( 25.75999999999999801, -2.208672634433321348E-15, -2.499999999999997780 ) ) ;
#32068 = CARTESIAN_POINT ( 'NONE',  ( 4.749760686538667009, 7.530955069117513112, 2.741043480754951744 ) ) ;
#32069 = DIRECTION ( 'NONE',  ( -7.770718973608973726E-17, -0.9063077870366497146, 0.4226182617406998854 ) ) ;
#32070 = EDGE_LOOP ( 'NONE', ( #6380, #2071, #3276, #10687 ) ) ;
#32071 = CARTESIAN_POINT ( 'NONE',  ( 5.377543748152549874, 2.741043480754926875, 7.530955069117522882 ) ) ;
#32072 = VERTEX_POINT ( 'NONE', #25401 ) ;
#32073 = CARTESIAN_POINT ( 'NONE',  ( 25.52557118915447987, -17.56218954043521663, -1.000000000000000444 ) ) ;
#32074 = CARTESIAN_POINT ( 'NONE',  ( 3.063284526839887167, 0.000000000000000000, 0.000000000000000000 ) ) ;
#32075 = AXIS2_PLACEMENT_3D ( 'NONE', #19223, #6840, #24244 ) ;
#32076 = FACE_BOUND ( 'NONE', #2098, .T. ) ;
#32077 = CIRCLE ( 'NONE', #18203, 0.5000000000000004441 ) ;
#32078 = DIRECTION ( 'NONE',  ( 0.000000000000000000, -0.7431448254773862505, -0.6691306063588670083 ) ) ;
#32079 = PLANE ( 'NONE',  #22620 ) ;
#32080 = ORIENTED_EDGE ( 'NONE', *, *, #25936, .T. ) ;
#32081 = CARTESIAN_POINT ( 'NONE',  ( 107.9275968081481238, 17.77499038371485440, -4.611092782519711442 ) ) ;
#32082 = EDGE_CURVE ( 'NONE', #4614, #8864, #16653, .T. ) ;
#32083 = AXIS2_PLACEMENT_3D ( 'NONE', #12148, #5421, #25010 ) ;
#32084 = AXIS2_PLACEMENT_3D ( 'NONE', #2470, #12485, #32898 ) ;
#32085 = ORIENTED_EDGE ( 'NONE', *, *, #11401, .F. ) ;
#32086 = DATE_TIME_ROLE ( 'classification_date' ) ;
#32087 = EDGE_CURVE ( 'NONE', #28296, #2170, #32938, .T. ) ;
#32088 = DIRECTION ( 'NONE',  ( 0.000000000000000000, 0.000000000000000000, 1.000000000000000000 ) ) ;
#32089 = EDGE_CURVE ( 'NONE', #1782, #17721, #8127, .T. ) ;
#32090 = AXIS2_PLACEMENT_3D ( 'NONE', #6863, #17052, #4378 ) ;
#32091 = DIRECTION ( 'NONE',  ( 1.387778780781445676E-14, 0.000000000000000000, -1.000000000000000000 ) ) ;
#32092 = LINE ( 'NONE', #16705, #22045 ) ;
#32093 = ORIENTED_EDGE ( 'NONE', *, *, #25415, .F. ) ;
#32094 = ORIENTED_EDGE ( 'NONE', *, *, #886, .F. ) ;
#32095 = CARTESIAN_POINT ( 'NONE',  ( 107.4500373638809947, -17.36019379023286646, 4.522129901861156931 ) ) ;
#32096 = DIRECTION ( 'NONE',  ( 0.000000000000000000, -0.2588190451025291217, 0.9659258262890659807 ) ) ;
#32097 = CARTESIAN_POINT ( 'NONE',  ( 22.36000000000000298, -1.573300977624594976, 1.942864903642425700 ) ) ;
#32098 = CARTESIAN_POINT ( 'NONE',  ( 2.325338337819572221, -10.58933493131363690, -1.500000000000000000 ) ) ;
#32100 = VERTEX_POINT ( 'NONE', #27721 ) ;
#32099 = DIRECTION ( 'NONE',  ( 8.574039729943018344E-17, 1.000000000000000000, 0.000000000000000000 ) ) ;
#32101 = CARTESIAN_POINT ( 'NONE',  ( -2.887550801365593500, -2.752080473201636845, 2.228590825266444586 ) ) ;
#32102 = DIRECTION ( 'NONE',  ( 0.000000000000000000, 0.000000000000000000, -1.000000000000000000 ) ) ;
#32103 = VECTOR ( 'NONE', #6771, 1000.000000000000227 ) ;
#32104 = CARTESIAN_POINT ( 'NONE',  ( 47.98568197278774505, -2.821418575600922019, 0.07017451552782173751 ) ) ;
#32105 = DIRECTION ( 'NONE',  ( 0.000000000000000000, -0.000000000000000000, 1.000000000000000000 ) ) ;
#32106 = CIRCLE ( 'NONE', #4321, 8.000000000000000000 ) ;
#32107 = ORIENTED_EDGE ( 'NONE', *, *, #17035, .T. ) ;
#32109 = VERTEX_POINT ( 'NONE', #10008 ) ;
#32108 = CARTESIAN_POINT ( 'NONE',  ( 2.637178239634298205, -1.030952082498953744E-33, 1.518998482601880973 ) ) ;
#32110 = CIRCLE ( 'NONE', #28379, 10.68156436372894902 ) ;
#32112 = ADVANCED_FACE ( 'NONE', ( #20219 ), #23065, .F. ) ;
#32111 = CIRCLE ( 'NONE', #21948, 0.5000000000000000000 ) ;
#32113 = PRODUCT_DEFINITION ( 'UNKNOWN', '', #1824, #19273 ) ;
#32115 = CIRCLE ( 'NONE', #10213, 0.4499999999999996225 ) ;
#32114 = CARTESIAN_POINT ( 'NONE',  ( 3.249999999999999556, 6.772677083992467928, -5.538577986808824960 ) ) ;
#32116 = DIRECTION ( 'NONE',  ( 0.000000000000000000, 0.000000000000000000, -1.000000000000000000 ) ) ;
#32117 = DIRECTION ( 'NONE',  ( 1.000000000000000000, 0.000000000000000000, 0.000000000000000000 ) ) ;
#32118 = FACE_OUTER_BOUND ( 'NONE', #9797, .T. ) ;
#32119 = VECTOR ( 'NONE', #6410, 1000.000000000000000 ) ;
#32120 = LINE ( 'NONE', #880, #8177 ) ;
#32121 = CARTESIAN_POINT ( 'NONE',  ( 41.34552818480883474, -4.491668296273251038, 2.184957213357078043 ) ) ;
#32122 = CARTESIAN_POINT ( 'NONE',  ( -2.387550801365593056, 3.521866450007987037, 0.3701630799359328372 ) ) ;
#32123 = ORIENTED_EDGE ( 'NONE', *, *, #25393, .T. ) ;
#32124 = DIRECTION ( 'NONE',  ( -1.000000000000000000, 0.000000000000000000, 0.000000000000000000 ) ) ;
#32125 = ORIENTED_EDGE ( 'NONE', *, *, #3772, .F. ) ;
#32126 = EDGE_CURVE ( 'NONE', #32283, #15594, #20943, .T. ) ;
#32127 = CARTESIAN_POINT ( 'NONE',  ( 0.000000000000000000, 1.106368468154540263, -8.427689411260562480 ) ) ;
#32128 = CIRCLE ( 'NONE', #30009, 10.64228691119593151 ) ;
#32129 = CARTESIAN_POINT ( 'NONE',  ( 2.274274201625327230, 1.975651141462238858, 10.82112760146736896 ) ) ;
#32130 = MANIFOLD_SOLID_BREP ( 'Shell1', #31270 ) ;
#32132 = CARTESIAN_POINT ( 'NONE',  ( 107.9803621325096685, -17.78658171004472521, 4.330008079635504714 ) ) ;
#32131 = CARTESIAN_POINT ( 'NONE',  ( 6.880159790065803804, 2.190520500543487348, 8.451885315426432399 ) ) ;
#32133 = ORIENTED_EDGE ( 'NONE', *, *, #30354, .T. ) ;
#32134 = AXIS2_PLACEMENT_3D ( 'NONE', #19145, #16961, #16633 ) ;
#32135 = CIRCLE ( 'NONE', #111, 8.749000000000002331 ) ;
#32136 = LINE ( 'NONE', #19589, #29968 ) ;
#32137 = CIRCLE ( 'NONE', #28898, 9.269952810656748809 ) ;
#32138 = EDGE_LOOP ( 'NONE', ( #5545, #3589, #20099, #14407, #20025 ) ) ;
#32139 = DIRECTION ( 'NONE',  ( -0.000000000000000000, 0.08715574274765541807, -0.9961946980917457672 ) ) ;
#32141 = ORIENTED_EDGE ( 'NONE', *, *, #29595, .T. ) ;
#32140 = CARTESIAN_POINT ( 'NONE',  ( 28.69357550994990902, -5.616729480415231457, -3.995006647729451466 ) ) ;
#32142 = VERTEX_POINT ( 'NONE', #16739 ) ;
#32143 = VECTOR ( 'NONE', #10542, 1000.000000000000000 ) ;
#32144 = CARTESIAN_POINT ( 'NONE',  ( 6.883866621640342132, 6.123537914202324295, -6.224335161394955129 ) ) ;
#32145 = CIRCLE ( 'NONE', #96, 0.5000000000000004441 ) ;
#32147 = VECTOR ( 'NONE', #12298, 1000.000000000000000 ) ;
#32146 = CARTESIAN_POINT ( 'NONE',  ( 29.41391112839824373, -2.700987858903441730, 1.010822989962091301 ) ) ;
#32149 = ORIENTED_EDGE ( 'NONE', *, *, #24714, .F. ) ;
#32148 = CARTESIAN_POINT ( 'NONE',  ( 3.326404063733029215, -17.46746234660859187, -1.500000000000001776 ) ) ;
#32150 = CARTESIAN_POINT ( 'NONE',  ( 3.958196854299250007E-16, 4.616489984850531414, 1.946309384392607811 ) ) ;
#32151 = FACE_OUTER_BOUND ( 'NONE', #5890, .T. ) ;
#32152 = CARTESIAN_POINT ( 'NONE',  ( 5.887530024394193262, -3.218326717262310677, 7.753515897409877233 ) ) ;
#32153 = CARTESIAN_POINT ( 'NONE',  ( 6.694810660865504914, -7.699995848971193269, -1.500000000000000000 ) ) ;
#32156 = EDGE_CURVE ( 'NONE', #32786, #15111, #4545, .T. ) ;
#32155 = VERTEX_POINT ( 'NONE', #16549 ) ;
#32154 = CARTESIAN_POINT ( 'NONE',  ( 107.9963546461726622, -18.01686992834544654, -5.137599899355107524 ) ) ;
#32157 = CARTESIAN_POINT ( 'NONE',  ( 10.00000000000000000, -3.641590349731909537, -3.055657119358837992 ) ) ;
#32158 = CIRCLE ( 'NONE', #24748, 10.94895958125474245 ) ;
#32159 = AXIS2_PLACEMENT_3D ( 'NONE', #2096, #24985, #14633 ) ;
#32160 = DIRECTION ( 'NONE',  ( 0.000000000000000000, 0.000000000000000000, -1.000000000000000000 ) ) ;
#32161 = DIRECTION ( 'NONE',  ( 1.000000000000000000, 0.000000000000000000, 0.000000000000000000 ) ) ;
#32162 = AXIS2_PLACEMENT_3D ( 'NONE', #30245, #32576, #14322 ) ;
#32163 = AXIS2_PLACEMENT_3D ( 'NONE', #9553, #32836, #12580 ) ;
#32164 = VECTOR ( 'NONE', #21986, 1000.000000000000000 ) ;
#32165 = B_SPLINE_CURVE_WITH_KNOTS ( 'NONE', 3,
 ( #30616, #25740, #15025, #17539, #12539, #28087, #22745, #13039 ),
 .UNSPECIFIED., .F., .F.,
 ( 4, 2, 2, 4 ),
 ( 2.333100269167940293E-07, 0.001262083418509050764, 0.001893008472750115590, 0.002523933526991180634 ),
 .UNSPECIFIED. ) ;
#32166 = DIRECTION ( 'NONE',  ( 0.000000000000000000, 0.8191520442889936859, -0.5735764363510433839 ) ) ;
#32167 = CARTESIAN_POINT ( 'NONE',  ( 0.6791198416090081791, -7.715582677070901951, -4.928602827912293094 ) ) ;
#32168 = ORIENTED_EDGE ( 'NONE', *, *, #32372, .F. ) ;
#32169 = CARTESIAN_POINT ( 'NONE',  ( -54.06000000000000227, -10.96999999999998643, 5.700000000000000178 ) ) ;
#32170 = AXIS2_PLACEMENT_3D ( 'NONE', #32446, #27422, #16878 ) ;
#32171 = FACE_OUTER_BOUND ( 'NONE', #27757, .T. ) ;
#32172 = EDGE_CURVE ( 'NONE', #23146, #27444, #17975, .T. ) ;
#32173 = CARTESIAN_POINT ( 'NONE',  ( 5.377543748152550762, 7.530955069117551304, -2.741043480754851380 ) ) ;
#32174 = ORIENTED_EDGE ( 'NONE', *, *, #26122, .F. ) ;
#32175 = EDGE_CURVE ( 'NONE', #26433, #28422, #1881, .T. ) ;
#32176 = AXIS2_PLACEMENT_3D ( 'NONE', #17826, #28028, #30875 ) ;
#32177 = EDGE_CURVE ( 'NONE', #30224, #22455, #12909, .T. ) ;
#32178 = CARTESIAN_POINT ( 'NONE',  ( 7.249760686538667009, 4.007137495034812424, 6.940565734314612101 ) ) ;
#32179 = CARTESIAN_POINT ( 'NONE',  ( 2.386646147131364248, -0.3554301312245153333, -1.500000000000000666 ) ) ;
#32180 = ORIENTED_EDGE ( 'NONE', *, *, #8308, .T. ) ;
#32181 = CARTESIAN_POINT ( 'NONE',  ( -5.175170698068149555, 0.000000000000000000, -5.403836275575627290 ) ) ;
#32182 = ORIENTED_EDGE ( 'NONE', *, *, #18889, .T. ) ;
#32183 = ORIENTED_EDGE ( 'NONE', *, *, #19034, .F. ) ;
#32184 = DIRECTION ( 'NONE',  ( 0.000000000000000000, 1.000000000000000000, 0.000000000000000000 ) ) ;
#32185 = AXIS2_PLACEMENT_3D ( 'NONE', #195, #4852, #10374 ) ;
#32187 = ORIENTED_EDGE ( 'NONE', *, *, #32126, .T. ) ;
#32186 = CARTESIAN_POINT ( 'NONE',  ( 5.377543748152548098, -6.940565734314625423, 4.007137495034787555 ) ) ;
#32188 = ORIENTED_EDGE ( 'NONE', *, *, #461, .T. ) ;
#32189 = CARTESIAN_POINT ( 'NONE',  ( 20.86000000136559507, -0.9349337715887247047, 3.156283516753367824 ) ) ;
#32190 = AXIS2_PLACEMENT_3D ( 'NONE', #28851, #20844, #18350 ) ;
#32191 = CIRCLE ( 'NONE', #10815, 8.749000000000002331 ) ;
#32192 = EDGE_LOOP ( 'NONE', ( #25408, #12167, #28354, #934, #13614 ) ) ;
#32193 = DIRECTION ( 'NONE',  ( -4.917867153433010739E-17, -0.5735764363510469366, -0.8191520442889912434 ) ) ;
#32194 = CARTESIAN_POINT ( 'NONE',  ( 7.249760686538667009, -7.892520144992443143, 1.391664247347202288 ) ) ;
#32196 = ORIENTED_EDGE ( 'NONE', *, *, #29184, .F. ) ;
#32195 = PLANE ( 'NONE',  #6934 ) ;
#32197 = LINE ( 'NONE', #17562, #24688 ) ;
#32198 = CARTESIAN_POINT ( 'NONE',  ( 3.249999999999999556, 5.538577986808899567, 6.772677083992407532 ) ) ;
#32199 = AXIS2_PLACEMENT_3D ( 'NONE', #8559, #8743, #13888 ) ;
#32200 =( GEOMETRIC_REPRESENTATION_CONTEXT ( 3 ) GLOBAL_UNCERTAINTY_ASSIGNED_CONTEXT ( ( #5478 ) ) GLOBAL_UNIT_ASSIGNED_CONTEXT ( ( #5446, #10610, #28525 ) ) REPRESENTATION_CONTEXT ( 'NONE', 'WORKASPACE' ) );
#32201 = CARTESIAN_POINT ( 'NONE',  ( -56.77537022611499395, 0.4514244267945254907, 2.028141679927229379 ) ) ;
#32202 = CARTESIAN_POINT ( 'NONE',  ( 2.274274201627287884, 5.222868219167418502, -9.680994141364108074 ) ) ;
#32203 = VECTOR ( 'NONE', #12067, 1000.000000000000227 ) ;
#32204 = CARTESIAN_POINT ( 'NONE',  ( -2.786590204610737587, -5.640011313469492471, -4.522129901861166701 ) ) ;
#32205 = CARTESIAN_POINT ( 'NONE',  ( 0.7632845268398871230, 0.000000000000000000, 0.000000000000000000 ) ) ;
#32206 = DIRECTION ( 'NONE',  ( 1.000000000000000000, 0.000000000000000000, 0.000000000000000000 ) ) ;
#32207 = ADVANCED_FACE ( 'NONE', ( #22252 ), #16894, .T. ) ;
#32208 = CARTESIAN_POINT ( 'NONE',  ( 0.000000000000000000, -7.533794289457995674, -7.944914065997195074 ) ) ;
#32209 = TOROIDAL_SURFACE ( 'NONE', #14010, 7.482234843104714983, 0.5000000000000000000 ) ;
#32210 = DIRECTION ( 'NONE',  ( -1.000000000000000000, 0.000000000000000000, -0.000000000000000000 ) ) ;
#32211 = LINE ( 'NONE', #1777, #7034 ) ;
#32212 = B_SPLINE_CURVE_WITH_KNOTS ( 'NONE', 3,
 ( #9354, #12040, #20074, #32104, #12351, #32784, #29921, #1511 ),
 .UNSPECIFIED., .F., .F.,
 ( 4, 2, 2, 4 ),
 ( 0.000000000000000000, 0.5000000000000000000, 0.7500000000000000000, 1.000000000000000000 ),
 .UNSPECIFIED. ) ;
#32213 = CIRCLE ( 'NONE', #17781, 6.248999999999999666 ) ;
#32214 = AXIS2_PLACEMENT_3D ( 'NONE', #18883, #19038, #20884 ) ;
#32215 = DIRECTION ( 'NONE',  ( -0.1027947991993878041, 0.9947025833170222153, 0.000000000000000000 ) ) ;
#32216 = CARTESIAN_POINT ( 'NONE',  ( -5.050050802731187005, 1.887961173149511618, 2.331437884370912705 ) ) ;
#32217 = ORIENTED_EDGE ( 'NONE', *, *, #32065, .T. ) ;
#32218 = CIRCLE ( 'NONE', #3392, 4.000000000000001776 ) ;
#32219 = AXIS2_PLACEMENT_3D ( 'NONE', #17717, #17232, #14356 ) ;
#32220 = CARTESIAN_POINT ( 'NONE',  ( -7.587550801365593678, -3.521866450007987037, -0.3701630799359323931 ) ) ;
#32221 = CIRCLE ( 'NONE', #3397, 6.249000000000001442 ) ;
#32222 = CARTESIAN_POINT ( 'NONE',  ( -34.98193025661426248, 0.5174497483512505713, 2.552009564962238297 ) ) ;
#32223 = CYLINDRICAL_SURFACE ( 'NONE', #30565, 0.5000000000000004441 ) ;
#32224 = CARTESIAN_POINT ( 'NONE',  ( 6.734961451239206198, -5.723322302743246937, 1.500000000000000000 ) ) ;
#32225 = AXIS2_PLACEMENT_3D ( 'NONE', #32884, #20165, #15297 ) ;
#32226 = ORIENTED_EDGE ( 'NONE', *, *, #1848, .T. ) ;
#32227 = CARTESIAN_POINT ( 'NONE',  ( -30.49402871571406948, -10.96966150227469505, -11.50000000000000000 ) ) ;
#32228 = CARTESIAN_POINT ( 'NONE',  ( 107.1769020805352142, 16.40214705320008903, 1.508259000770581615 ) ) ;
#32229 = ORIENTED_EDGE ( 'NONE', *, *, #6195, .T. ) ;
#32230 = CARTESIAN_POINT ( 'NONE',  ( 3.985780818972730177, -12.21549014006416733, 1.500000000000104583 ) ) ;
#32231 = CALENDAR_DATE ( 2026, 6, 10 ) ;
#32232 = LINE ( 'NONE', #4282, #27798 ) ;
#32233 = ORIENTED_EDGE ( 'NONE', *, *, #14071, .F. ) ;
#32234 = CARTESIAN_POINT ( 'NONE',  ( -3.368890048313184504, -11.43143575104568832, 1.500000000000000666 ) ) ;
#32235 = B_SPLINE_CURVE_WITH_KNOTS ( 'NONE', 3,
 ( #8984, #19195, #15404, #16201, #5827, #2727, #12901, #20624, #30832, #18546, #27395, #4654 ),
 .UNSPECIFIED., .F., .F.,
 ( 4, 2, 2, 2, 2, 4 ),
 ( -5.999999992760755618E-08, 0.0005421413210631730083, 0.0008132419815947244772, 0.001084342642126276055, 0.001626543963189388967, 0.002168745284252502313 ),
 .UNSPECIFIED. ) ;
#32236 = FACE_OUTER_BOUND ( 'NONE', #7263, .T. ) ;
#32237 = VECTOR ( 'NONE', #2088, 1000.000000000000000 ) ;
#32238 = CARTESIAN_POINT ( 'NONE',  ( 54.96481031291111918, -6.058022586596120362, -4.312042181587000478 ) ) ;
#32239 = CYLINDRICAL_SURFACE ( 'NONE', #6657, 5.000000000000002665 ) ;
#32240 = DIRECTION ( 'NONE',  ( 0.000000000000000000, -0.9271838545667856479, -0.3746065934159163446 ) ) ;
#32241 = CIRCLE ( 'NONE', #17198, 6.999999999999998224 ) ;
#32242 = VERTEX_POINT ( 'NONE', #24918 ) ;
#32243 = AXIS2_PLACEMENT_3D ( 'NONE', #10819, #11135, #8316 ) ;
#32244 = CARTESIAN_POINT ( 'NONE',  ( 8.878230740118540965, 0.000000000000000000, 1.080849929302613033 ) ) ;
#32245 = CARTESIAN_POINT ( 'NONE',  ( 3.499999999999999556, 0.000000000000000000, 0.000000000000000000 ) ) ;
#32246 = CIRCLE ( 'NONE', #32797, 5.009999999999999787 ) ;
#32247 = CARTESIAN_POINT ( 'NONE',  ( -8.000050800000000351, 3.673940397442060361E-16, 3.000000000000000444 ) ) ;
#32248 = AXIS2_PLACEMENT_3D ( 'NONE', #14035, #1865, #1675 ) ;
#32250 = VERTEX_POINT ( 'NONE', #12057 ) ;
#32249 = CARTESIAN_POINT ( 'NONE',  ( 25.75999999999999801, 2.805042440084548172, 1.132414195126726364 ) ) ;
#32251 = DIRECTION ( 'NONE',  ( -1.000000000000000000, -0.000000000000000000, -0.000000000000000000 ) ) ;
#32252 = ADVANCED_FACE ( 'NONE', ( #27443 ), #24411, .T. ) ;
#32253 = CARTESIAN_POINT ( 'NONE',  ( -31.43793636962779203, -21.68942756709066089, 1.500000000000000000 ) ) ;
#32254 = CARTESIAN_POINT ( 'NONE',  ( 6.530491712438075247, -3.778856441136667854, -7.792522225867680952 ) ) ;
#32255 = CARTESIAN_POINT ( 'NONE',  ( 3.499999999999999556, -7.009698679648292519, 0.7308381473896670144 ) ) ;
#32256 = DIRECTION ( 'NONE',  ( -0.000000000000000000, 0.000000000000000000, 1.000000000000000000 ) ) ;
#32257 = CC_DESIGN_SECURITY_CLASSIFICATION ( #6052, ( #4466 ) ) ;
#32258 = CARTESIAN_POINT ( 'NONE',  ( -8.000050800000000351, 3.450593544762993847, 0.6811748426398763767 ) ) ;
#32259 = CARTESIAN_POINT ( 'NONE',  ( 5.612974441954674099, -6.163896661468935001, -5.432722698947220152 ) ) ;
#32260 = CARTESIAN_POINT ( 'NONE',  ( 5.377543748152548986, 4.007137495034812424, 6.940565734314612101 ) ) ;
#32261 = CARTESIAN_POINT ( 'NONE',  ( -28.03476286530682771, 5.886549661986336446, 2.094166778015133623 ) ) ;
#32262 = ORIENTED_EDGE ( 'NONE', *, *, #31428, .T. ) ;
#32263 = EDGE_CURVE ( 'NONE', #18451, #8590, #2799, .T. ) ;
#32264 = CARTESIAN_POINT ( 'NONE',  ( -2.750050802731187627, 2.983565686104819648, 0.3135853898029609677 ) ) ;
#32265 = ORIENTED_EDGE ( 'NONE', *, *, #9393, .T. ) ;
#32266 = CARTESIAN_POINT ( 'NONE',  ( -7.904531657079157725, -2.975847129947406522, -0.3127741368606805072 ) ) ;
#32267 =( BOUNDED_SURFACE ( )  B_SPLINE_SURFACE ( 1, 3, ( 
 ( #24863, #2478, #9821, #32563 ),
 ( #20039, #30233, #27692, #12647 ) ),
 .UNSPECIFIED., .F., .F., .F. ) 
 B_SPLINE_SURFACE_WITH_KNOTS ( ( 2, 2 ),
 ( 4, 4 ),
 ( 0.000000000000000000, 1.000000000000000000 ),
 ( 0.000000000000000000, 1.000000000000000000 ),
 .UNSPECIFIED. ) 
 GEOMETRIC_REPRESENTATION_ITEM ( )  RATIONAL_B_SPLINE_SURFACE ( (
 ( 1.000000000000000000, 0.9917560313531952332, 0.9917560313531952332, 1.000000000000000000),
 ( 1.000000000000000000, 0.9917560313531952332, 0.9917560313531952332, 1.000000000000000000) ) ) 
 REPRESENTATION_ITEM ( '' )  SURFACE ( )  );
#32268 = CIRCLE ( 'NONE', #6610, 5.010000000000000675 ) ;
#32269 = CARTESIAN_POINT ( 'NONE',  ( 17.75999999999999801, -2.208672634433321348E-15, -2.499999999999996891 ) ) ;
#32270 = CARTESIAN_POINT ( 'NONE',  ( 48.01729800609908949, -4.703650321873321438, -4.522129901861162260 ) ) ;
#32271 = CARTESIAN_POINT ( 'NONE',  ( 3.499999999999999556, 8.265874651078016555, 1.981241088980809639 ) ) ;
#32272 = CARTESIAN_POINT ( 'NONE',  ( 25.82046699000660439, 24.17190842697641173, 2.806473568333437196 ) ) ;
#32273 = EDGE_LOOP ( 'NONE', ( #23892, #13273, #21089, #22264 ) ) ;
#32274 = CYLINDRICAL_SURFACE ( 'NONE', #28958, 302.4235430809786180 ) ;
#32275 = ADVANCED_FACE ( 'NONE', ( #24569 ), #11318, .T. ) ;
#32276 = VERTEX_POINT ( 'NONE', #11891 ) ;
#32277 = APPROVAL_ROLE ( '' ) ;
#32279 = CARTESIAN_POINT ( 'NONE',  ( 102.4227322578115462, -3.991710622338239034, 4.006107067514854236 ) ) ;
#32278 = LOCAL_TIME ( 16, 7, 10.00000000000000000, #23703 ) ;
#32280 = EDGE_CURVE ( 'NONE', #3978, #20330, #5464, .T. ) ;
#32281 = DIRECTION ( 'NONE',  ( 0.000000000000000000, 0.000000000000000000, 1.000000000000000000 ) ) ;
#32282 = CARTESIAN_POINT ( 'NONE',  ( 0.000000000000000000, 1.699438267350371179, 9.241976615262162298 ) ) ;
#32283 = VERTEX_POINT ( 'NONE', #7026 ) ;
#32284 = ORIENTED_EDGE ( 'NONE', *, *, #28572, .T. ) ;
#32285 = CARTESIAN_POINT ( 'NONE',  ( 24.73499999999999943, -0.2613211581691358698, -2.486304738420681559 ) ) ;
#32286 = CARTESIAN_POINT ( 'NONE',  ( -2.312550801365593767, 3.675193018007246959, -1.088641768524161391 ) ) ;
#32287 = CARTESIAN_POINT ( 'NONE',  ( 25.54750000000000298, -2.594547506269383685, -0.7685399846772043020 ) ) ;
#32288 = CARTESIAN_POINT ( 'NONE',  ( 8.438478135943391578, -14.31961526477670787, -1.500000000000000444 ) ) ;
#32290 = ORIENTED_EDGE ( 'NONE', *, *, #22667, .F. ) ;
#32289 = CARTESIAN_POINT ( 'NONE',  ( 5.489344046532323773, 3.969101778624022803, -7.082516960462276856 ) ) ;
#32291 = AXIS2_PLACEMENT_3D ( 'NONE', #9276, #24643, #24470 ) ;
#32292 = CARTESIAN_POINT ( 'NONE',  ( -4.937550801365593323, 1.828967928396027176, -3.368539882008727115 ) ) ;
#32293 = CARTESIAN_POINT ( 'NONE',  ( 3.499999999999999556, -5.848742439617878652, -6.167836887841044557 ) ) ;
#32294 = CARTESIAN_POINT ( 'NONE',  ( 3.499999999999999556, 1.459547570502463198, -6.894905428400257996 ) ) ;
#32295 = FACE_OUTER_BOUND ( 'NONE', #30740, .T. ) ;
#32296 = EDGE_LOOP ( 'NONE', ( #10608, #22504, #19754, #3526, #25668 ) ) ;
#32298 = VERTEX_POINT ( 'NONE', #14213 ) ;
#32297 = CARTESIAN_POINT ( 'NONE',  ( 5.887530180601100227, -7.076866030741283176, -4.515817126386082236 ) ) ;
#32299 = CARTESIAN_POINT ( 'NONE',  ( 2.440333863881506637, 7.210444323284797008, 7.872241054360181955 ) ) ;
#32300 = DIRECTION ( 'NONE',  ( -0.4999999999999960032, -0.8660254037844409281, 0.000000000000000000 ) ) ;
#32301 = ADVANCED_FACE ( 'NONE', ( #31956 ), #9714, .F. ) ;
#32302 = ORGANIZATION ( 'NAUO-ORG4', 'UNSPECIFIED', 'UNSPECIFIED' ) ;
#32303 = EDGE_CURVE ( 'NONE', #11796, #25815, #28735, .T. ) ;
#32304 = CARTESIAN_POINT ( 'NONE',  ( 24.67250000136559507, 3.024605502323846729, -0.3178988483021056854 ) ) ;
#32305 = CARTESIAN_POINT ( 'NONE',  ( -17.34999999999999787, -10.96966150227469505, -11.00000000000000000 ) ) ;
#32306 = CARTESIAN_POINT ( 'NONE',  ( -4.280320213591900291, -6.512170938462894298, -1.499999999999840128 ) ) ;
#32307 = DIRECTION ( 'NONE',  ( 1.000000000000000000, 0.000000000000000000, 0.000000000000000000 ) ) ;
#32308 = DIRECTION ( 'NONE',  ( 0.000000000000000000, 0.000000000000000000, -1.000000000000000000 ) ) ;
#32309 = CARTESIAN_POINT ( 'NONE',  ( -3.887550801365593500, 2.228590825266444142, 2.752080473201636845 ) ) ;
#32310 = ORIENTED_EDGE ( 'NONE', *, *, #19958, .T. ) ;
#32311 = EDGE_CURVE ( 'NONE', #33059, #16776, #17239, .T. ) ;
#32312 = VERTEX_POINT ( 'NONE', #17550 ) ;
#32313 = AXIS2_PLACEMENT_3D ( 'NONE', #29926, #17226, #2175 ) ;
#32314 = CARTESIAN_POINT ( 'NONE',  ( 5.865515302491369098, 15.00000000000000000, 1.500000000000000000 ) ) ;
#32315 =( NAMED_UNIT ( * ) PLANE_ANGLE_UNIT ( ) SI_UNIT ( $, .RADIAN. ) );
#32316 = CARTESIAN_POINT ( 'NONE',  ( 7.249760686538667009, 6.147671362329219846, 6.226446564517938320 ) ) ;
#32317 = CYLINDRICAL_SURFACE ( 'NONE', #19824, 8.749000000000002331 ) ;
#32318 = ORIENTED_EDGE ( 'NONE', *, *, #30556, .T. ) ;
#32319 = EDGE_CURVE ( 'NONE', #14922, #12410, #30789, .T. ) ;
#32320 = APPROVAL ( #18320, 'UNKNOWN' ) ;
#32321 = DIRECTION ( 'NONE',  ( 0.000000000000000000, 0.000000000000000000, 1.000000000000000000 ) ) ;
#32322 = ORIENTED_EDGE ( 'NONE', *, *, #16663, .T. ) ;
#32323 = CARTESIAN_POINT ( 'NONE',  ( 8.911384905465473238, 0.2172754300402719996, 1.412391582771868492 ) ) ;
#32325 = EDGE_LOOP ( 'NONE', ( #8861, #16018, #22117, #11600, #19700, #9568, #30392, #13786, #10957 ) ) ;
#32324 = CARTESIAN_POINT ( 'NONE',  ( 54.94550656002158462, -5.360552262008241975, -3.995336669076017255 ) ) ;
#32326 = VERTEX_POINT ( 'NONE', #12550 ) ;
#32327 = CARTESIAN_POINT ( 'NONE',  ( 5.377543748152549874, 5.151476664237558900, -6.139290821770204687 ) ) ;
#32328 = DIRECTION ( 'NONE',  ( -0.000000000000000000, -0.000000000000000000, 1.000000000000000000 ) ) ;
#32330 = ORIENTED_EDGE ( 'NONE', *, *, #10311, .T. ) ;
#32329 = CARTESIAN_POINT ( 'NONE',  ( 25.75999999999999801, 2.769709385801040646, 1.244424427642012221 ) ) ;
#32331 = CARTESIAN_POINT ( 'NONE',  ( 26.04661131027748056, 19.53168319095744465, -1.500000000000000000 ) ) ;
#32332 = CARTESIAN_POINT ( 'NONE',  ( 22.54750000000000654, -2.594547506269383685, -0.7685399846772043020 ) ) ;
#32333 = PLANE ( 'NONE',  #26264 ) ;
#32334 = DIRECTION ( 'NONE',  ( 1.000000000000000000, -8.574039729943018344E-17, -0.000000000000000000 ) ) ;
#32336 = VERTEX_POINT ( 'NONE', #2531 ) ;
#32335 = CARTESIAN_POINT ( 'NONE',  ( 107.4894986256252594, -17.93307083222387632, -5.107540108678854551 ) ) ;
#32337 = CARTESIAN_POINT ( 'NONE',  ( -23.35000000000000142, -10.96966150227469505, -1.499999999999999556 ) ) ;
#32338 = DIRECTION ( 'NONE',  ( -1.000000000000000000, 8.574039729943022041E-17, 6.162975822039154730E-33 ) ) ;
#32339 = FACE_OUTER_BOUND ( 'NONE', #12620, .T. ) ;
#32340 = EDGE_CURVE ( 'NONE', #6932, #12461, #2685, .T. ) ;
#32341 = DIRECTION ( 'NONE',  ( 0.000000000000000000, 0.000000000000000000, -1.000000000000000000 ) ) ;
#32342 = CARTESIAN_POINT ( 'NONE',  ( 0.3076690219754980582, -6.806638167515089322, 7.713510465969206642 ) ) ;
#32343 = ORIENTED_EDGE ( 'NONE', *, *, #23865, .T. ) ;
#32344 = CARTESIAN_POINT ( 'NONE',  ( -16.96515769256209794, -28.43932300454936879, 11.09540449768827131 ) ) ;
#32345 = B_SPLINE_CURVE_WITH_KNOTS ( 'NONE', 3,
 ( #1490, #11666, #24710, #1839, #12019, #22213, #32578, #32422 ),
 .UNSPECIFIED., .F., .F.,
 ( 4, 2, 2, 4 ),
 ( 2.304311362529371911E-07, 0.001261163669367343495, 0.001891630288482890618, 0.002522096907598437958 ),
 .UNSPECIFIED. ) ;
#32346 = CARTESIAN_POINT ( 'NONE',  ( 10.00000000000000000, -3.641590349731909537, -3.055657119358837992 ) ) ;
#32347 = VERTEX_POINT ( 'NONE', #27933 ) ;
#32348 = CARTESIAN_POINT ( 'NONE',  ( -50.81000000000000227, -10.96999999999998643, 1.500000000000000000 ) ) ;
#32349 = CARTESIAN_POINT ( 'NONE',  ( 3.583596913636406533, -0.01388667853607431120, -1.134179515492645729 ) ) ;
#32350 = ORIENTED_EDGE ( 'NONE', *, *, #7994, .F. ) ;
#32351 = CARTESIAN_POINT ( 'NONE',  ( 7.622999046548425639, -3.997048926087008791, 1.000000000000000000 ) ) ;
#32352 = ORIENTED_EDGE ( 'NONE', *, *, #15986, .T. ) ;
#32353 = EDGE_CURVE ( 'NONE', #19944, #20824, #23579, .T. ) ;
#32354 = EDGE_LOOP ( 'NONE', ( #15741, #29826, #485, #32093 ) ) ;
#32355 = PLANE ( 'NONE',  #16654 ) ;
#32356 = DATE_AND_TIME ( #24137, #2961 ) ;
#32358 = ORIENTED_EDGE ( 'NONE', *, *, #16629, .F. ) ;
#32357 = CARTESIAN_POINT ( 'NONE',  ( 18.06290729145370477, -21.14813556147819540, -1.751201132231419377 ) ) ;
#32359 = ORIENTED_EDGE ( 'NONE', *, *, #30794, .F. ) ;
#32360 = CARTESIAN_POINT ( 'NONE',  ( 22.67250000136559507, 2.363507492473148286, 1.913930629741525058 ) ) ;
#32361 = B_SPLINE_CURVE_WITH_KNOTS ( 'NONE', 3,
 ( #16841, #16667, #24689, #29878, #14478, #1818, #30063, #4299, #3994, #19683 ),
 .UNSPECIFIED., .F., .F.,
 ( 4, 2, 2, 2, 4 ),
 ( 1.968338519010778477E-07, 0.0005467930078056964724, 0.001093389181759491739, 0.001639985355713287222, 0.002186581529667082704 ),
 .UNSPECIFIED. ) ;
#32362 = ORIENTED_EDGE ( 'NONE', *, *, #29972, .F. ) ;
#32363 = LINE ( 'NONE', #9423, #24094 ) ;
#32364 = CARTESIAN_POINT ( 'NONE',  ( -8.000050800000000351, 0.000000000000000000, 0.000000000000000000 ) ) ;
#32366 = VERTEX_POINT ( 'NONE', #22753 ) ;
#32365 = CARTESIAN_POINT ( 'NONE',  ( 18.97818541978548268, -3.421065958672000917, -1.873789191074026306 ) ) ;
#32367 = CARTESIAN_POINT ( 'NONE',  ( 34.48223484310469900, 0.000000000000000000, 2.482234843104950350 ) ) ;
#32368 = CARTESIAN_POINT ( 'NONE',  ( 26.50087866478441256, 17.58784721092446190, 0.4463807625373157340 ) ) ;
#32369 = CARTESIAN_POINT ( 'NONE',  ( 5.612974044843316968, 1.229732182294900555, 8.123783100924550027 ) ) ;
#32370 = CARTESIAN_POINT ( 'NONE',  ( 23.36000000136559507, 0.9349337715887185984, -3.156283516753368268 ) ) ;
#32371 = CARTESIAN_POINT ( 'NONE',  ( 108.0597073579234149, -18.92913321739387200, 4.563813387248837117 ) ) ;
#32372 = EDGE_CURVE ( 'NONE', #29650, #2323, #15185, .T. ) ;
#32373 = ADVANCED_FACE ( 'NONE', ( #20412 ), #15221, .T. ) ;
#32374 = CARTESIAN_POINT ( 'NONE',  ( 0.7294883270164040923, -11.94795532514583591, -5.485967528433937979 ) ) ;
#32375 = LINE ( 'NONE', #7416, #22506 ) ;
#32376 = CARTESIAN_POINT ( 'NONE',  ( 25.20116447083525557, -17.53130488828757549, 1.247823832778429898 ) ) ;
#32377 = CARTESIAN_POINT ( 'NONE',  ( -38.14293509397970183, 21.49000000000000199, 1.050000000000000044 ) ) ;
#32378 = CARTESIAN_POINT ( 'NONE',  ( 3.608283490412365891E-16, 4.208382051008230818, -2.718385644597129502 ) ) ;
#32379 = CARTESIAN_POINT ( 'NONE',  ( 24.72695737054825926, 18.91229966141139229, -1.500000000000000000 ) ) ;
#32380 = CARTESIAN_POINT ( 'NONE',  ( 0.3076688774120017178, -2.239519426673731939, -10.04057401065164612 ) ) ;
#32381 = CARTESIAN_POINT ( 'NONE',  ( -4.500050802731188071, 1.549418761218566143, -2.853674364686379583 ) ) ;
#32382 = ORIENTED_EDGE ( 'NONE', *, *, #11145, .F. ) ;
#32383 = CARTESIAN_POINT ( 'NONE',  ( -3.750050800000001239, -0.9222479816126459840, -3.113457007523259268 ) ) ;
#32384 = DIRECTION ( 'NONE',  ( -1.000000000000000000, 0.000000000000000000, 0.000000000000000000 ) ) ;
#32385 = DIRECTION ( 'NONE',  ( -7.472768010112085392E-18, -0.08715574274766894891, 0.9961946980917446570 ) ) ;
#32386 = EDGE_LOOP ( 'NONE', ( #24145, #12839 ) ) ;
#32387 = CARTESIAN_POINT ( 'NONE',  ( 3.499999999999999556, 4.438567988583181467, -7.249076783337631724 ) ) ;
#32388 = CARTESIAN_POINT ( 'NONE',  ( 7.611844841314722387, -2.453950335954110162, -1.500000000000000222 ) ) ;
#32389 = ORIENTED_EDGE ( 'NONE', *, *, #6089, .F. ) ;
#32390 = CARTESIAN_POINT ( 'NONE',  ( 2.425585535373192325, 9.314797388894900720, 5.239665997526921970 ) ) ;
#32391 = PERSON_AND_ORGANIZATION ( #6766, #25292 ) ;
#32392 = CARTESIAN_POINT ( 'NONE',  ( -50.60000000000000142, -21.43932300454937945, -1.000000000000000000 ) ) ;
#32393 = VERTEX_POINT ( 'NONE', #18057 ) ;
#32394 = CARTESIAN_POINT ( 'NONE',  ( 8.528645601772334217, -0.5000000000000000000, -1.500000000000000000 ) ) ;
#32395 = CARTESIAN_POINT ( 'NONE',  ( 13.24625820531402631, 6.653948736490935545, -1.050000000000000044 ) ) ;
#32396 = CARTESIAN_POINT ( 'NONE',  ( 8.930755659325141593, 0.5000000000000086597, -1.500000000000000000 ) ) ;
#32397 = CARTESIAN_POINT ( 'NONE',  ( 6.357667697713671018, -2.056386458247330129, 8.357963647880069402 ) ) ;
#32398 = CYLINDRICAL_SURFACE ( 'NONE', #18708, 2.999999999999999112 ) ;
#32399 = ORIENTED_EDGE ( 'NONE', *, *, #25996, .T. ) ;
#32400 = EDGE_CURVE ( 'NONE', #660, #5275, #16133, .T. ) ;
#32401 = CARTESIAN_POINT ( 'NONE',  ( 23.27353278736380204, -21.94187821002792660, -1.000000000000000000 ) ) ;
#32402 = CARTESIAN_POINT ( 'NONE',  ( 56.97280603064898941, -277.2763395528616002, 4.629213727441584325 ) ) ;
#32403 = DIRECTION ( 'NONE',  ( 1.000000000000000000, -0.000000000000000000, -0.000000000000000000 ) ) ;
#32404 = EDGE_CURVE ( 'NONE', #25815, #32480, #13971, .T. ) ;
#32406 = ORIENTED_EDGE ( 'NONE', *, *, #4395, .T. ) ;
#32405 = CARTESIAN_POINT ( 'NONE',  ( -4.290242492657217039E-16, -5.003758587302148619, -0.2500000000000008882 ) ) ;
#32407 = CARTESIAN_POINT ( 'NONE',  ( 34.99999999999998579, 0.000000000000000000, 3.000000000000239364 ) ) ;
#32408 = CARTESIAN_POINT ( 'NONE',  ( 25.91108971418529805, 23.29498995882582335, -2.334455007174283558 ) ) ;
#32409 = CARTESIAN_POINT ( 'NONE',  ( 5.887530180601099339, -3.870837198608047203, -7.449245365665835727 ) ) ;
#32410 = CARTESIAN_POINT ( 'NONE',  ( 108.5692966685781755, 15.69075386566562713, 1.106576256426021532 ) ) ;
#32411 = FACE_OUTER_BOUND ( 'NONE', #509, .T. ) ;
#32412 = DIRECTION ( 'NONE',  ( 7.770718973609021797E-17, 0.9063077870366551547, -0.4226182617406882280 ) ) ;
#32413 = DIRECTION ( 'NONE',  ( 6.062761635205589313E-17, 0.7071067811865484609, -0.7071067811865465735 ) ) ;
#32414 = DIRECTION ( 'NONE',  ( 7.770718973608935516E-17, 0.9063077870366456068, 0.4226182617407089337 ) ) ;
#32415 = DIRECTION ( 'NONE',  ( 1.000000000000000000, -8.574039729943018344E-17, -0.000000000000000000 ) ) ;
#32416 = EDGE_LOOP ( 'NONE', ( #13200, #17633, #7291, #6494 ) ) ;
#32417 = CARTESIAN_POINT ( 'NONE',  ( 10.00000000000000000, 4.467071865485470639, 1.625881193364712596 ) ) ;
#32418 = ORIENTED_EDGE ( 'NONE', *, *, #20622, .F. ) ;
#32419 = CARTESIAN_POINT ( 'NONE',  ( -6.954531657079158435, -0.9198621039125872700, -3.105402419394638791 ) ) ;
#32420 = DIRECTION ( 'NONE',  ( -1.000000000000000000, 0.000000000000000000, 0.000000000000000000 ) ) ;
#32421 = PLANE ( 'NONE',  #22086 ) ;
#32422 = CARTESIAN_POINT ( 'NONE',  ( 2.274274201625327230, 9.680994141368847394, -5.222868219166750592 ) ) ;
#32423 = DIRECTION ( 'NONE',  ( 0.000000000000000000, -1.000000000000000000, 0.000000000000000000 ) ) ;
#32424 = VERTEX_POINT ( 'NONE', #25576 ) ;
#32425 = CARTESIAN_POINT ( 'NONE',  ( -59.58387603396901966, -5.539140460716925674, 5.221328934740562033 ) ) ;
#32426 = EDGE_CURVE ( 'NONE', #24269, #25473, #24674, .T. ) ;
#32427 = EDGE_LOOP ( 'NONE', ( #26062, #32546, #9627, #3508 ) ) ;
#32428 = CALENDAR_DATE ( 2026, 6, 10 ) ;
#32429 = CARTESIAN_POINT ( 'NONE',  ( 40.88396986210033646, -6.892597666169408832, 3.999773184966937567 ) ) ;
#32430 = EDGE_CURVE ( 'NONE', #7224, #13047, #8666, .T. ) ;
#32431 = DIRECTION ( 'NONE',  ( 0.4999999999999977796, 0.8660254037844398178, 0.000000000000000000 ) ) ;
#32433 = CARTESIAN_POINT ( 'NONE',  ( 10.52034268205830614, 3.055657119358800244, 3.641590349731939735 ) ) ;
#32432 = DIRECTION ( 'NONE',  ( 1.000000000000000000, -8.574039729943018344E-17, -0.000000000000000000 ) ) ;
#32434 = EDGE_LOOP ( 'NONE', ( #21640, #20109, #17043, #28704 ) ) ;
#32435 = FACE_OUTER_BOUND ( 'NONE', #30792, .T. ) ;
#32436 = CARTESIAN_POINT ( 'NONE',  ( 5.612718761614564400, -7.212912035758782814, -3.934162523501308684 ) ) ;
#32437 = EDGE_CURVE ( 'NONE', #17424, #8184, #10029, .T. ) ;
#32438 = CARTESIAN_POINT ( 'NONE',  ( 25.23499999999999943, 0.2613211581691317065, 2.486304738420681559 ) ) ;
#32439 = B_SPLINE_CURVE_WITH_KNOTS ( 'NONE', 3,
 ( #7959, #23495, #21173, #30889, #20686, #10971, #16135, #23001 ),
 .UNSPECIFIED., .F., .F.,
 ( 4, 2, 2, 4 ),
 ( 5.099451029784175022E-07, 0.001229189612685845740, 0.001843529446477279411, 0.002457869280268713298 ),
 .UNSPECIFIED. ) ;
#32440 = CARTESIAN_POINT ( 'NONE',  ( 0.1361373023263046378, -7.043147518533485751, -1.774498076833521898 ) ) ;
#32442 = EDGE_LOOP ( 'NONE', ( #25471, #12103, #20755, #26533, #1529 ) ) ;
#32441 = CARTESIAN_POINT ( 'NONE',  ( -15.02135460118491217, -25.93932300454937945, 1.095404497688272638 ) ) ;
#32443 = CARTESIAN_POINT ( 'NONE',  ( -2.237550801365593589, 1.088641768524161613, 3.675193018007247403 ) ) ;
#32444 = CARTESIAN_POINT ( 'NONE',  ( 10.00000000000000178, 4.616489984850531414, 1.946309384392610031 ) ) ;
#32445 = EDGE_CURVE ( 'NONE', #31825, #25210, #29514, .T. ) ;
#32446 = CARTESIAN_POINT ( 'NONE',  ( 10.00000000000000178, -8.574039729943018837E-16, 0.000000000000000000 ) ) ;
#32447 = ORIENTED_EDGE ( 'NONE', *, *, #2729, .T. ) ;
#32449 = EDGE_LOOP ( 'NONE', ( #31769, #21175, #30451, #15459 ) ) ;
#32448 = CARTESIAN_POINT ( 'NONE',  ( 13.28821369005689945, 21.83086517065485666, 1.350282695622831319 ) ) ;
#32450 =( BOUNDED_SURFACE ( )  B_SPLINE_SURFACE ( 3, 3, ( 
 ( #32759, #29898, #1837, #32270, #17363, #9330, #1489, #19542 ),
 ( #9147, #6977, #19874, #4006, #27557, #17184, #6666, #14679 ),
 ( #24880, #14827, #1991, #12164, #25026, #2141, #12321, #24373 ),
 ( #22542, #9836, #20052, #6485, #26899, #14173, #29582, #11665 ) ),
 .UNSPECIFIED., .F., .F., .T. ) 
 B_SPLINE_SURFACE_WITH_KNOTS ( ( 4, 4 ),
 ( 4, 2, 2, 4 ),
 ( 0.000000000000000000, 1.000000000000000000 ),
 ( 0.000000000000000000, 0.5000000000000000000, 0.7500000000000000000, 1.000000000000000000 ),
 .UNSPECIFIED. ) 
 GEOMETRIC_REPRESENTATION_ITEM ( )  RATIONAL_B_SPLINE_SURFACE ( (
 ( 1.000000000000000000, 1.000000000000000000, 1.000000000000000000, 1.000000000000000000, 1.000000000000000000, 1.000000000000000000, 1.000000000000000000, 1.000000000000000000),
 ( 0.6857970438836928917, 0.6857970438836928917, 0.6857970438836928917, 0.6857970438836928917, 0.6857970438836928917, 0.6857970438836928917, 0.6857970438836928917, 0.6857970438836928917),
 ( 0.6857970438836928917, 0.6857970438836928917, 0.6857970438836928917, 0.6857970438836928917, 0.6857970438836928917, 0.6857970438836928917, 0.6857970438836928917, 0.6857970438836928917),
 ( 1.000000000000000000, 1.000000000000000000, 1.000000000000000000, 1.000000000000000000, 1.000000000000000000, 1.000000000000000000, 1.000000000000000000, 1.000000000000000000) ) ) 
 REPRESENTATION_ITEM ( '' )  SURFACE ( )  );
#32451 = CARTESIAN_POINT ( 'NONE',  ( 107.4160271293911251, 17.73379232341987333, 4.360465883803716913 ) ) ;
#32452 = DIRECTION ( 'NONE',  ( -1.000000000000000000, 8.574039729943017111E-17, -0.000000000000000000 ) ) ;
#32453 = EDGE_CURVE ( 'NONE', #4554, #469, #17402, .T. ) ;
#32454 = CARTESIAN_POINT ( 'NONE',  ( 0.000000000000000000, 6.478011392632983423, -6.807171995660517005 ) ) ;
#32455 = FACE_OUTER_BOUND ( 'NONE', #27090, .T. ) ;
#32456 = CARTESIAN_POINT ( 'NONE',  ( 8.152039755618655903, -19.35439874310824848, -1.499999999999998668 ) ) ;
#32457 = CARTESIAN_POINT ( 'NONE',  ( 5.377543748152548098, 6.940565734314597002, 4.007137495034836405 ) ) ;
#32458 = EDGE_CURVE ( 'NONE', #23049, #9305, #9741, .T. ) ;
#32459 = CARTESIAN_POINT ( 'NONE',  ( 84.87411226249194840, -2.587501188395394003, 1.529339190611904264 ) ) ;
#32460 = CARTESIAN_POINT ( 'NONE',  ( 107.6149215477164347, -15.92400613423468414, 1.487010776595586670 ) ) ;
#32461 = VERTEX_POINT ( 'NONE', #9878 ) ;
#32462 = CARTESIAN_POINT ( 'NONE',  ( 85.49734435724778336, -7.913007294147514692, -0.07017451552783579571 ) ) ;
#32463 = ORIENTED_EDGE ( 'NONE', *, *, #24039, .F. ) ;
#32464 = CARTESIAN_POINT ( 'NONE',  ( 21.39621122230731487, -21.77804412735446959, 1.397661460514373122 ) ) ;
#32465 = EDGE_CURVE ( 'NONE', #11793, #27801, #15622, .T. ) ;
#32466 = DIRECTION ( 'NONE',  ( 0.000000000000000000, 0.000000000000000000, 1.000000000000000000 ) ) ;
#32467 = LINE ( 'NONE', #17407, #16579 ) ;
#32468 = VERTEX_POINT ( 'NONE', #3527 ) ;
#32469 = CARTESIAN_POINT ( 'NONE',  ( -4.290242492657217039E-16, -5.003758587302148619, 0.2499999999999991951 ) ) ;
#32470 = VERTEX_POINT ( 'NONE', #3035 ) ;
#32471 = CARTESIAN_POINT ( 'NONE',  ( -23.54713438637982748, 3.520075575296777171, 2.000000000000000000 ) ) ;
#32473 = ORIENTED_EDGE ( 'NONE', *, *, #33060, .T. ) ;
#32472 = CARTESIAN_POINT ( 'NONE',  ( 102.3440911088257792, -2.856485598251504499, -3.995970699071413446 ) ) ;
#32474 = ORIENTED_EDGE ( 'NONE', *, *, #4547, .T. ) ;
#32475 = ADVANCED_FACE ( 'NONE', ( #13342 ), #11176, .T. ) ;
#32476 = EDGE_CURVE ( 'NONE', #22878, #29891, #31948, .T. ) ;
#32477 = DIRECTION ( 'NONE',  ( -0.000000000000000000, -0.000000000000000000, -1.000000000000000000 ) ) ;
#32478 = CARTESIAN_POINT ( 'NONE',  ( 69.09268213438589612, -2.232183665269758421, 1.010822989962091301 ) ) ;
#32480 = VERTEX_POINT ( 'NONE', #3358 ) ;
#32479 = CARTESIAN_POINT ( 'NONE',  ( 15.88617735125738584, -21.20699763342221900, -1.500000000000000222 ) ) ;
#32481 = DIRECTION ( 'NONE',  ( 1.000000000000000000, -8.574039729943018344E-17, -0.000000000000000000 ) ) ;
#32482 = CARTESIAN_POINT ( 'NONE',  ( 10.55147673363119232, -4.116875700062100130, 2.376879293651050329 ) ) ;
#32483 = DIRECTION ( 'NONE',  ( 0.000000000000000000, -0.9510565162951504226, -0.3090169943749573322 ) ) ;
#32484 = CARTESIAN_POINT ( 'NONE',  ( 7.461135470892884314, -4.560857689778476498, -1.000000000000000000 ) ) ;
#32485 = ADVANCED_FACE ( 'NONE', ( #11027 ), #28423, .T. ) ;
#32487 = ORIENTED_EDGE ( 'NONE', *, *, #15727, .F. ) ;
#32486 = CARTESIAN_POINT ( 'NONE',  ( 107.9815267783868649, -17.80335232094880382, -4.374195006133829722 ) ) ;
#32488 = CARTESIAN_POINT ( 'NONE',  ( 2.274274201625327230, -1.464956435139465496, -10.90201369670500142 ) ) ;
#32489 = DIRECTION ( 'NONE',  ( 0.000000000000000000, 0.08715574274765135188, 0.9961946980917461003 ) ) ;
#32490 = CARTESIAN_POINT ( 'NONE',  ( 24.17250000136559507, -2.363507492473152283, -1.913930629741525280 ) ) ;
#32491 = DIRECTION ( 'NONE',  ( -1.000000000000000000, 0.000000000000000000, 0.000000000000000000 ) ) ;
#32492 = EDGE_CURVE ( 'NONE', #32878, #12355, #4415, .T. ) ;
#32493 = CARTESIAN_POINT ( 'NONE',  ( -31.85000000000000497, -10.96966150227469505, 4.000000000000000000 ) ) ;
#32494 = CARTESIAN_POINT ( 'NONE',  ( 0.6708088701982989344, 0.000000000000000000, 4.629213727441584325 ) ) ;
#32495 = ORIENTED_EDGE ( 'NONE', *, *, #29109, .F. ) ;
#32496 = LINE ( 'NONE', #5076, #13992 ) ;
#32497 = CYLINDRICAL_SURFACE ( 'NONE', #9164, 0.5000000000000002220 ) ;
#32498 = CARTESIAN_POINT ( 'NONE',  ( -5.437550801365593323, 1.088641768524161613, 3.675193018007246959 ) ) ;
#32499 = VERTEX_POINT ( 'NONE', #13524 ) ;
#32500 = ADVANCED_FACE ( 'NONE', ( #6175 ), #8015, .T. ) ;
#32501 = B_SPLINE_CURVE_WITH_KNOTS ( 'NONE', 3,
 ( #15703, #973, #18381, #28880 ),
 .UNSPECIFIED., .F., .F.,
 ( 4, 4 ),
 ( -7.558714219364254830E-06, 0.0001212692848185989160 ),
 .UNSPECIFIED. ) ;
#32502 = FACE_BOUND ( 'NONE', #13322, .T. ) ;
#32503 = CARTESIAN_POINT ( 'NONE',  ( 12.57238041616097313, -15.42470150510370708, -0.9788672205888330202 ) ) ;
#32504 = VERTEX_POINT ( 'NONE', #18701 ) ;
#32505 = DIRECTION ( 'NONE',  ( 0.000000000000000000, 0.000000000000000000, -1.000000000000000000 ) ) ;
#32506 = ORIENTED_EDGE ( 'NONE', *, *, #4870, .F. ) ;
#32507 = ORIENTED_EDGE ( 'NONE', *, *, #6263, .T. ) ;
#32508 = LINE ( 'NONE', #16941, #6521 ) ;
#32510 = ORIENTED_EDGE ( 'NONE', *, *, #22335, .T. ) ;
#32509 = CARTESIAN_POINT ( 'NONE',  ( 21.20754276729296706, -21.72113672149313857, -1.466027919133052304 ) ) ;
#32511 = ORIENTED_EDGE ( 'NONE', *, *, #11185, .F. ) ;
#32512 = CARTESIAN_POINT ( 'NONE',  ( 22.42250000136559507, 1.913930629741522838, -2.363507492473150062 ) ) ;
#32513 = EDGE_CURVE ( 'NONE', #25887, #7812, #17738, .T. ) ;
#32514 = ADVANCED_FACE ( 'NONE', ( #18401 ), #17220, .T. ) ;
#32515 = VERTEX_POINT ( 'NONE', #10865 ) ;
#32516 = CYLINDRICAL_SURFACE ( 'NONE', #1241, 3.000000000000000444 ) ;
#32518 = ORIENTED_EDGE ( 'NONE', *, *, #25791, .F. ) ;
#32517 = CARTESIAN_POINT ( 'NONE',  ( 84.89549059758259375, -2.934676561234151659, -2.184955970506606171 ) ) ;
#32519 = LINE ( 'NONE', #22659, #11712 ) ;
#32520 = CARTESIAN_POINT ( 'NONE',  ( 4.013969549054183686E-16, 4.681538312723517059, 0.8254815157535410064 ) ) ;
#32521 = CARTESIAN_POINT ( 'NONE',  ( 25.17250000136559507, -2.363507492473152283, -1.913930629741525280 ) ) ;
#32522 = CARTESIAN_POINT ( 'NONE',  ( 101.7221769401408551, -2.897900707893039662, 3.993434276071444078 ) ) ;
#32523 = CARTESIAN_POINT ( 'NONE',  ( 13.65718777918027271, -19.09288791508984318, -4.522129901861166701 ) ) ;
#32524 = CARTESIAN_POINT ( 'NONE',  ( 107.3822631068044871, -16.38429022892981024, -2.521216264004209506 ) ) ;
#32525 = CARTESIAN_POINT ( 'NONE',  ( 25.38273381070388979, -17.54867692718855920, 1.149837904939749800 ) ) ;
#32526 = EDGE_CURVE ( 'NONE', #12740, #2610, #20893, .T. ) ;
#32527 = DIRECTION ( 'NONE',  ( 0.1437473352844943209, 0.000000000000000000, -0.9896144216807913896 ) ) ;
#32528 = CARTESIAN_POINT ( 'NONE',  ( 17.49368528859141847, -18.49828807951654497, 5.485967528433933538 ) ) ;
#32529 = CC_DESIGN_PERSON_AND_ORGANIZATION_ASSIGNMENT ( #1310, #19669, ( #2068 ) ) ;
#32530 = CARTESIAN_POINT ( 'NONE',  ( 10.00000000000000178, -0.2500000000000201505, 5.003758587302149508 ) ) ;
#32531 = CARTESIAN_POINT ( 'NONE',  ( 101.6022419886208468, -1.170867242066748304, 0.02339150516273448555 ) ) ;
#32532 = FACE_OUTER_BOUND ( 'NONE', #6037, .T. ) ;
#32533 = CARTESIAN_POINT ( 'NONE',  ( -7.050050802731187893, -1.887961173149512062, -2.331437884370912261 ) ) ;
#32534 = EDGE_LOOP ( 'NONE', ( #8597, #29555, #30844, #22655 ) ) ;
#32535 = CARTESIAN_POINT ( 'NONE',  ( -2.600050800000000883, 1.887961173149511618, 2.331437884370912705 ) ) ;
#32536 = DIRECTION ( 'NONE',  ( -1.000000000000000000, -1.369475477426764022E-16, 0.000000000000000000 ) ) ;
#32537 = CARTESIAN_POINT ( 'NONE',  ( 18.58227844715246135, -7.846511338401735536, 2.713652344655544724 ) ) ;
#32538 = VERTEX_POINT ( 'NONE', #5831 ) ;
#32539 = DIRECTION ( 'NONE',  ( -1.000000000000000000, 0.000000000000000000, -0.000000000000000000 ) ) ;
#32540 = EDGE_CURVE ( 'NONE', #31286, #29792, #1617, .T. ) ;
#32541 = VERTEX_POINT ( 'NONE', #16015 ) ;
#32542 = CARTESIAN_POINT ( 'NONE',  ( 3.063284526839887167, 7.360373001730918574, 4.729683950898899703 ) ) ;
#32543 = ADVANCED_FACE ( 'NONE', ( #13828 ), #23092, .T. ) ;
#32544 = CALENDAR_DATE ( 2026, 6, 10 ) ;
#32545 = CARTESIAN_POINT ( 'NONE',  ( 4.183205650141505458E-16, -1.999317321091424793, -10.76487093102067050 ) ) ;
#32546 = ORIENTED_EDGE ( 'NONE', *, *, #7944, .T. ) ;
#32547 = DIRECTION ( 'NONE',  ( -1.000000000000000000, 0.000000000000000000, -8.654346879536960414E-15 ) ) ;
#32548 = ORIENTED_EDGE ( 'NONE', *, *, #9409, .F. ) ;
#32549 = VECTOR ( 'NONE', #29645, 1000.000000000000000 ) ;
#32550 = DIRECTION ( 'NONE',  ( 0.000000000000000000, 0.000000000000000000, 1.000000000000000000 ) ) ;
#32551 = CARTESIAN_POINT ( 'NONE',  ( 40.88276903863778955, -6.671230418080579483, -4.215290092883790862 ) ) ;
#32552 = CARTESIAN_POINT ( 'NONE',  ( 7.249760686538667009, -3.647351267791625773, 7.953573330858203505 ) ) ;
#32553 = CYLINDRICAL_SURFACE ( 'NONE', #29939, 11.00000000000000000 ) ;
#32554 = VERTEX_POINT ( 'NONE', #11356 ) ;
#32555 = CARTESIAN_POINT ( 'NONE',  ( 22.46520446472753463, -21.85309543850499736, -1.407654187663929024 ) ) ;
#32556 = CARTESIAN_POINT ( 'NONE',  ( 101.7323081545095107, -3.043787674472451688, 4.171847251016090219 ) ) ;
#32557 = B_SPLINE_CURVE_WITH_KNOTS ( 'NONE', 3,
 ( #22479, #17802, #5106, #14626, #9589, #9433, #14934, #12759 ),
 .UNSPECIFIED., .F., .F.,
 ( 4, 2, 2, 4 ),
 ( 2.737843117574031781E-07, 0.001228034957219863513, 0.001841915543673915958, 0.002455796130127969705 ),
 .UNSPECIFIED. ) ;
#32559 = ORIENTED_EDGE ( 'NONE', *, *, #22373, .T. ) ;
#32558 = DIRECTION ( 'NONE',  ( -1.000000000000000000, 0.000000000000000000, 0.000000000000000000 ) ) ;
#32560 = CARTESIAN_POINT ( 'NONE',  ( 0.000000000000000000, 0.000000000000000000, 0.000000000000000000 ) ) ;
#32561 = DIRECTION ( 'NONE',  ( 0.000000000000000000, 0.000000000000000000, -1.000000000000000000 ) ) ;
#32562 = CARTESIAN_POINT ( 'NONE',  ( 7.064632940817597628, -3.748318449932240615, -7.906491560603705615 ) ) ;
#32563 = CARTESIAN_POINT ( 'NONE',  ( 110.8079127523828618, 15.75827621748124940, -1.491740999229419273 ) ) ;
#32564 = DIRECTION ( 'NONE',  ( 0.000000000000000000, 1.000000000000000000, 0.000000000000000000 ) ) ;
#32565 = AXIS2_PLACEMENT_3D ( 'NONE', #32883, #2283, #7130 ) ;
#32566 = CARTESIAN_POINT ( 'NONE',  ( -8.000050800000000351, 3.202524238648755350, 1.313925200161312423 ) ) ;
#32567 = CARTESIAN_POINT ( 'NONE',  ( 25.25173065115962245, -17.50931434788435936, -1.141336708623620577 ) ) ;
#32568 = CARTESIAN_POINT ( 'NONE',  ( 24.17250000273118715, 2.378061970571979433, -1.291182301015470602 ) ) ;
#32569 = CARTESIAN_POINT ( 'NONE',  ( 23.19643008672779771, -21.93767770566448050, 1.043375197815962885 ) ) ;
#32570 = VECTOR ( 'NONE', #12665, 1000.000000000000000 ) ;
#32571 = ORIENTED_EDGE ( 'NONE', *, *, #10196, .T. ) ;
#32572 = MANIFOLD_SOLID_BREP ( 'Fillet1', #7073 ) ;
#32573 = CARTESIAN_POINT ( 'NONE',  ( 0.000000000000000000, 9.680994141368771011, 5.222868219166891812 ) ) ;
#32574 = ORIENTED_EDGE ( 'NONE', *, *, #24435, .T. ) ;
#32575 = CARTESIAN_POINT ( 'NONE',  ( -7.254531657079158258, -1.545410377633946286, 2.846291840500174697 ) ) ;
#32576 = DIRECTION ( 'NONE',  ( 0.000000000000000000, -0.9961946980917467664, 0.08715574274764384399 ) ) ;
#32577 = CARTESIAN_POINT ( 'NONE',  ( -8.000050800000000351, 0.000000000000000000, 0.000000000000000000 ) ) ;
#32578 = CARTESIAN_POINT ( 'NONE',  ( 2.357330042320761265, 9.485534025193874896, -5.240837896778860916 ) ) ;
#32579 = PLANE ( 'NONE',  #8202 ) ;
#32580 = ORIENTED_EDGE ( 'NONE', *, *, #27448, .F. ) ;
#32581 = EDGE_CURVE ( 'NONE', #436, #21704, #9595, .T. ) ;
#32582 = DIRECTION ( 'NONE',  ( 0.000000000000000000, 0.000000000000000000, 1.000000000000000000 ) ) ;
#32583 = ADVANCED_FACE ( 'NONE', ( #6822 ), #8842, .F. ) ;
#32584 = VERTEX_POINT ( 'NONE', #4325 ) ;
#32585 = ADVANCED_FACE ( 'NONE', ( #1842 ), #16693, .T. ) ;
#32586 = PERSON_AND_ORGANIZATION_ROLE ( 'design_owner' ) ;
#32587 = CARTESIAN_POINT ( 'NONE',  ( 85.03560246333768191, -5.201294972509532322, 3.998505472958077345 ) ) ;
#32588 = AXIS2_PLACEMENT_3D ( 'NONE', #8649, #18870, #29069 ) ;
#32589 = LINE ( 'NONE', #22726, #31014 ) ;
#32590 = VECTOR ( 'NONE', #5460, 1000.000000000000000 ) ;
#32592 = LINE ( 'NONE', #9664, #4913 ) ;
#32591 = CARTESIAN_POINT ( 'NONE',  ( 5.885541806331895387, 7.447669719165333824, 3.871259391815477624 ) ) ;
#32593 = EDGE_LOOP ( 'NONE', ( #27932, #29813, #12109 ) ) ;
#32594 = DIRECTION ( 'NONE',  ( 0.000000000000000000, 0.000000000000000000, -1.000000000000000000 ) ) ;
#32595 = CYLINDRICAL_SURFACE ( 'NONE', #26213, 3.000000000000000000 ) ;
#32596 = CARTESIAN_POINT ( 'NONE',  ( 21.48499999999999943, -2.486304738420683780, 0.2613211581691335383 ) ) ;
#32597 = CARTESIAN_POINT ( 'NONE',  ( 0.5878146867678383236, -8.555166304036935898, -1.500000000000070832 ) ) ;
#32598 = CIRCLE ( 'NONE', #10164, 12.00121908859764552 ) ;
#32600 = VERTEX_POINT ( 'NONE', #1344 ) ;
#32599 = CARTESIAN_POINT ( 'NONE',  ( 3.541509388326189001, -13.88765124358304170, 4.522129901861157819 ) ) ;
#32601 = CARTESIAN_POINT ( 'NONE',  ( -4.637550801365592612, 1.088641768524161613, 3.675193018007247403 ) ) ;
#32602 = LINE ( 'NONE', #6340, #19254 ) ;
#32603 = CARTESIAN_POINT ( 'NONE',  ( 2.589202797589354788, -10.26630467377260558, -1.003524335601144291 ) ) ;
#32604 = CARTESIAN_POINT ( 'NONE',  ( 22.04750000000000298, 2.594547506269380133, 0.7685399846772031918 ) ) ;
#32605 = ORIENTED_EDGE ( 'NONE', *, *, #9421, .F. ) ;
#32607 = EDGE_LOOP ( 'NONE', ( #9123, #19743, #11740 ) ) ;
#32606 = DIRECTION ( 'NONE',  ( 0.000000000000000000, -0.2079116908177663647, 0.9781476007338042455 ) ) ;
#32608 = CYLINDRICAL_SURFACE ( 'NONE', #18753, 6.000000000000000000 ) ;
#32609 = CARTESIAN_POINT ( 'NONE',  ( 6.530491482054473273, 8.398420403995373817, 2.114164693852618182 ) ) ;
#32610 = AXIS2_PLACEMENT_3D ( 'NONE', #29866, #22993, #20334 ) ;
#32611 = CARTESIAN_POINT ( 'NONE',  ( 25.54750000136559507, 1.913930629741522838, -2.363507492473150062 ) ) ;
#32612 = CIRCLE ( 'NONE', #28871, 10.19912342234043834 ) ;
#32613 = CARTESIAN_POINT ( 'NONE',  ( 3.020080181664722030, -3.262125172866642053, -8.342499971020046701 ) ) ;
#32614 = CARTESIAN_POINT ( 'NONE',  ( 14.48598712922800225, -20.94846587651628056, -1.499999999999997780 ) ) ;
#32615 = EDGE_CURVE ( 'NONE', #4162, #30798, #14684, .T. ) ;
#32616 = DIRECTION ( 'NONE',  ( -0.000000000000000000, 0.000000000000000000, -1.000000000000000000 ) ) ;
#32617 = VECTOR ( 'NONE', #12716, 1000.000000000000000 ) ;
#32618 = CARTESIAN_POINT ( 'NONE',  ( 102.2268587688196106, -1.179183864763504230, 0.8105616763793748181 ) ) ;
#32619 = CARTESIAN_POINT ( 'NONE',  ( 0.7632845268451400322, 6.772677083973724699, 5.538577986791671570 ) ) ;
#32620 = ORIENTED_EDGE ( 'NONE', *, *, #3629, .F. ) ;
#32621 = DIRECTION ( 'NONE',  ( 0.000000000000000000, 0.5877852522924689183, 0.8090169943749504489 ) ) ;
#32622 = ORIENTED_EDGE ( 'NONE', *, *, #6160, .T. ) ;
#32623 = AXIS2_PLACEMENT_3D ( 'NONE', #1535, #17248, #27450 ) ;
#32624 = LINE ( 'NONE', #9702, #31625 ) ;
#32625 = DIRECTION ( 'NONE',  ( 1.000000000000000000, 0.000000000000000000, 0.000000000000000000 ) ) ;
#32626 = DIRECTION ( 'NONE',  ( -1.000000000000000000, 0.000000000000000000, 0.000000000000000000 ) ) ;
#32627 = ORIENTED_EDGE ( 'NONE', *, *, #15001, .T. ) ;
#32628 = ORIENTED_EDGE ( 'NONE', *, *, #24325, .T. ) ;
#32629 = CARTESIAN_POINT ( 'NONE',  ( 2.795120610037678865, -9.728666380661900703, 0.7443816538093672719 ) ) ;
#32631 = ORIENTED_EDGE ( 'NONE', *, *, #28245, .F. ) ;
#32630 = CARTESIAN_POINT ( 'NONE',  ( 40.87778564756947475, -5.758464639511137406, -4.008636882573171967 ) ) ;
#32632 = AXIS2_PLACEMENT_3D ( 'NONE', #14702, #14342, #22234 ) ;
#32633 = ORIENTED_EDGE ( 'NONE', *, *, #27117, .F. ) ;
#32634 = VECTOR ( 'NONE', #31516, 1000.000000000000114 ) ;
#32635 = DIRECTION ( 'NONE',  ( 1.000000000000000000, 0.000000000000000000, 0.000000000000000000 ) ) ;
#32636 = CIRCLE ( 'NONE', #26746, 9.269952810656748809 ) ;
#32637 = CARTESIAN_POINT ( 'NONE',  ( 85.10544820215893935, -1.573551533646333711, 1.915219082070892531 ) ) ;
#32639 = ORIENTED_EDGE ( 'NONE', *, *, #24583, .T. ) ;
#32638 = DIRECTION ( 'NONE',  ( -1.000000000000000000, 0.000000000000000000, -0.000000000000000000 ) ) ;
#32640 = CARTESIAN_POINT ( 'NONE',  ( 6.356382399260308347, 4.790388219480560927, 7.150437133400945555 ) ) ;
#32641 = AXIS2_PLACEMENT_3D ( 'NONE', #18189, #15008, #2350 ) ;
#32642 = CARTESIAN_POINT ( 'NONE',  ( 8.900602013106571064, 0.09531162291654594887, -1.304562659182835871 ) ) ;
#32643 = CARTESIAN_POINT ( 'NONE',  ( -4.179200081765273467, -3.233695810519997327, 1.500000000000000000 ) ) ;
#32644 = DIRECTION ( 'NONE',  ( -1.000000000000000000, 0.000000000000000000, 0.000000000000000000 ) ) ;
#32646 = ORIENTED_EDGE ( 'NONE', *, *, #1821, .F. ) ;
#32645 = CARTESIAN_POINT ( 'NONE',  ( 107.4510233030913611, -17.37417541359246087, -4.558428962808153351 ) ) ;
#32647 = DIRECTION ( 'NONE',  ( 0.000000000000000000, 1.000000000000000000, 0.000000000000000000 ) ) ;
#32648 = AXIS2_PLACEMENT_3D ( 'NONE', #23821, #21646, #21308 ) ;
#32649 = ADVANCED_FACE ( 'NONE', ( #17010 ), #4161, .T. ) ;
#32650 = CARTESIAN_POINT ( 'NONE',  ( 6.357667873252800028, -2.398098878660900102, -8.266402141659465741 ) ) ;
#32651 = CARTESIAN_POINT ( 'NONE',  ( 24.98500000136559507, -2.892927487894331406, 1.570731468192932301 ) ) ;
#32652 = DIRECTION ( 'NONE',  ( -1.000000000000000000, 0.000000000000000000, 0.000000000000000000 ) ) ;
#32653 = DIRECTION ( 'NONE',  ( 1.000000000000000000, 0.000000000000000000, 0.000000000000000000 ) ) ;
#32654 = ORIENTED_EDGE ( 'NONE', *, *, #16049, .F. ) ;
#32655 = DIRECTION ( 'NONE',  ( -0.000000000000000000, -1.000000000000000000, 0.000000000000000000 ) ) ;
#32656 = AXIS2_PLACEMENT_3D ( 'NONE', #1032, #11557, #6060 ) ;
#32657 = EDGE_CURVE ( 'NONE', #21064, #12879, #28441, .T. ) ;
#32658 = DIRECTION ( 'NONE',  ( 0.000000000000000000, -0.8660254037844432595, 0.4999999999999918399 ) ) ;
#32659 = EDGE_CURVE ( 'NONE', #30204, #3232, #11519, .T. ) ;
#32660 = CARTESIAN_POINT ( 'NONE',  ( -5.087550801365593678, -2.228590825266444586, -2.752080473201636401 ) ) ;
#32661 = VERTEX_POINT ( 'NONE', #17189 ) ;
#32662 = AXIS2_PLACEMENT_3D ( 'NONE', #19230, #26931, #4034 ) ;
#32663 = AXIS2_PLACEMENT_3D ( 'NONE', #9904, #8048, #25604 ) ;
#32664 = AXIS2_PLACEMENT_3D ( 'NONE', #1397, #11082, #21281 ) ;
#32665 =( BOUNDED_CURVE ( )  B_SPLINE_CURVE ( 2, ( #30699, #10435, #3095, #20486, #17963, #20147, #265, #30342, #7412, #17795, #15275 ),
 .UNSPECIFIED., .F., .F. ) 
 B_SPLINE_CURVE_WITH_KNOTS ( ( 3, 2, 2, 2, 2, 3 ),
 ( 0.4353822619934377136, 0.4375000000000000000, 0.4531250000000000000, 0.4687500000000000000, 0.4843750000000000000, 0.4978822619934377136 ),
 .UNSPECIFIED. ) 
 CURVE ( )  GEOMETRIC_REPRESENTATION_ITEM ( )  RATIONAL_B_SPLINE_CURVE ( ( 0.9821626249036857770, 0.9896829947469991673, 1.000000000000000000, 0.9238795325112867385, 1.000000000000000000, 0.9238795325112867385, 1.000000000000000000, 0.9238795325112867385, 1.000000000000000000, 0.9341965377642874602, 0.9821626249036857770 ) ) 
 REPRESENTATION_ITEM ( '' )  );
#32666 = PLANE ( 'NONE',  #29583 ) ;
#32667 = FACE_OUTER_BOUND ( 'NONE', #4595, .T. ) ;
#32668 = ORIENTED_EDGE ( 'NONE', *, *, #8233, .F. ) ;
#32670 = CARTESIAN_POINT ( 'NONE',  ( 10.56183597391177464, 4.888740217817763464E-14, -4.753758587302147731 ) ) ;
#32669 = CIRCLE ( 'NONE', #8694, 8.750000000000000000 ) ;
#32671 = EDGE_CURVE ( 'NONE', #24299, #3835, #20544, .T. ) ;
#32672 = EDGE_LOOP ( 'NONE', ( #31771, #14345, #1901, #860 ) ) ;
#32673 = CIRCLE ( 'NONE', #8100, 2.499999999999996891 ) ;
#32674 = CIRCLE ( 'NONE', #13944, 8.749000000000002331 ) ;
#32675 = ORIENTED_EDGE ( 'NONE', *, *, #7960, .F. ) ;
#32676 = DIRECTION ( 'NONE',  ( -0.000000000000000000, 0.2588190451025185190, -0.9659258262890689783 ) ) ;
#32678 = VERTEX_POINT ( 'NONE', #27399 ) ;
#32677 = CARTESIAN_POINT ( 'NONE',  ( -3.043410827172835731, -0.3793687891476489882, 1.490164052093359670 ) ) ;
#32679 = ORIENTED_EDGE ( 'NONE', *, *, #15821, .F. ) ;
#32680 = CARTESIAN_POINT ( 'NONE',  ( 22.11000000136559507, -3.156283516753370488, -0.9349337715887220401 ) ) ;
#32681 = ADVANCED_FACE ( 'NONE', ( #26719 ), #23920, .T. ) ;
#32682 = VERTEX_POINT ( 'NONE', #19386 ) ;
#32683 = CARTESIAN_POINT ( 'NONE',  ( 0.3749742847179772798, 9.289351359934663321, -3.955024136977240978 ) ) ;
#32685 = VERTEX_POINT ( 'NONE', #29587 ) ;
#32684 = DIRECTION ( 'NONE',  ( -1.000000000000000000, 8.574039729943019576E-17, -6.162975822039154730E-33 ) ) ;
#32686 = CARTESIAN_POINT ( 'NONE',  ( -56.77769102277633095, 0.5030464795276025081, -1.050000000000000044 ) ) ;
#32687 = VECTOR ( 'NONE', #8941, 999.9999999999998863 ) ;
#32688 = DIRECTION ( 'NONE',  ( -1.387778780781444413E-14, 0.000000000000000000, -1.000000000000000000 ) ) ;
#32689 = CARTESIAN_POINT ( 'NONE',  ( 24.54750000136559507, 3.024605502323846729, -0.3178988483021056854 ) ) ;
#32690 = CYLINDRICAL_SURFACE ( 'NONE', #24745, 2.999999999999999112 ) ;
#32691 = AXIS2_PLACEMENT_3D ( 'NONE', #28550, #15969, #31234 ) ;
#32692 = AXIS2_PLACEMENT_3D ( 'NONE', #17357, #20539, #5148 ) ;
#32693 = CARTESIAN_POINT ( 'NONE',  ( 107.7673897845259461, 19.73285661471971508, 3.823381474136016145 ) ) ;
#32694 = DIRECTION ( 'NONE',  ( 0.000000000000000000, 0.000000000000000000, 1.000000000000000000 ) ) ;
#32695 = CARTESIAN_POINT ( 'NONE',  ( 24.61821134308531356, -17.47399247671398115, 1.556972331816578459 ) ) ;
#32696 = AXIS2_PLACEMENT_3D ( 'NONE', #19448, #24777, #27762 ) ;
#32697 = AXIS2_PLACEMENT_3D ( 'NONE', #30043, #12289, #15143 ) ;
#32698 = CARTESIAN_POINT ( 'NONE',  ( 0.7632845268398871230, -6.772677083992345359, -5.538577986808975062 ) ) ;
#32699 = CARTESIAN_POINT ( 'NONE',  ( 84.65816297383790356, -6.961284151106942097, 0.02339150517593242135 ) ) ;
#32700 = CARTESIAN_POINT ( 'NONE',  ( 3.499999999999999556, 2.871924938129881699, 6.435996203144517480 ) ) ;
#32701 = DIRECTION ( 'NONE',  ( 1.000000000000000000, -0.000000000000000000, -0.000000000000000000 ) ) ;
#32702 = ADVANCED_FACE ( 'NONE', ( #22053 ), #32274, .T. ) ;
#32703 = CARTESIAN_POINT ( 'NONE',  ( 23.68064580653238949, -7.171681651382474598, 4.522129901861163148 ) ) ;
#32704 = EDGE_CURVE ( 'NONE', #21921, #29082, #31770, .T. ) ;
#32705 = CARTESIAN_POINT ( 'NONE',  ( -2.400050802731187094, -3.113457007523259268, 0.9222479816126455399 ) ) ;
#32706 = ORIENTED_EDGE ( 'NONE', *, *, #22169, .F. ) ;
#32707 = CARTESIAN_POINT ( 'NONE',  ( -2.700050800000000084, 2.983565686104819648, 0.3135853898029609677 ) ) ;
#32708 = AXIS2_PLACEMENT_3D ( 'NONE', #7876, #4249, #30455 ) ;
#32709 = CIRCLE ( 'NONE', #1725, 10.99999999999999822 ) ;
#32710 = LINE ( 'NONE', #10102, #9812 ) ;
#32711 = CARTESIAN_POINT ( 'NONE',  ( 10.00000000000000178, 4.884328206559836794, 1.115095498423327225 ) ) ;
#32713 = EDGE_LOOP ( 'NONE', ( #16252, #10452, #10710, #21965 ) ) ;
#32712 = AXIS2_PLACEMENT_3D ( 'NONE', #2636, #12799, #23014 ) ;
#32714 = DIRECTION ( 'NONE',  ( -0.000000000000000000, -0.000000000000000000, -1.000000000000000000 ) ) ;
#32715 = CARTESIAN_POINT ( 'NONE',  ( 0.000000000000000000, -27.93932300454937590, -1.000000000000000000 ) ) ;
#32716 = CIRCLE ( 'NONE', #22562, 10.99999999999999822 ) ;
#32717 = VECTOR ( 'NONE', #32655, 1000.000000000000000 ) ;
#32718 = ORIENTED_EDGE ( 'NONE', *, *, #14515, .T. ) ;
#32719 = CARTESIAN_POINT ( 'NONE',  ( 8.533641835123258801, -14.05299950477806625, 1.499999999999999556 ) ) ;
#32720 = PERSON_AND_ORGANIZATION_ROLE ( 'classification_officer' ) ;
#32721 = AXIS2_PLACEMENT_3D ( 'NONE', #1902, #7051, #22270 ) ;
#32722 = FACE_OUTER_BOUND ( 'NONE', #22207, .T. ) ;
#32723 = ORIENTED_EDGE ( 'NONE', *, *, #7935, .F. ) ;
#32724 = DIRECTION ( 'NONE',  ( -8.281886410780478979E-17, -0.9659258262890646485, -0.2588190451025343397 ) ) ;
#32725 = VECTOR ( 'NONE', #23248, 1000.000000000000227 ) ;
#32726 = AXIS2_PLACEMENT_3D ( 'NONE', #18556, #31124, #13534 ) ;
#32727 = ADVANCED_FACE ( 'NONE', ( #17867 ), #10335, .T. ) ;
#32728 = ORIENTED_EDGE ( 'NONE', *, *, #346, .T. ) ;
#32729 = CC_DESIGN_PERSON_AND_ORGANIZATION_ASSIGNMENT ( #7947, #15645, ( #27464 ) ) ;
#32730 = CARTESIAN_POINT ( 'NONE',  ( 108.0161426671036082, -18.30181250712185559, -4.596922648963735369 ) ) ;
#32731 = CARTESIAN_POINT ( 'NONE',  ( 8.917264641016661386, 0.3030370628138376321, -1.471187449996646190 ) ) ;
#32732 = LINE ( 'NONE', #20028, #2207 ) ;
#32733 = CARTESIAN_POINT ( 'NONE',  ( -54.06000000000000227, -10.96999999999998643, 9.000000000000000000 ) ) ;
#32734 = DIRECTION ( 'NONE',  ( -1.000000000000000000, 8.574039729943015878E-17, 1.232595164407830946E-32 ) ) ;
#32735 = DIRECTION ( 'NONE',  ( 0.000000000000000000, 0.000000000000000000, 1.000000000000000000 ) ) ;
#32736 = CARTESIAN_POINT ( 'NONE',  ( 3.499999999999999556, 6.704570150426983233, 2.172265885002680808 ) ) ;
#32738 = ORIENTED_EDGE ( 'NONE', *, *, #26233, .T. ) ;
#32737 = DIRECTION ( 'NONE',  ( -1.000000000000000000, 8.574039729943019576E-17, 0.000000000000000000 ) ) ;
#32739 = CIRCLE ( 'NONE', #25251, 10.96966150227469328 ) ;
#32740 = B_SPLINE_CURVE_WITH_KNOTS ( 'NONE', 3,
 ( #28318, #10449, #28811, #5904, #16096, #3436, #20659, #31494 ),
 .UNSPECIFIED., .F., .F.,
 ( 4, 2, 2, 4 ),
 ( 0.009544196576262197265, 0.5047720982881310769, 0.7523860491440654830, 1.000000000000000000 ),
 .UNSPECIFIED. ) ;
#32741 = PRODUCT ( 'Part2_handle2', 'Part2_handle2', '', ( #14647 ) ) ;
#32742 = DIRECTION ( 'NONE',  ( -0.2880220749472530706, -0.1662896225033516362, 0.9430753128943475394 ) ) ;
#32743 = PLANE ( 'NONE',  #3797 ) ;
#32744 = CARTESIAN_POINT ( 'NONE',  ( 20.74999999999999645, -1.779113243963175696E-15, 0.000000000000000000 ) ) ;
#32745 = DIRECTION ( 'NONE',  ( 1.000000000000000000, -8.574039729943018344E-17, -0.000000000000000000 ) ) ;
#32746 = EDGE_CURVE ( 'NONE', #17929, #5917, #16783, .T. ) ;
#32747 = VECTOR ( 'NONE', #384, 1000.000000000000000 ) ;
#32748 = AXIS2_PLACEMENT_3D ( 'NONE', #10412, #20621, #30828 ) ;
#32749 = CARTESIAN_POINT ( 'NONE',  ( -8.000050800000002127, 2.386805812962781825, 2.383467509112250138 ) ) ;
#32750 = CARTESIAN_POINT ( 'NONE',  ( 10.56183597391177464, -4.753758587302148619, 0.000000000000000000 ) ) ;
#32751 = CARTESIAN_POINT ( 'NONE',  ( -56.75720195825324765, 0.3530522875096756552, -1.047845628850368582 ) ) ;
#32752 = CARTESIAN_POINT ( 'NONE',  ( 23.22564588060109259, -21.93932300456764040, 1.000000000000000000 ) ) ;
#32753 = EDGE_LOOP ( 'NONE', ( #12976, #28925, #21885, #25563 ) ) ;
#32754 = AXIS2_PLACEMENT_3D ( 'NONE', #9525, #1070, #14557 ) ;
#32755 = CARTESIAN_POINT ( 'NONE',  ( -5.412550801365593856, 3.368539882008727115, 1.828967928396026954 ) ) ;
#32756 = VERTEX_POINT ( 'NONE', #15492 ) ;
#32757 = CARTESIAN_POINT ( 'NONE',  ( -7.404531657079157725, 1.883076972206379374, 2.325406398514293205 ) ) ;
#32758 = DIRECTION ( 'NONE',  ( 1.000000000000000000, 0.000000000000000000, 0.000000000000000000 ) ) ;
#32759 = CARTESIAN_POINT ( 'NONE',  ( 102.6609843814833027, -1.982062027707615526, -4.522129901861162260 ) ) ;
#32760 = DIRECTION ( 'NONE',  ( 0.000000000000000000, -0.000000000000000000, -1.000000000000000000 ) ) ;
#32761 = FACE_OUTER_BOUND ( 'NONE', #12011, .T. ) ;
#32762 = VERTEX_POINT ( 'NONE', #9992 ) ;
#32763 = CARTESIAN_POINT ( 'NONE',  ( 21.37793795825544052, -21.75892242064796278, 1.431755257449183194 ) ) ;
#32764 = AXIS2_PLACEMENT_3D ( 'NONE', #14123, #24467, #13626 ) ;
#32765 = ORIENTED_EDGE ( 'NONE', *, *, #2417, .F. ) ;
#32766 = CARTESIAN_POINT ( 'NONE',  ( 5.885541838704151374, -5.105720535585458464, 6.662285765435201235 ) ) ;
#32767 = COORDINATED_UNIVERSAL_TIME_OFFSET ( 0, 0, .AHEAD. ) ;
#32768 = CARTESIAN_POINT ( 'NONE',  ( 85.03520090177219970, -5.194741742402703366, 4.008636570293263368 ) ) ;
#32769 = AXIS2_PLACEMENT_3D ( 'NONE', #6282, #956, #3145 ) ;
#32770 = AXIS2_PLACEMENT_3D ( 'NONE', #21099, #21247, #11049 ) ;
#32771 = CARTESIAN_POINT ( 'NONE',  ( 109.7606186995332536, 16.66703046365059393, 0.4463807625373084065 ) ) ;
#32773 = DIRECTION ( 'NONE',  ( 1.000000000000000000, -0.000000000000000000, -0.000000000000000000 ) ) ;
#32772 = CARTESIAN_POINT ( 'NONE',  ( 0.6728001243864745184, 7.719803900020854925, -4.913284922774296071 ) ) ;
#32774 = ORIENTED_EDGE ( 'NONE', *, *, #12498, .T. ) ;
#32775 = APPROVAL_PERSON_ORGANIZATION ( #18405, #26006, #18706 ) ;
#32776 = DIRECTION ( 'NONE',  ( -0.8660254037844409281, 0.4999999999999960587, 0.000000000000000000 ) ) ;
#32777 = DIRECTION ( 'NONE',  ( 0.000000000000000000, 0.000000000000000000, 1.000000000000000000 ) ) ;
#32778 = CARTESIAN_POINT ( 'NONE',  ( 22.92250000136559862, 0.3178988483021036315, 3.024605502323848949 ) ) ;
#32779 = CARTESIAN_POINT ( 'NONE',  ( 0.2332737126359348268, -7.747681480072266424, -1.773831282197832371 ) ) ;
#32781 = VERTEX_POINT ( 'NONE', #150 ) ;
#32780 = CARTESIAN_POINT ( 'NONE',  ( 0.1610798642962572302, -10.72944008624798151, 4.522129901861157819 ) ) ;
#32782 = CARTESIAN_POINT ( 'NONE',  ( -7.862550801365593145, 3.521866450007987037, 0.3701630799359328372 ) ) ;
#32783 = CYLINDRICAL_SURFACE ( 'NONE', #26713, 3.250000000000002665 ) ;
#32784 = CARTESIAN_POINT ( 'NONE',  ( 29.41391112839824373, -2.700987858903443950, 0.07017451552782173751 ) ) ;
#32785 = CARTESIAN_POINT ( 'NONE',  ( 3.499999999999999556, 2.871924938129968741, -6.435996203144479288 ) ) ;
#32786 = VERTEX_POINT ( 'NONE', #30759 ) ;
#32787 = EDGE_CURVE ( 'NONE', #1029, #23722, #21176, .T. ) ;
#32789 = VERTEX_POINT ( 'NONE', #2333 ) ;
#32788 = CARTESIAN_POINT ( 'NONE',  ( 23.02255580927015188, -17.31849206757248183, 1.529834177132855633 ) ) ;
#32790 = EDGE_CURVE ( 'NONE', #22104, #21443, #13998, .T. ) ;
#32791 = CIRCLE ( 'NONE', #1834, 0.5000000000000000000 ) ;
#32792 = CARTESIAN_POINT ( 'NONE',  ( 23.80188655377674323, 18.45496240403558019, 1.500000000000000222 ) ) ;
#32793 = CARTESIAN_POINT ( 'NONE',  ( 109.4831014662949258, 20.77917954950597590, 0.4463807625372899768 ) ) ;
#32794 = EDGE_CURVE ( 'NONE', #8502, #3835, #17675, .T. ) ;
#32795 = CARTESIAN_POINT ( 'NONE',  ( 3.249999999999999556, 0.000000000000000000, 0.000000000000000000 ) ) ;
#32796 = TOROIDAL_SURFACE ( 'NONE', #13014, 10.51776515689528502, 0.5000000000000000000 ) ;
#32797 = AXIS2_PLACEMENT_3D ( 'NONE', #12908, #28286, #31161 ) ;
#32798 = DIRECTION ( 'NONE',  ( -1.000000000000000000, -0.000000000000000000, 0.000000000000000000 ) ) ;
#32799 = CARTESIAN_POINT ( 'NONE',  ( -29.33353502638487953, 7.575402792874002422, 2.048453119712660087 ) ) ;
#32800 = CARTESIAN_POINT ( 'NONE',  ( -2.787158681079298095, -12.40563758779646264, -1.500000000000000000 ) ) ;
#32801 = CARTESIAN_POINT ( 'NONE',  ( 24.85999999999999943, 1.573300977624590313, -1.942864903642426144 ) ) ;
#32802 = B_SPLINE_CURVE_WITH_KNOTS ( 'NONE', 3,
 ( #21130, #23303, #69, #20483, #15604, #17792, #18279, #7769, #5742, #31329 ),
 .UNSPECIFIED., .F., .F.,
 ( 4, 2, 2, 2, 4 ),
 ( 2.571685856657688708E-07, 0.0005478592107668812028, 0.001095461252948096761, 0.001643063295129312210, 0.002190665337310527660 ),
 .UNSPECIFIED. ) ;
#32803 = LOCAL_TIME ( 16, 7, 10.00000000000000000, #31887 ) ;
#32804 = CARTESIAN_POINT ( 'NONE',  ( 29.34042402276785566, -3.698761498129368164, 0.4367664976601824955 ) ) ;
#32805 = FACE_OUTER_BOUND ( 'NONE', #9598, .T. ) ;
#32806 = ORIENTED_EDGE ( 'NONE', *, *, #27284, .F. ) ;
#32807 = CARTESIAN_POINT ( 'NONE',  ( 56.97280603064898941, -277.2763395528616002, 2.806473568333413660 ) ) ;
#32808 = APPROVAL_DATE_TIME ( #30442, #3324 ) ;
#32809 = FACE_OUTER_BOUND ( 'NONE', #18306, .T. ) ;
#32810 = ORIENTED_EDGE ( 'NONE', *, *, #4395, .F. ) ;
#32811 = CIRCLE ( 'NONE', #18389, 0.5000000000000000000 ) ;
#32812 = CARTESIAN_POINT ( 'NONE',  ( 107.9511351265079782, 17.90606102802182420, -4.842550456795976288 ) ) ;
#32813 = ORIENTED_EDGE ( 'NONE', *, *, #23857, .T. ) ;
#32814 = PLANE ( 'NONE',  #30614 ) ;
#32816 = VERTEX_POINT ( 'NONE', #30091 ) ;
#32815 = CARTESIAN_POINT ( 'NONE',  ( 69.01421513638182148, -4.990059488610206095, -4.023790688807778793 ) ) ;
#32817 = VERTEX_POINT ( 'NONE', #5160 ) ;
#32818 = CARTESIAN_POINT ( 'NONE',  ( 23.61000000000000298, -1.942864903642428587, -1.573300977624592756 ) ) ;
#32819 = CARTESIAN_POINT ( 'NONE',  ( 23.90742340929308085, -3.204431202270363599, 2.713652344655541615 ) ) ;
#32821 = VERTEX_POINT ( 'NONE', #5000 ) ;
#32820 = CARTESIAN_POINT ( 'NONE',  ( 0.3076689308780826138, 5.232617538234601184, 8.857103639574667397 ) ) ;
#32822 = CARTESIAN_POINT ( 'NONE',  ( 23.82349779645404553, 17.94250544646148882, -1.499999999999882316 ) ) ;
#32823 = DIRECTION ( 'NONE',  ( 0.000000000000000000, 0.9063077870366493816, 0.4226182617407006070 ) ) ;
#32824 = DIRECTION ( 'NONE',  ( 0.000000000000000000, 0.000000000000000000, 1.000000000000000000 ) ) ;
#32825 = SECURITY_CLASSIFICATION ( '', '', #32000 ) ;
#32826 = CARTESIAN_POINT ( 'NONE',  ( 8.845957756765750801, -0.9823800963979932854, -1.500000000000000000 ) ) ;
#32827 = EDGE_CURVE ( 'NONE', #9415, #9377, #22718, .T. ) ;
#32829 = EDGE_LOOP ( 'NONE', ( #8035, #30180, #11224, #24885, #30336 ) ) ;
#32828 = CARTESIAN_POINT ( 'NONE',  ( 107.5612922043142561, -18.97663357200326217, -4.540760459233397661 ) ) ;
#32830 = DIRECTION ( 'NONE',  ( 0.000000000000000000, 0.000000000000000000, 1.000000000000000000 ) ) ;
#32831 = EDGE_CURVE ( 'NONE', #7759, #3542, #3884, .T. ) ;
#32832 = PLANE ( 'NONE',  #32663 ) ;
#32833 = CARTESIAN_POINT ( 'NONE',  ( 25.23500000136559507, -1.570731468192933633, -2.892927487894330074 ) ) ;
#32834 = DIRECTION ( 'NONE',  ( 1.000000000000000000, -0.000000000000000000, -0.000000000000000000 ) ) ;
#32835 = DIRECTION ( 'NONE',  ( -1.000000000000000000, -0.000000000000000000, 0.000000000000000000 ) ) ;
#32836 = DIRECTION ( 'NONE',  ( 0.9947025833170223263, 0.1027947991993880261, -0.000000000000000000 ) ) ;
#32837 = AXIS2_PLACEMENT_3D ( 'NONE', #16454, #32869, #22314 ) ;
#32838 = VERTEX_POINT ( 'NONE', #12664 ) ;
#32839 = CARTESIAN_POINT ( 'NONE',  ( 14.23800746264080885, 22.11259878822730229, 1.508259000770582059 ) ) ;
#32840 = CARTESIAN_POINT ( 'NONE',  ( -1.773875666770781789, -0.3178988483021056854, 3.024605502323848949 ) ) ;
#32841 = CARTESIAN_POINT ( 'NONE',  ( -6.487550801365593145, 2.752080473201636845, -2.228590825266444142 ) ) ;
#32842 = VERTEX_POINT ( 'NONE', #14991 ) ;
#32843 = B_SPLINE_CURVE_WITH_KNOTS ( 'NONE', 3,
 ( #7633, #15652, #25862, #8120 ),
 .UNSPECIFIED., .F., .F.,
 ( 4, 4 ),
 ( 0.0005429330443435420768, 0.0007203473150553858393 ),
 .UNSPECIFIED. ) ;
#32844 = DIRECTION ( 'NONE',  ( -1.000000000000000000, 0.000000000000000000, 0.000000000000000000 ) ) ;
#32845 = DIRECTION ( 'NONE',  ( -0.000000000000000000, 0.000000000000000000, 1.000000000000000000 ) ) ;
#32846 = FACE_OUTER_BOUND ( 'NONE', #10956, .T. ) ;
#32847 = ORIENTED_EDGE ( 'NONE', *, *, #29075, .T. ) ;
#32848 = DIRECTION ( 'NONE',  ( 0.000000000000000000, -0.7071067811865495711, 0.7071067811865454633 ) ) ;
#32849 = EDGE_LOOP ( 'NONE', ( #12963, #23430, #10486 ) ) ;
#32850 = CARTESIAN_POINT ( 'NONE',  ( -3.687551352559800218E-13, 10.76487093102146098, 1.999317321091203192 ) ) ;
#32851 = ORIENTED_EDGE ( 'NONE', *, *, #1409, .T. ) ;
#32852 = CARTESIAN_POINT ( 'NONE',  ( 0.7632845268398876781, -3.174628368996014860, -8.152713396088786979 ) ) ;
#32853 = EDGE_CURVE ( 'NONE', #32480, #17452, #6824, .T. ) ;
#32855 = ORIENTED_EDGE ( 'NONE', *, *, #18751, .F. ) ;
#32854 = PLANE ( 'NONE',  #2667 ) ;
#32856 = ORIENTED_EDGE ( 'NONE', *, *, #9846, .T. ) ;
#32857 = DIRECTION ( 'NONE',  ( 0.000000000000000000, 0.000000000000000000, 1.000000000000000000 ) ) ;
#32858 = VERTEX_POINT ( 'NONE', #25707 ) ;
#32859 = CYLINDRICAL_SURFACE ( 'NONE', #5434, 5.010000000000000675 ) ;
#32860 = ADVANCED_FACE ( 'NONE', ( #22867 ), #30400, .T. ) ;
#32862 = ORIENTED_EDGE ( 'NONE', *, *, #5851, .T. ) ;
#32861 = CARTESIAN_POINT ( 'NONE',  ( 0.1962428234089072521, -6.885380501030516243, -1.500000000000000000 ) ) ;
#32863 = CARTESIAN_POINT ( 'NONE',  ( 1.750000000000000222, -7.851777359434023218, 3.255701506262406841 ) ) ;
#32864 = DIRECTION ( 'NONE',  ( -0.4809547266710039182, 0.000000000000000000, 0.8767454310646960458 ) ) ;
#32865 = PLANE ( 'NONE',  #3407 ) ;
#32866 = CARTESIAN_POINT ( 'NONE',  ( 7.249760686538667009, 0.7071067811866343922, -8.721381771256197624 ) ) ;
#32867 = EDGE_CURVE ( 'NONE', #22455, #31994, #22573, .T. ) ;
#32868 = DIRECTION ( 'NONE',  ( -1.000000000000000000, -5.263081354843156381E-15, 0.000000000000000000 ) ) ;
#32869 = DIRECTION ( 'NONE',  ( -0.000000000000000000, 0.000000000000000000, 1.000000000000000000 ) ) ;
#32870 = CARTESIAN_POINT ( 'NONE',  ( 7.249760686538667009, 4.973063321323977881, -7.199384779417068891 ) ) ;
#32871 = CARTESIAN_POINT ( 'NONE',  ( 68.79832465278998654, -7.861404707920828905, -0.02339150517595086839 ) ) ;
#32872 = CARTESIAN_POINT ( 'NONE',  ( 6.356381935169121533, 8.556754636093206301, 0.9265622495396070857 ) ) ;
#32873 = CARTESIAN_POINT ( 'NONE',  ( 84.37491783462850492, -2.359815117480457136, 0.02339150516272687358 ) ) ;
#32874 =( BOUNDED_SURFACE ( )  B_SPLINE_SURFACE ( 3, 2, ( 
 ( #29, #10214, #7731 ),
 ( #12393, #25778, #20436 ),
 ( #17923, #2905, #30813 ),
 ( #20757, #18073, #5373 ),
 ( #13068, #371, #10546 ),
 ( #30957, #28450, #25091 ),
 ( #9897, #23755, #3544 ),
 ( #13850, #21582, #29256 ),
 ( #13702, #11381, #3202 ),
 ( #21097, #18424, #28614 ),
 ( #21402, #31299, #10702 ),
 ( #8371, #31612, #15888 ),
 ( #8521, #24056, #13363 ),
 ( #18568, #5708, #26445 ),
 ( #28760, #13546, #1182 ),
 ( #3380, #868, #26097 ),
 ( #23904, #11196, #15743 ),
 ( #23576, #10890, #5850 ),
 ( #3691, #16034, #26265 ),
 ( #699, #23412, #11047 ),
 ( #1012, #21245, #8699 ),
 ( #25946, #31443, #18722 ) ),
 .UNSPECIFIED., .F., .F., .F. ) 
 B_SPLINE_SURFACE_WITH_KNOTS ( ( 4, 2, 2, 2, 2, 2, 2, 2, 2, 2, 4 ),
 ( 3, 3 ),
 ( 0.004062408222415266751, 0.005697251201790947198, 0.007332094181166628512, 0.01060178013991799027, 0.01387146609866935290, 0.01550630907804503335, 0.01714115205742071379, 0.02041083801617207816, 0.02368052397492343905, 0.02695020993367479994, 0.03021989589242616431 ),
 ( 0.000000000000000000, 1.000000000000000000 ),
 .UNSPECIFIED. ) 
 GEOMETRIC_REPRESENTATION_ITEM ( )  RATIONAL_B_SPLINE_SURFACE ( (
 ( 1.000000000000000000, 0.7071067811865475727, 1.000000000000000000),
 ( 1.000000000000000000, 0.7071067811865475727, 1.000000000000000000),
 ( 1.000000000000000000, 0.7071067811865475727, 1.000000000000000000),
 ( 1.000000000000000000, 0.7071067811865475727, 1.000000000000000000),
 ( 1.000000000000000000, 0.7071067811865475727, 1.000000000000000000),
 ( 1.000000000000000000, 0.7071067811865475727, 1.000000000000000000),
 ( 1.000000000000000000, 0.7071067811865475727, 1.000000000000000000),
 ( 1.000000000000000000, 0.7071067811865475727, 1.000000000000000000),
 ( 1.000000000000000000, 0.7071067811865475727, 1.000000000000000000),
 ( 1.000000000000000000, 0.7071067811865475727, 1.000000000000000000),
 ( 1.000000000000000000, 0.7071067811865483499, 1.000000000000000000),
 ( 1.000000000000000000, 0.7071067811865483499, 1.000000000000000000),
 ( 1.000000000000000000, 0.7071067811865475727, 1.000000000000000000),
 ( 1.000000000000000000, 0.7071067811865475727, 1.000000000000000000),
 ( 1.000000000000000000, 0.7071067811865475727, 1.000000000000000000),
 ( 1.000000000000000000, 0.7071067811865475727, 1.000000000000000000),
 ( 1.000000000000000000, 0.7071067811865475727, 1.000000000000000000),
 ( 1.000000000000000000, 0.7071067811865475727, 1.000000000000000000),
 ( 1.000000000000000000, 0.7071067811865475727, 1.000000000000000000),
 ( 1.000000000000000000, 0.7071067811865475727, 1.000000000000000000),
 ( 1.000000000000000000, 0.7071067811865475727, 1.000000000000000000),
 ( 1.000000000000000000, 0.7071067811865475727, 1.000000000000000000) ) ) 
 REPRESENTATION_ITEM ( '' )  SURFACE ( )  );
#32875 = EDGE_CURVE ( 'NONE', #1268, #16254, #7666, .T. ) ;
#32876 = FACE_OUTER_BOUND ( 'NONE', #14910, .T. ) ;
#32877 = CARTESIAN_POINT ( 'NONE',  ( -4.000050802731187183, -3.113457007523259268, 0.9222479816126455399 ) ) ;
#32878 = VERTEX_POINT ( 'NONE', #7473 ) ;
#32879 = CARTESIAN_POINT ( 'NONE',  ( -2.550050800000000173, 0.9222479816126443186, 3.113457007523260156 ) ) ;
#32880 = DIRECTION ( 'NONE',  ( 3.623545766764247286E-17, 0.4226182617407038267, -0.9063077870366479383 ) ) ;
#32881 = DIRECTION ( 'NONE',  ( -1.000000000000000000, 0.000000000000000000, -0.000000000000000000 ) ) ;
#32882 = ORIENTED_EDGE ( 'NONE', *, *, #822, .T. ) ;
#32883 = CARTESIAN_POINT ( 'NONE',  ( -50.60000000000000142, -10.96966150227468972, 7.074999999999997513 ) ) ;
#32884 = CARTESIAN_POINT ( 'NONE',  ( 0.000000000000000000, 18.00000000000000355, 0.000000000000000000 ) ) ;
#32885 = ADVANCED_FACE ( 'NONE', ( #7323 ), #17233, .F. ) ;
#32886 = CARTESIAN_POINT ( 'NONE',  ( 107.4513092838961796, -17.37832399921928683, 4.568466631925298671 ) ) ;
#32887 = VERTEX_POINT ( 'NONE', #5803 ) ;
#32888 = CARTESIAN_POINT ( 'NONE',  ( 101.7915511448668582, -3.896871997815702482, -4.171847251125799794 ) ) ;
#32889 = EDGE_CURVE ( 'NONE', #18983, #24335, #12413, .T. ) ;
#32890 = CONTEXT_DEPENDENT_SHAPE_REPRESENTATION ( #12487, #193 ) ;
#32891 = CARTESIAN_POINT ( 'NONE',  ( 111.5384102276657785, -20.44549501351493603, -0.9788672205760856615 ) ) ;
#32892 = VERTEX_POINT ( 'NONE', #960 ) ;
#32893 = DIRECTION ( 'NONE',  ( -0.09975574163943223827, 0.1727820128662104493, -0.9798954883250904357 ) ) ;
#32894 = EDGE_LOOP ( 'NONE', ( #22784, #5932, #7582 ) ) ;
#32895 = CARTESIAN_POINT ( 'NONE',  ( 107.9988871568685909, -18.05333745236665166, -4.637859085129263370 ) ) ;
#32897 = VERTEX_POINT ( 'NONE', #5496 ) ;
#32896 = CARTESIAN_POINT ( 'NONE',  ( -23.54713438637982748, 3.263167658947396799, 6.089596369742212190 ) ) ;
#32898 = DIRECTION ( 'NONE',  ( 0.000000000000000000, 1.000000000000000000, 0.000000000000000000 ) ) ;
#32899 = DIRECTION ( 'NONE',  ( 1.000000000000000000, -8.574039729943018344E-17, -0.000000000000000000 ) ) ;
#32900 = EDGE_CURVE ( 'NONE', #4647, #24556, #908, .T. ) ;
#32901 = CARTESIAN_POINT ( 'NONE',  ( 21.40209301355503513, -21.75562217689082800, -1.444354797330493989 ) ) ;
#32902 = ADVANCED_FACE ( 'NONE', ( #5657 ), #15685, .T. ) ;
#32903 = CARTESIAN_POINT ( 'NONE',  ( 101.7974586501933203, -3.981938604915898683, 4.091315454896042425 ) ) ;
#32904 = ORIENTED_EDGE ( 'NONE', *, *, #15383, .F. ) ;
#32905 = CARTESIAN_POINT ( 'NONE',  ( 7.249760686538667009, -6.226446564517957860, 6.147671362329200306 ) ) ;
#32906 = CARTESIAN_POINT ( 'NONE',  ( 3.822634483660936850E-16, 4.458382051008224600, -2.285372942704906762 ) ) ;
#32907 = CARTESIAN_POINT ( 'NONE',  ( 4.749760686538667009, -1.391664247347281780, 7.892520144992429820 ) ) ;
#32908 = CARTESIAN_POINT ( 'NONE',  ( -23.54713438637982748, 8.275374457817619600, 8.600000000000004974 ) ) ;
#32909 = EDGE_CURVE ( 'NONE', #22878, #5480, #11139, .T. ) ;
#32910 = CARTESIAN_POINT ( 'NONE',  ( 1.750000000000000222, -7.673322273190700926, -3.656518192455154193 ) ) ;
#32911 = CARTESIAN_POINT ( 'NONE',  ( -56.52933573942885204, 0.04063196321577920711, -1.249307687641485476 ) ) ;
#32912 = LINE ( 'NONE', #22710, #8659 ) ;
#32913 = ORIENTED_EDGE ( 'NONE', *, *, #22049, .T. ) ;
#32914 = CARTESIAN_POINT ( 'NONE',  ( -6.012550801365594388, -1.828967928396026510, 3.368539882008728004 ) ) ;
#32915 = ORIENTED_EDGE ( 'NONE', *, *, #82, .F. ) ;
#32916 = ADVANCED_FACE ( 'NONE', ( #25894 ), #10495, .T. ) ;
#32917 = CARTESIAN_POINT ( 'NONE',  ( -5.754531657079158258, 0.9198621039125853827, 3.105402419394639235 ) ) ;
#32918 = CARTESIAN_POINT ( 'NONE',  ( 21.86000000136559507, 1.570731468192929858, 2.892927487894329186 ) ) ;
#32919 = DIRECTION ( 'NONE',  ( -1.000000000000000000, -0.000000000000000000, -0.000000000000000000 ) ) ;
#32920 = CARTESIAN_POINT ( 'NONE',  ( 23.61632761762281163, -8.296864917633445913, -2.713652344655543391 ) ) ;
#32921 = DIRECTION ( 'NONE',  ( 0.000000000000000000, -0.9876883405951383255, 0.1564344650402271775 ) ) ;
#32922 = ORIENTED_EDGE ( 'NONE', *, *, #13896, .F. ) ;
#32923 = CARTESIAN_POINT ( 'NONE',  ( 12.44989959798878232, 19.51744974835125035, 2.318435636271098943 ) ) ;
#32924 = FACE_OUTER_BOUND ( 'NONE', #30843, .T. ) ;
#32925 = VERTEX_POINT ( 'NONE', #20708 ) ;
#32926 = CARTESIAN_POINT ( 'NONE',  ( -3.312942406915326377, -5.022711880624455567E-15, 2.999999999999999556 ) ) ;
#32927 = DATE_TIME_ROLE ( 'classification_date' ) ;
#32928 = CARTESIAN_POINT ( 'NONE',  ( 40.88394771555588392, -6.888509962679972176, 4.006106576922047857 ) ) ;
#32929 = ADVANCED_FACE ( 'NONE', ( #31546 ), #9182, .T. ) ;
#32930 = CARTESIAN_POINT ( 'NONE',  ( 2.482257818914018088, 0.000000000000000000, -1.712210361609936005 ) ) ;
#32932 = DIRECTION ( 'NONE',  ( 0.000000000000000000, -0.8191520442889824727, -0.5735764363510594821 ) ) ;
#32931 = CARTESIAN_POINT ( 'NONE',  ( 0.7632845268398871230, -8.461683424509292450, -2.223716399045660985 ) ) ;
#32933 = ORIENTED_EDGE ( 'NONE', *, *, #6928, .F. ) ;
#32934 = EDGE_CURVE ( 'NONE', #25317, #2704, #20457, .T. ) ;
#32935 = CARTESIAN_POINT ( 'NONE',  ( 108.0375632182117869, -18.61026311478333994, -4.377304920009720490 ) ) ;
#32936 = DIRECTION ( 'NONE',  ( -1.000000000000000000, 0.000000000000000000, 0.000000000000000000 ) ) ;
#32937 = CARTESIAN_POINT ( 'NONE',  ( 25.42250000136559507, -0.3178988483021076838, -3.024605502323848949 ) ) ;
#32938 = LINE ( 'NONE', #28076, #22545 ) ;
#32940 = ORIENTED_EDGE ( 'NONE', *, *, #32492, .F. ) ;
#32939 = CARTESIAN_POINT ( 'NONE',  ( 7.064632879756604034, 8.711672189281438605, -0.8180878109960962874 ) ) ;
#32941 = CARTESIAN_POINT ( 'NONE',  ( -4.712550801365592790, 3.675193018007247403, -1.088641768524161391 ) ) ;
#32942 = DIRECTION ( 'NONE',  ( -1.000000000000000000, -0.000000000000000000, -0.000000000000000000 ) ) ;
#32943 = FACE_OUTER_BOUND ( 'NONE', #11913, .T. ) ;
#32944 = FACE_BOUND ( 'NONE', #31441, .T. ) ;
#32945 = ORIENTED_EDGE ( 'NONE', *, *, #6395, .F. ) ;
#32947 = ORIENTED_EDGE ( 'NONE', *, *, #13829, .T. ) ;
#32946 = CARTESIAN_POINT ( 'NONE',  ( 24.09939086539757014, -17.43210107469715098, 1.523452847363739870 ) ) ;
#32948 = EDGE_CURVE ( 'NONE', #4058, #21466, #8183, .T. ) ;
#32949 = CARTESIAN_POINT ( 'NONE',  ( 9.331062908042598636, 15.00000000000002132, -4.612695725900422872 ) ) ;
#32950 = DIRECTION ( 'NONE',  ( 1.000000000000000000, -0.000000000000000000, -0.000000000000000000 ) ) ;
#32951 = CARTESIAN_POINT ( 'NONE',  ( 22.79750000136559862, 2.363507492473148286, 1.913930629741525058 ) ) ;
#32952 = EDGE_CURVE ( 'NONE', #1225, #17959, #628, .T. ) ;
#32953 = CARTESIAN_POINT ( 'NONE',  ( 18.96091535642496240, -3.614110606601104614, 2.184956778830005053 ) ) ;
#32954 = CARTESIAN_POINT ( 'NONE',  ( 5.388150845455290217, -18.36759383093766118, -1.499999999999999112 ) ) ;
#32955 = PRODUCT_RELATED_PRODUCT_CATEGORY ( 'detail', '', ( #25253 ) ) ;
#32956 = CARTESIAN_POINT ( 'NONE',  ( 6.883866601413089370, 7.193114723270807254, 4.949663153219556300 ) ) ;
#32957 = DIRECTION ( 'NONE',  ( -8.541412920197218582E-17, -0.9961946980917459893, 0.08715574274765194862 ) ) ;
#32958 = CARTESIAN_POINT ( 'NONE',  ( 3.529825581556927552E-16, 4.116875700062083254, 2.376879293651078751 ) ) ;
#32959 = ORIENTED_EDGE ( 'NONE', *, *, #12814, .T. ) ;
#32960 = CARTESIAN_POINT ( 'NONE',  ( 0.5982512417152469064, -7.989521869415790789, 5.029253150608139933 ) ) ;
#32961 = DATE_AND_TIME ( #15724, #12999 ) ;
#32962 = DIRECTION ( 'NONE',  ( 0.000000000000000000, 0.000000000000000000, 1.000000000000000000 ) ) ;
#32963 = ORIENTED_EDGE ( 'NONE', *, *, #25482, .T. ) ;
#32964 = ADVANCED_FACE ( 'NONE', ( #24663 ), #12971, .T. ) ;
#32965 = CARTESIAN_POINT ( 'NONE',  ( 107.6039373603924645, 18.80783371073036037, -5.109269587507049515 ) ) ;
#32966 = ORIENTED_EDGE ( 'NONE', *, *, #32657, .F. ) ;
#32967 = CARTESIAN_POINT ( 'NONE',  ( -19.40370476787681042, 16.88291497481784020, 1.811101872898883469 ) ) ;
#32968 = ADVANCED_FACE ( 'NONE', ( #8950 ), #11482, .T. ) ;
#32970 = VERTEX_POINT ( 'NONE', #3972 ) ;
#32969 = CARTESIAN_POINT ( 'NONE',  ( 40.87788096477831346, -5.775834591683154606, -4.033869542163018629 ) ) ;
#32971 = ORIENTED_EDGE ( 'NONE', *, *, #7500, .F. ) ;
#32972 = CARTESIAN_POINT ( 'NONE',  ( -50.60000000000000142, -10.96966150227468972, 1.500000000000000000 ) ) ;
#32973 = CARTESIAN_POINT ( 'NONE',  ( -6.962550801365593678, 2.228590825266444142, 2.752080473201636845 ) ) ;
#32974 = DIRECTION ( 'NONE',  ( 0.9896144216807899463, -0.000000000000000000, 0.1437473352845035635 ) ) ;
#32975 = PLANE ( 'NONE',  #31101 ) ;
#32977 = VERTEX_POINT ( 'NONE', #32228 ) ;
#32976 = CARTESIAN_POINT ( 'NONE',  ( -2.147796952350726040E-16, 1.841529640130565566E-32, 0.000000000000000000 ) ) ;
#32978 = CARTESIAN_POINT ( 'NONE',  ( 25.05859343314882537, 19.07886064307538021, -1.500000000000000000 ) ) ;
#32979 = CARTESIAN_POINT ( 'NONE',  ( 25.75999999999999801, -6.000000000000002665, 7.347880794884119736E-16 ) ) ;
#32980 = CARTESIAN_POINT ( 'NONE',  ( -4.147439473165015045, -6.154442848042452674, 1.745243268039455620 ) ) ;
#32981 = DIRECTION ( 'NONE',  ( 0.000000000000000000, 0.000000000000000000, 1.000000000000000000 ) ) ;
#32983 = ORIENTED_EDGE ( 'NONE', *, *, #8777, .F. ) ;
#32982 = CARTESIAN_POINT ( 'NONE',  ( 107.5615883074459020, -18.98093538359634636, -4.529405805268299723 ) ) ;
#32984 = DIRECTION ( 'NONE',  ( 4.917867153432934934E-17, 0.5735764363510388320, 0.8191520442889969056 ) ) ;
#32985 = CARTESIAN_POINT ( 'NONE',  ( 10.00000000000000178, 5.999999999999998224, 0.000000000000000000 ) ) ;
#32986 = CARTESIAN_POINT ( 'NONE',  ( 25.48500000136559862, 2.892927487894327410, -1.570731468192931635 ) ) ;
#32987 = CYLINDRICAL_SURFACE ( 'NONE', #4372, 3.000000000000000444 ) ;
#32988 = CARTESIAN_POINT ( 'NONE',  ( -2.837798564937434875, -0.5311976243149594268, -1.513817338014939118 ) ) ;
#32989 = EDGE_LOOP ( 'NONE', ( #16429, #2124, #11527, #13563 ) ) ;
#32990 = DIRECTION ( 'NONE',  ( -1.000000000000000000, 0.000000000000000000, 0.000000000000000000 ) ) ;
#32991 = CARTESIAN_POINT ( 'NONE',  ( -5.737550801365594033, 1.828967928396027398, -3.368539882008727115 ) ) ;
#32992 = EDGE_LOOP ( 'NONE', ( #5277, #29547, #5200 ) ) ;
#32993 = CARTESIAN_POINT ( 'NONE',  ( 7.249760686538667009, 6.940565734314653845, -4.007137495034738706 ) ) ;
#32994 = DIRECTION ( 'NONE',  ( 0.1908089953765452762, 0.000000000000000000, 0.9816271834476639757 ) ) ;
#32995 = CARTESIAN_POINT ( 'NONE',  ( 102.9361373302715918, -5.944196040818416016, 2.713652344655542503 ) ) ;
#32996 = VERTEX_POINT ( 'NONE', #1303 ) ;
#32997 = CARTESIAN_POINT ( 'NONE',  ( 107.1772993348646139, 16.40207914262226296, 0.000000000000000000 ) ) ;
#32998 = EDGE_CURVE ( 'NONE', #14095, #22172, #21523, .T. ) ;
#32999 = ORIENTED_EDGE ( 'NONE', *, *, #31552, .F. ) ;
#33000 = EDGE_CURVE ( 'NONE', #21466, #11105, #29540, .T. ) ;
#33001 = CARTESIAN_POINT ( 'NONE',  ( -40.76519394227695159, -12.76841724022742852, 5.871858310191298003 ) ) ;
#33002 = ORIENTED_EDGE ( 'NONE', *, *, #811, .F. ) ;
#33003 = CARTESIAN_POINT ( 'NONE',  ( -2.742527549463130931, 0.2598362491872778235, 1.021881266978499792 ) ) ;
#33005 = ORIENTED_EDGE ( 'NONE', *, *, #8207, .T. ) ;
#33004 = LINE ( 'NONE', #24964, #9050 ) ;
#33006 = EDGE_LOOP ( 'NONE', ( #8485, #6061 ) ) ;
#33007 = CARTESIAN_POINT ( 'NONE',  ( -0.2059365608663963898, 0.000000000000000000, 0.000000000000000000 ) ) ;
#33008 = ORIENTED_EDGE ( 'NONE', *, *, #27007, .F. ) ;
#33009 = DIRECTION ( 'NONE',  ( 0.000000000000000000, 1.000000000000000000, 0.000000000000000000 ) ) ;
#33011 = VERTEX_POINT ( 'NONE', #4276 ) ;
#33010 = CARTESIAN_POINT ( 'NONE',  ( 18.86054332783663767, -4.736068442360261699, 3.993434336035624366 ) ) ;
#33012 = CARTESIAN_POINT ( 'NONE',  ( 0.1371395441367533607, -7.141515111121043091, -1.774689084756775781 ) ) ;
#33013 = DIRECTION ( 'NONE',  ( -1.000000000000000000, 0.000000000000000000, 0.000000000000000000 ) ) ;
#33014 = CARTESIAN_POINT ( 'NONE',  ( -47.64323377349501243, 16.45499999999998408, 1.050000000000000044 ) ) ;
#33015 = DIRECTION ( 'NONE',  ( -1.000000000000000000, 0.000000000000000000, 0.000000000000000000 ) ) ;
#33016 = DIRECTION ( 'NONE',  ( 8.541412920197229675E-17, 0.9961946980917466554, -0.08715574274764535667 ) ) ;
#33017 = LINE ( 'NONE', #4604, #19837 ) ;
#33018 = CARTESIAN_POINT ( 'NONE',  ( 25.29940076078100475, -17.51841556854394710, 1.122629911123150803 ) ) ;
#33019 = CARTESIAN_POINT ( 'NONE',  ( -3.142639414278896925, -12.00291247001455730, 0.9788672205877712029 ) ) ;
#33020 = CARTESIAN_POINT ( 'NONE',  ( 0.9232102171129888957, 0.000000000000000000, 4.522129901861156931 ) ) ;
#33021 = CARTESIAN_POINT ( 'NONE',  ( 19.01480233880806381, -3.011762293215139330, 0.07017451552781951707 ) ) ;
#33022 = CARTESIAN_POINT ( 'NONE',  ( 19.01480233880806381, -3.011762293215139330, -0.07017451552781628354 ) ) ;
#33023 = CARTESIAN_POINT ( 'NONE',  ( 69.13057415542958495, -2.987362752442197955, 2.713652344655542503 ) ) ;
#33024 = CARTESIAN_POINT ( 'NONE',  ( -2.850050802731187716, 2.331437884370912705, -1.887961173149511618 ) ) ;
#33025 = ORIENTED_EDGE ( 'NONE', *, *, #19243, .F. ) ;
#33026 = CARTESIAN_POINT ( 'NONE',  ( -5.737550801365594033, 1.828967928396027176, -3.368539882008727115 ) ) ;
#33027 = EDGE_CURVE ( 'NONE', #24941, #9919, #26856, .T. ) ;
#33028 = B_SPLINE_CURVE_WITH_KNOTS ( 'NONE', 3,
 ( #20223, #25730, #12531, #5177, #27725, #2860 ),
 .UNSPECIFIED., .F., .F.,
 ( 4, 2, 4 ),
 ( 0.000000000000000000, 0.001992811738820069942, 0.003985623477640139883 ),
 .UNSPECIFIED. ) ;
#33029 = CARTESIAN_POINT ( 'NONE',  ( 23.22564588060107482, -21.93932300456764040, -1.000000000000000000 ) ) ;
#33030 = CYLINDRICAL_SURFACE ( 'NONE', #28518, 6.248999999999999666 ) ;
#33031 = ORIENTED_EDGE ( 'NONE', *, *, #15284, .F. ) ;
#33032 = CARTESIAN_POINT ( 'NONE',  ( 5.887530252753763627, -5.105578361685870981, -6.663910820542635172 ) ) ;
#33033 = CARTESIAN_POINT ( 'NONE',  ( 7.249760686538667009, -6.147671362329178102, -6.226446564517978288 ) ) ;
#33034 = ORIENTED_EDGE ( 'NONE', *, *, #17788, .F. ) ;
#33035 = DIRECTION ( 'NONE',  ( 1.000000000000000000, -0.000000000000000000, -0.000000000000000000 ) ) ;
#33037 = ORIENTED_EDGE ( 'NONE', *, *, #4219, .F. ) ;
#33036 = DIRECTION ( 'NONE',  ( 1.000000000000000000, -0.000000000000000000, 0.000000000000000000 ) ) ;
#33038 = ORIENTED_EDGE ( 'NONE', *, *, #22795, .T. ) ;
#33039 = CARTESIAN_POINT ( 'NONE',  ( 10.00000000000000000, -4.116875700062067267, -2.376879293651108060 ) ) ;
#33040 = ORIENTED_EDGE ( 'NONE', *, *, #14685, .T. ) ;
#33041 = CARTESIAN_POINT ( 'NONE',  ( 56.97280603064898941, -277.2763395528616002, -1.491740999229418829 ) ) ;
#33043 = EDGE_LOOP ( 'NONE', ( #17505, #16601, #33049, #3750, #22269 ) ) ;
#33042 = CARTESIAN_POINT ( 'NONE',  ( -53.95513674679793326, 5.522463357794191730, 1.050000000000049116 ) ) ;
#33044 = CARTESIAN_POINT ( 'NONE',  ( 5.377543748152548986, 7.892520144992435149, 1.391664247347255134 ) ) ;
#33045 = CARTESIAN_POINT ( 'NONE',  ( 3.499999999999999556, 1.459547570502463198, -6.894905428400257996 ) ) ;
#33046 = EDGE_CURVE ( 'NONE', #32312, #19070, #12608, .T. ) ;
#33047 = CARTESIAN_POINT ( 'NONE',  ( 21.36179047124926811, -21.76611816616638251, -1.413258355470295102 ) ) ;
#33048 = LINE ( 'NONE', #2122, #24188 ) ;
#33049 = ORIENTED_EDGE ( 'NONE', *, *, #32998, .F. ) ;
#33050 = DIRECTION ( 'NONE',  ( -1.000000000000000000, 2.473959037481237219E-13, -0.000000000000000000 ) ) ;
#33051 = CARTESIAN_POINT ( 'NONE',  ( 107.4454455519092164, 16.41225027714849816, -1.478824073157309016 ) ) ;
#33052 = ADVANCED_FACE ( 'NONE', ( #14641 ), #9952, .T. ) ;
#33053 = DIRECTION ( 'NONE',  ( 0.000000000000000000, 0.8191520442889956843, -0.5735764363510406083 ) ) ;
#33054 = DIRECTION ( 'NONE',  ( -1.000000000000000000, 8.574039729943018344E-17, -0.000000000000000000 ) ) ;
#33055 = CARTESIAN_POINT ( 'NONE',  ( -8.000050800000002127, -1.808230216471487184, 2.469696313123094011 ) ) ;
#33056 = CARTESIAN_POINT ( 'NONE',  ( 24.26973362692477920, -17.42849669161047288, -1.479847483348366355 ) ) ;
#33057 = CARTESIAN_POINT ( 'NONE',  ( 24.23500000273118715, 2.486304738420679783, -0.2613211581691337604 ) ) ;
#33058 = DIRECTION ( 'NONE',  ( 1.000000000000000000, 0.000000000000000000, 0.000000000000000000 ) ) ;
#33059 = VERTEX_POINT ( 'NONE', #22682 ) ;
#33060 = EDGE_CURVE ( 'NONE', #25199, #17653, #22597, .T. ) ;
#33061 = CARTESIAN_POINT ( 'NONE',  ( -5.962550801365593678, -2.752080473201636845, 2.228590825266444586 ) ) ;
#33062 = ORIENTED_EDGE ( 'NONE', *, *, #1917, .T. ) ;
#33063 = CARTESIAN_POINT ( 'NONE',  ( -5.154531657079158613, 3.105402419394639235, -0.9198621039125850496 ) ) ;
#33064 = CARTESIAN_POINT ( 'NONE',  ( 24.04750000136559507, -1.913930629741527500, 2.363507492473149618 ) ) ;
#33065 = FACE_OUTER_BOUND ( 'NONE', #20137, .T. ) ;
#33066 = ADVANCED_FACE ( 'NONE', ( #30037 ), #17765, .F. ) ;
#33067 = CARTESIAN_POINT ( 'NONE',  ( 0.1483196811915227509, -7.185865554061074967, 1.774508006492702128 ) ) ;
#33068 = DIRECTION ( 'NONE',  ( -1.000000000000000000, -0.000000000000000000, -0.000000000000000000 ) ) ;
#33069 = EDGE_LOOP ( 'NONE', ( #14114, #5588, #16120, #1179 ) ) ;
#33070 = CARTESIAN_POINT ( 'NONE',  ( 3.499999999999999556, -6.106419733535023653, 3.518755179752782958 ) ) ;
#33071 = EDGE_CURVE ( 'NONE', #5967, #28234, #30081, .T. ) ;
#33072 = CARTESIAN_POINT ( 'NONE',  ( 23.84310522038038727, -4.329614468550014195, -4.522129901861162260 ) ) ;
#33073 = ORIENTED_EDGE ( 'NONE', *, *, #12415, .F. ) ;
#33074 = CARTESIAN_POINT ( 'NONE',  ( -3.550050800000000173, 3.113457007523260156, -0.9222479816126439855 ) ) ;
#33075 = DATE_AND_TIME ( #27565, #234 ) ;
#33076 = CARTESIAN_POINT ( 'NONE',  ( 40.88380423908032668, -6.862032121010850361, 4.043900193569005985 ) ) ;
#33077 = EDGE_CURVE ( 'NONE', #25919, #16275, #21115, .T. ) ;
#33078 = PLANE ( 'NONE',  #5376 ) ;
#33080 = CARTESIAN_POINT ( 'NONE',  ( 3.499999999999999556, 2.429606751577043422, 5.757344182232919216 ) ) ;
#33079 = CARTESIAN_POINT ( 'NONE',  ( 108.9970757964848076, 18.07279684343247439, -5.421406142183877286 ) ) ;
#33081 = VERTEX_POINT ( 'NONE', #30534 ) ;
#33082 = CARTESIAN_POINT ( 'NONE',  ( -7.998722633285748174, -2.371517779863575370, 1.837526800715260533 ) ) ;
#33083 = CARTESIAN_POINT ( 'NONE',  ( 3.020080146450412784, 0.5244911560323111122, 8.942241244976923298 ) ) ;
#33084 = CARTESIAN_POINT ( 'NONE',  ( 23.29750000136559862, -2.363507492473152283, -1.913930629741525280 ) ) ;
#33085 = EDGE_CURVE ( 'NONE', #27844, #4589, #29518, .T. ) ;
#33086 = CARTESIAN_POINT ( 'NONE',  ( 14.67783075693927408, -16.02377530647586923, -1.500000000000000222 ) ) ;
#33087 = AXIS2_PLACEMENT_3D ( 'NONE', #14640, #14449, #12469 ) ;
#33089 = ORIENTED_EDGE ( 'NONE', *, *, #23075, .T. ) ;
#33088 = CARTESIAN_POINT ( 'NONE',  ( -1.170068671574864494, -6.059534462705076230, 4.522129901861157819 ) ) ;
#33090 = CARTESIAN_POINT ( 'NONE',  ( -6.412550801365592967, 1.828967928396027176, -3.368539882008727115 ) ) ;
#33091 = DIRECTION ( 'NONE',  ( -1.000000000000000000, 0.000000000000000000, 0.000000000000000000 ) ) ;
#33092 = CIRCLE ( 'NONE', #9022, 6.248999999999998778 ) ;
#33093 = CARTESIAN_POINT ( 'NONE',  ( 6.530491751506349196, -7.017944781891989336, 5.074604403564646482 ) ) ;
#33094 = DIRECTION ( 'NONE',  ( 0.000000000000000000, 0.000000000000000000, 1.000000000000000000 ) ) ;
#33095 = ORIENTED_EDGE ( 'NONE', *, *, #11152, .F. ) ;
#33096 = CARTESIAN_POINT ( 'NONE',  ( 23.74728587540910496, -17.43182369245540286, 1.598909884664836856 ) ) ;
#33097 = DIRECTION ( 'NONE',  ( -1.000000000000000000, 0.000000000000000000, 0.000000000000000000 ) ) ;
#33098 = NEXT_ASSEMBLY_USAGE_OCCURRENCE ( 'NAUO1', ' ', ' ', #1899, #32113, $ ) ;
#33099 = NEXT_ASSEMBLY_USAGE_OCCURRENCE ( 'NAUO2', ' ', ' ', #1899, #2068, $ ) ;
#33100 = NEXT_ASSEMBLY_USAGE_OCCURRENCE ( 'NAUO3', ' ', ' ', #1899, #25774, $ ) ;
#33101 = NEXT_ASSEMBLY_USAGE_OCCURRENCE ( 'NAUO4', ' ', ' ', #1899, #31711, $ ) ;
#33102 = NEXT_ASSEMBLY_USAGE_OCCURRENCE ( 'NAUO5', ' ', ' ', #1899, #28213, $ ) ;
#33103 = NEXT_ASSEMBLY_USAGE_OCCURRENCE ( 'NAUO6', ' ', ' ', #1899, #1036, $ ) ;
#33104 = NEXT_ASSEMBLY_USAGE_OCCURRENCE ( 'NAUO7', ' ', ' ', #1899, #21105, $ ) ;
#33105 = NEXT_ASSEMBLY_USAGE_OCCURRENCE ( 'NAUO8', ' ', ' ', #1899, #23132, $ ) ;
#33106 = COLOUR_RGB('Deep Blue', 0.66274510, 0.83137255, 0.94901961);
#33107 = FILL_AREA_STYLE_COLOUR('',#33106);
#33108 = FILL_AREA_STYLE('',(#33107));
#33109 = SURFACE_STYLE_FILL_AREA(#33108);
#33110 = SURFACE_SIDE_STYLE('',(#33109));
#33111 = SURFACE_STYLE_USAGE(.BOTH.,#33110);
#33112 = PRESENTATION_STYLE_ASSIGNMENT((#33111));
#33113 = COLOUR_RGB('Light Blue', 0.31764706, 0.68627451, 0.89019608);
#33114 = FILL_AREA_STYLE_COLOUR('',#33113);
#33115 = FILL_AREA_STYLE('',(#33114));
#33116 = SURFACE_STYLE_FILL_AREA(#33115);
#33117 = SURFACE_SIDE_STYLE('',(#33116));
#33118 = SURFACE_STYLE_USAGE(.BOTH.,#33117);
#33119 = PRESENTATION_STYLE_ASSIGNMENT((#33118));
#33120 = COLOUR_RGB('Sky Blue', 0.40784314, 0.44705882, 0.49803922);
#33121 = FILL_AREA_STYLE_COLOUR('',#33120);
#33122 = FILL_AREA_STYLE('',(#33121));
#33123 = SURFACE_STYLE_FILL_AREA(#33122);
#33124 = SURFACE_SIDE_STYLE('',(#33123));
#33125 = SURFACE_STYLE_USAGE(.BOTH.,#33124);
#33126 = PRESENTATION_STYLE_ASSIGNMENT((#33125));
#33127 = COLOUR_RGB('Slate Gray', 0.72549020, 0.75294118, 0.79215686);
#33128 = FILL_AREA_STYLE_COLOUR('',#33127);
#33129 = FILL_AREA_STYLE('',(#33128));
#33130 = SURFACE_STYLE_FILL_AREA(#33129);
#33131 = SURFACE_SIDE_STYLE('',(#33130));
#33132 = SURFACE_STYLE_USAGE(.BOTH.,#33131);
#33133 = PRESENTATION_STYLE_ASSIGNMENT((#33132));
#33134 = COLOUR_RGB('Light Gray', 0.08235294, 0.09019608, 0.10196078);
#33135 = FILL_AREA_STYLE_COLOUR('',#33134);
#33136 = FILL_AREA_STYLE('',(#33135));
#33137 = SURFACE_STYLE_FILL_AREA(#33136);
#33138 = SURFACE_SIDE_STYLE('',(#33137));
#33139 = SURFACE_STYLE_USAGE(.BOTH.,#33138);
#33140 = PRESENTATION_STYLE_ASSIGNMENT((#33139));
#33141 = COLOUR_RGB('Black', 0.09019608, 0.27058824, 0.51372549);
#33142 = FILL_AREA_STYLE_COLOUR('',#33141);
#33143 = FILL_AREA_STYLE('',(#33142));
#33144 = SURFACE_STYLE_FILL_AREA(#33143);
#33145 = SURFACE_SIDE_STYLE('',(#33144));
#33146 = SURFACE_STYLE_USAGE(.BOTH.,#33145);
#33147 = PRESENTATION_STYLE_ASSIGNMENT((#33146));
#33148 = STYLED_ITEM('',(#33112),#9961);
#33149 = MECHANICAL_DESIGN_GEOMETRIC_PRESENTATION_REPRESENTATION('',(#33148),#30610);
#33150 = STYLED_ITEM('',(#33147),#21573);
#33151 = MECHANICAL_DESIGN_GEOMETRIC_PRESENTATION_REPRESENTATION('',(#33150),#8690);
#33152 = STYLED_ITEM('',(#33126),#10515);
#33153 = MECHANICAL_DESIGN_GEOMETRIC_PRESENTATION_REPRESENTATION('',(#33152),#32200);
#33154 = STYLED_ITEM('',(#33140),#21237);
#33155 = MECHANICAL_DESIGN_GEOMETRIC_PRESENTATION_REPRESENTATION('',(#33154),#13509);
#33156 = STYLED_ITEM('',(#33119),#10233);
#33157 = MECHANICAL_DESIGN_GEOMETRIC_PRESENTATION_REPRESENTATION('',(#33156),#179);
#33158 = STYLED_ITEM('',(#33133),#10563);
#33159 = MECHANICAL_DESIGN_GEOMETRIC_PRESENTATION_REPRESENTATION('',(#33158),#7630);
#33160 = STYLED_ITEM('',(#33112),#32130);
#33161 = MECHANICAL_DESIGN_GEOMETRIC_PRESENTATION_REPRESENTATION('',(#33160),#21519);
#33162 = STYLED_ITEM('',(#33119),#32572);
#33163 = MECHANICAL_DESIGN_GEOMETRIC_PRESENTATION_REPRESENTATION('',(#33162),#7102);
ENDSEC;
END-ISO-10303-21;
